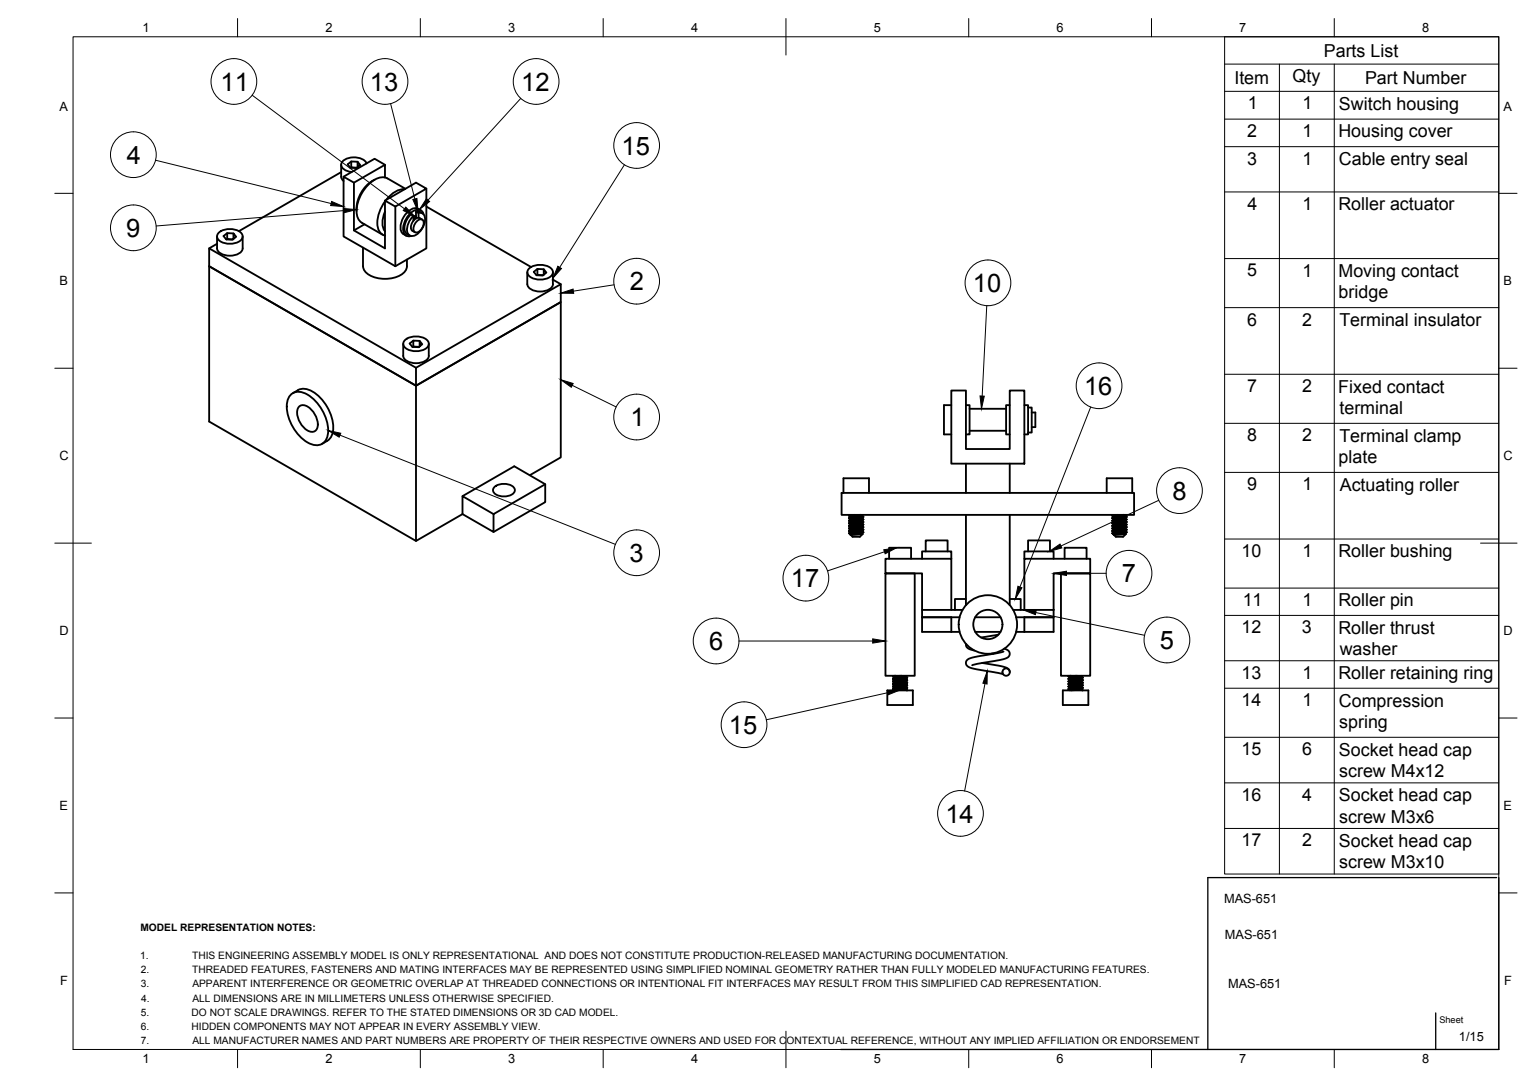
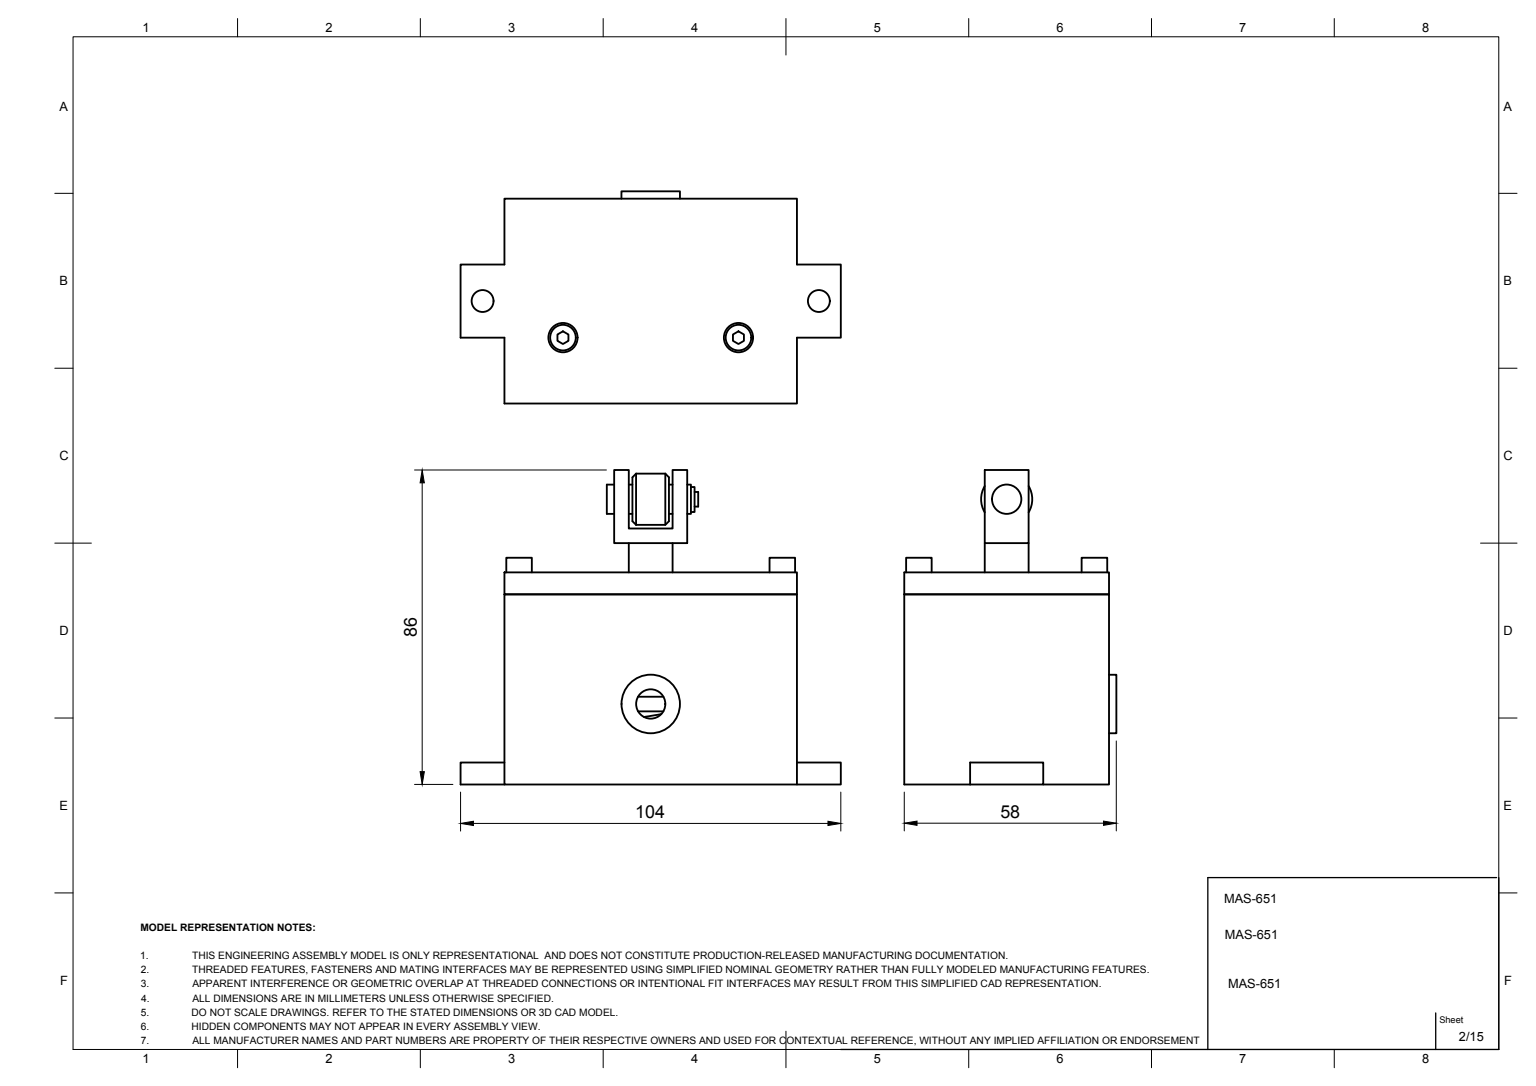
ISO-10303-21;
HEADER;
/* Generated by software containing ST-Developer
 * from STEP Tools, Inc. (www.steptools.com) 
 */

FILE_DESCRIPTION(
/* description */ ('Independent direct-acting normally-closed roller-plunger limit-switch
 CAD. Removable cover, insulated terminal supports, captured bus/conta
ct bridge, native Coil return spring, integral lower travel stop, reus
able instanced hardware and free roller. Manual geometric contact open
ing4mm; no snap-action/contact-force, electrical/current/voltage, envi
ronmental seal, safety-switch, wear, load or life certification. Exter
nal wiring and anchors omitted; fits and application engineering requi
red.'),
/* implementation_level */ '2;1');

FILE_NAME(
/* name */ 'MAS-651.step',
/* time_stamp */ '2026-11-08T07:32:43-08:00',
/* author */ (''),
/* organization */ (''),
/* preprocessor_version */ 'ST-DEVELOPER v20.2',
/* originating_system */ 'Autodesk Translation Framework v15.17.0.0',
/* authorisation */ '');

FILE_SCHEMA (('AUTOMOTIVE_DESIGN { 1 0 10303 214 3 1 1 }'));
ENDSEC;

DATA;
#10=MECHANICAL_DESIGN_GEOMETRIC_PRESENTATION_REPRESENTATION('',(#176,#177,
#178,#179,#180,#181,#182,#183,#184,#185,#186,#187,#188,#189,#190,#191,#192),
#36482);
#11=ITEM_DEFINED_TRANSFORMATION($,$,#9973,#10659);
#12=ITEM_DEFINED_TRANSFORMATION($,$,#10172,#10660);
#13=ITEM_DEFINED_TRANSFORMATION($,$,#10194,#10661);
#14=ITEM_DEFINED_TRANSFORMATION($,$,#10207,#10662);
#15=ITEM_DEFINED_TRANSFORMATION($,$,#10284,#10663);
#16=ITEM_DEFINED_TRANSFORMATION($,$,#10314,#10664);
#17=ITEM_DEFINED_TRANSFORMATION($,$,#10401,#10665);
#18=ITEM_DEFINED_TRANSFORMATION($,$,#10443,#10666);
#19=ITEM_DEFINED_TRANSFORMATION($,$,#10297,#10667);
#20=ITEM_DEFINED_TRANSFORMATION($,$,#10314,#10668);
#21=ITEM_DEFINED_TRANSFORMATION($,$,#10401,#10669);
#22=ITEM_DEFINED_TRANSFORMATION($,$,#10443,#10670);
#23=ITEM_DEFINED_TRANSFORMATION($,$,#10453,#10671);
#24=ITEM_DEFINED_TRANSFORMATION($,$,#10462,#10672);
#25=ITEM_DEFINED_TRANSFORMATION($,$,#10496,#10673);
#26=ITEM_DEFINED_TRANSFORMATION($,$,#10480,#10674);
#27=ITEM_DEFINED_TRANSFORMATION($,$,#10491,#10675);
#28=ITEM_DEFINED_TRANSFORMATION($,$,#10496,#10676);
#29=ITEM_DEFINED_TRANSFORMATION($,$,#10496,#10677);
#30=ITEM_DEFINED_TRANSFORMATION($,$,#10505,#10678);
#31=ITEM_DEFINED_TRANSFORMATION($,$,#10559,#10679);
#32=ITEM_DEFINED_TRANSFORMATION($,$,#10601,#10680);
#33=ITEM_DEFINED_TRANSFORMATION($,$,#10505,#10681);
#34=ITEM_DEFINED_TRANSFORMATION($,$,#10505,#10682);
#35=ITEM_DEFINED_TRANSFORMATION($,$,#10505,#10683);
#36=ITEM_DEFINED_TRANSFORMATION($,$,#10505,#10684);
#37=ITEM_DEFINED_TRANSFORMATION($,$,#10505,#10685);
#38=ITEM_DEFINED_TRANSFORMATION($,$,#10559,#10686);
#39=ITEM_DEFINED_TRANSFORMATION($,$,#10559,#10687);
#40=ITEM_DEFINED_TRANSFORMATION($,$,#10559,#10688);
#41=ITEM_DEFINED_TRANSFORMATION($,$,#10601,#10689);
#42=(
REPRESENTATION_RELATIONSHIP($,$,#36555,#36554)
REPRESENTATION_RELATIONSHIP_WITH_TRANSFORMATION(#11)
SHAPE_REPRESENTATION_RELATIONSHIP()
);
#43=(
REPRESENTATION_RELATIONSHIP($,$,#36556,#36554)
REPRESENTATION_RELATIONSHIP_WITH_TRANSFORMATION(#12)
SHAPE_REPRESENTATION_RELATIONSHIP()
);
#44=(
REPRESENTATION_RELATIONSHIP($,$,#36557,#36554)
REPRESENTATION_RELATIONSHIP_WITH_TRANSFORMATION(#13)
SHAPE_REPRESENTATION_RELATIONSHIP()
);
#45=(
REPRESENTATION_RELATIONSHIP($,$,#36558,#36554)
REPRESENTATION_RELATIONSHIP_WITH_TRANSFORMATION(#14)
SHAPE_REPRESENTATION_RELATIONSHIP()
);
#46=(
REPRESENTATION_RELATIONSHIP($,$,#36559,#36554)
REPRESENTATION_RELATIONSHIP_WITH_TRANSFORMATION(#15)
SHAPE_REPRESENTATION_RELATIONSHIP()
);
#47=(
REPRESENTATION_RELATIONSHIP($,$,#36561,#36554)
REPRESENTATION_RELATIONSHIP_WITH_TRANSFORMATION(#16)
SHAPE_REPRESENTATION_RELATIONSHIP()
);
#48=(
REPRESENTATION_RELATIONSHIP($,$,#36562,#36554)
REPRESENTATION_RELATIONSHIP_WITH_TRANSFORMATION(#17)
SHAPE_REPRESENTATION_RELATIONSHIP()
);
#49=(
REPRESENTATION_RELATIONSHIP($,$,#36563,#36554)
REPRESENTATION_RELATIONSHIP_WITH_TRANSFORMATION(#18)
SHAPE_REPRESENTATION_RELATIONSHIP()
);
#50=(
REPRESENTATION_RELATIONSHIP($,$,#36560,#36554)
REPRESENTATION_RELATIONSHIP_WITH_TRANSFORMATION(#19)
SHAPE_REPRESENTATION_RELATIONSHIP()
);
#51=(
REPRESENTATION_RELATIONSHIP($,$,#36561,#36554)
REPRESENTATION_RELATIONSHIP_WITH_TRANSFORMATION(#20)
SHAPE_REPRESENTATION_RELATIONSHIP()
);
#52=(
REPRESENTATION_RELATIONSHIP($,$,#36562,#36554)
REPRESENTATION_RELATIONSHIP_WITH_TRANSFORMATION(#21)
SHAPE_REPRESENTATION_RELATIONSHIP()
);
#53=(
REPRESENTATION_RELATIONSHIP($,$,#36563,#36554)
REPRESENTATION_RELATIONSHIP_WITH_TRANSFORMATION(#22)
SHAPE_REPRESENTATION_RELATIONSHIP()
);
#54=(
REPRESENTATION_RELATIONSHIP($,$,#36564,#36554)
REPRESENTATION_RELATIONSHIP_WITH_TRANSFORMATION(#23)
SHAPE_REPRESENTATION_RELATIONSHIP()
);
#55=(
REPRESENTATION_RELATIONSHIP($,$,#36565,#36554)
REPRESENTATION_RELATIONSHIP_WITH_TRANSFORMATION(#24)
SHAPE_REPRESENTATION_RELATIONSHIP()
);
#56=(
REPRESENTATION_RELATIONSHIP($,$,#36568,#36554)
REPRESENTATION_RELATIONSHIP_WITH_TRANSFORMATION(#25)
SHAPE_REPRESENTATION_RELATIONSHIP()
);
#57=(
REPRESENTATION_RELATIONSHIP($,$,#36566,#36554)
REPRESENTATION_RELATIONSHIP_WITH_TRANSFORMATION(#26)
SHAPE_REPRESENTATION_RELATIONSHIP()
);
#58=(
REPRESENTATION_RELATIONSHIP($,$,#36567,#36554)
REPRESENTATION_RELATIONSHIP_WITH_TRANSFORMATION(#27)
SHAPE_REPRESENTATION_RELATIONSHIP()
);
#59=(
REPRESENTATION_RELATIONSHIP($,$,#36568,#36554)
REPRESENTATION_RELATIONSHIP_WITH_TRANSFORMATION(#28)
SHAPE_REPRESENTATION_RELATIONSHIP()
);
#60=(
REPRESENTATION_RELATIONSHIP($,$,#36568,#36554)
REPRESENTATION_RELATIONSHIP_WITH_TRANSFORMATION(#29)
SHAPE_REPRESENTATION_RELATIONSHIP()
);
#61=(
REPRESENTATION_RELATIONSHIP($,$,#36569,#36554)
REPRESENTATION_RELATIONSHIP_WITH_TRANSFORMATION(#30)
SHAPE_REPRESENTATION_RELATIONSHIP()
);
#62=(
REPRESENTATION_RELATIONSHIP($,$,#36570,#36554)
REPRESENTATION_RELATIONSHIP_WITH_TRANSFORMATION(#31)
SHAPE_REPRESENTATION_RELATIONSHIP()
);
#63=(
REPRESENTATION_RELATIONSHIP($,$,#36571,#36554)
REPRESENTATION_RELATIONSHIP_WITH_TRANSFORMATION(#32)
SHAPE_REPRESENTATION_RELATIONSHIP()
);
#64=(
REPRESENTATION_RELATIONSHIP($,$,#36569,#36554)
REPRESENTATION_RELATIONSHIP_WITH_TRANSFORMATION(#33)
SHAPE_REPRESENTATION_RELATIONSHIP()
);
#65=(
REPRESENTATION_RELATIONSHIP($,$,#36569,#36554)
REPRESENTATION_RELATIONSHIP_WITH_TRANSFORMATION(#34)
SHAPE_REPRESENTATION_RELATIONSHIP()
);
#66=(
REPRESENTATION_RELATIONSHIP($,$,#36569,#36554)
REPRESENTATION_RELATIONSHIP_WITH_TRANSFORMATION(#35)
SHAPE_REPRESENTATION_RELATIONSHIP()
);
#67=(
REPRESENTATION_RELATIONSHIP($,$,#36569,#36554)
REPRESENTATION_RELATIONSHIP_WITH_TRANSFORMATION(#36)
SHAPE_REPRESENTATION_RELATIONSHIP()
);
#68=(
REPRESENTATION_RELATIONSHIP($,$,#36569,#36554)
REPRESENTATION_RELATIONSHIP_WITH_TRANSFORMATION(#37)
SHAPE_REPRESENTATION_RELATIONSHIP()
);
#69=(
REPRESENTATION_RELATIONSHIP($,$,#36570,#36554)
REPRESENTATION_RELATIONSHIP_WITH_TRANSFORMATION(#38)
SHAPE_REPRESENTATION_RELATIONSHIP()
);
#70=(
REPRESENTATION_RELATIONSHIP($,$,#36570,#36554)
REPRESENTATION_RELATIONSHIP_WITH_TRANSFORMATION(#39)
SHAPE_REPRESENTATION_RELATIONSHIP()
);
#71=(
REPRESENTATION_RELATIONSHIP($,$,#36570,#36554)
REPRESENTATION_RELATIONSHIP_WITH_TRANSFORMATION(#40)
SHAPE_REPRESENTATION_RELATIONSHIP()
);
#72=(
REPRESENTATION_RELATIONSHIP($,$,#36571,#36554)
REPRESENTATION_RELATIONSHIP_WITH_TRANSFORMATION(#41)
SHAPE_REPRESENTATION_RELATIONSHIP()
);
#73=CONTEXT_DEPENDENT_SHAPE_REPRESENTATION(#42,#36523);
#74=CONTEXT_DEPENDENT_SHAPE_REPRESENTATION(#43,#36524);
#75=CONTEXT_DEPENDENT_SHAPE_REPRESENTATION(#44,#36525);
#76=CONTEXT_DEPENDENT_SHAPE_REPRESENTATION(#45,#36526);
#77=CONTEXT_DEPENDENT_SHAPE_REPRESENTATION(#46,#36527);
#78=CONTEXT_DEPENDENT_SHAPE_REPRESENTATION(#47,#36528);
#79=CONTEXT_DEPENDENT_SHAPE_REPRESENTATION(#48,#36529);
#80=CONTEXT_DEPENDENT_SHAPE_REPRESENTATION(#49,#36530);
#81=CONTEXT_DEPENDENT_SHAPE_REPRESENTATION(#50,#36531);
#82=CONTEXT_DEPENDENT_SHAPE_REPRESENTATION(#51,#36532);
#83=CONTEXT_DEPENDENT_SHAPE_REPRESENTATION(#52,#36533);
#84=CONTEXT_DEPENDENT_SHAPE_REPRESENTATION(#53,#36534);
#85=CONTEXT_DEPENDENT_SHAPE_REPRESENTATION(#54,#36535);
#86=CONTEXT_DEPENDENT_SHAPE_REPRESENTATION(#55,#36536);
#87=CONTEXT_DEPENDENT_SHAPE_REPRESENTATION(#56,#36537);
#88=CONTEXT_DEPENDENT_SHAPE_REPRESENTATION(#57,#36538);
#89=CONTEXT_DEPENDENT_SHAPE_REPRESENTATION(#58,#36539);
#90=CONTEXT_DEPENDENT_SHAPE_REPRESENTATION(#59,#36540);
#91=CONTEXT_DEPENDENT_SHAPE_REPRESENTATION(#60,#36541);
#92=CONTEXT_DEPENDENT_SHAPE_REPRESENTATION(#61,#36542);
#93=CONTEXT_DEPENDENT_SHAPE_REPRESENTATION(#62,#36543);
#94=CONTEXT_DEPENDENT_SHAPE_REPRESENTATION(#63,#36544);
#95=CONTEXT_DEPENDENT_SHAPE_REPRESENTATION(#64,#36545);
#96=CONTEXT_DEPENDENT_SHAPE_REPRESENTATION(#65,#36546);
#97=CONTEXT_DEPENDENT_SHAPE_REPRESENTATION(#66,#36547);
#98=CONTEXT_DEPENDENT_SHAPE_REPRESENTATION(#67,#36548);
#99=CONTEXT_DEPENDENT_SHAPE_REPRESENTATION(#68,#36549);
#100=CONTEXT_DEPENDENT_SHAPE_REPRESENTATION(#69,#36550);
#101=CONTEXT_DEPENDENT_SHAPE_REPRESENTATION(#70,#36551);
#102=CONTEXT_DEPENDENT_SHAPE_REPRESENTATION(#71,#36552);
#103=CONTEXT_DEPENDENT_SHAPE_REPRESENTATION(#72,#36553);
#104=NEXT_ASSEMBLY_USAGE_OCCURRENCE('Switch housing:1',
'Switch housing:1','Switch housing:1',#36573,#36574,'Switch housing:1');
#105=NEXT_ASSEMBLY_USAGE_OCCURRENCE('Housing cover:1','Housing cover:1',
'Housing cover:1',#36573,#36575,'Housing cover:1');
#106=NEXT_ASSEMBLY_USAGE_OCCURRENCE('Cable entry seal:1',
'Cable entry seal:1','Cable entry seal:1',#36573,#36576,
'Cable entry seal:1');
#107=NEXT_ASSEMBLY_USAGE_OCCURRENCE('Roller actuator:1',
'Roller actuator:1','Roller actuator:1',#36573,#36577,
'Roller actuator:1');
#108=NEXT_ASSEMBLY_USAGE_OCCURRENCE('Moving contact bridge:1',
'Moving contact bridge:1','Moving contact bridge:1',#36573,#36578,
'Moving contact bridge:1');
#109=NEXT_ASSEMBLY_USAGE_OCCURRENCE('Terminal insulator:1',
'Terminal insulator:1','Terminal insulator:1',#36573,#36580,
'Terminal insulator:1');
#110=NEXT_ASSEMBLY_USAGE_OCCURRENCE('Fixed contact terminal:1',
'Fixed contact terminal:1','Fixed contact terminal:1',#36573,#36581,
'Fixed contact terminal:1');
#111=NEXT_ASSEMBLY_USAGE_OCCURRENCE('Terminal clamp plate:1',
'Terminal clamp plate:1','Terminal clamp plate:1',#36573,#36582,
'Terminal clamp plate:1');
#112=NEXT_ASSEMBLY_USAGE_OCCURRENCE('Actuating roller:1',
'Actuating roller:1','Actuating roller:1',#36573,#36579,
'Actuating roller:1');
#113=NEXT_ASSEMBLY_USAGE_OCCURRENCE('Terminal insulator:2',
'Terminal insulator:2','Terminal insulator:2',#36573,#36580,
'Terminal insulator:2');
#114=NEXT_ASSEMBLY_USAGE_OCCURRENCE('Fixed contact terminal:2',
'Fixed contact terminal:2','Fixed contact terminal:2',#36573,#36581,
'Fixed contact terminal:2');
#115=NEXT_ASSEMBLY_USAGE_OCCURRENCE('Terminal clamp plate:2',
'Terminal clamp plate:2','Terminal clamp plate:2',#36573,#36582,
'Terminal clamp plate:2');
#116=NEXT_ASSEMBLY_USAGE_OCCURRENCE('Roller bushing:1',
'Roller bushing:1','Roller bushing:1',#36573,#36583,'Roller bushing:1');
#117=NEXT_ASSEMBLY_USAGE_OCCURRENCE('Roller pin:1','Roller pin:1',
'Roller pin:1',#36573,#36584,'Roller pin:1');
#118=NEXT_ASSEMBLY_USAGE_OCCURRENCE('Roller thrust washer:1',
'Roller thrust washer:1','Roller thrust washer:1',#36573,#36587,
'Roller thrust washer:1');
#119=NEXT_ASSEMBLY_USAGE_OCCURRENCE('Roller retaining ring:1',
'Roller retaining ring:1','Roller retaining ring:1',#36573,#36585,
'Roller retaining ring:1');
#120=NEXT_ASSEMBLY_USAGE_OCCURRENCE('Compression spring:1',
'Compression spring:1','Compression spring:1',#36573,#36586,
'Compression spring:1');
#121=NEXT_ASSEMBLY_USAGE_OCCURRENCE('Roller thrust washer:2',
'Roller thrust washer:2','Roller thrust washer:2',#36573,#36587,
'Roller thrust washer:2');
#122=NEXT_ASSEMBLY_USAGE_OCCURRENCE('Roller thrust washer:3',
'Roller thrust washer:3','Roller thrust washer:3',#36573,#36587,
'Roller thrust washer:3');
#123=NEXT_ASSEMBLY_USAGE_OCCURRENCE('Socket head cap screw M4x12:1',
'Socket head cap screw M4x12:1','Socket head cap screw M4x12:1',#36573,
#36588,'Socket head cap screw M4x12:1');
#124=NEXT_ASSEMBLY_USAGE_OCCURRENCE('Socket head cap screw M3x6:1',
'Socket head cap screw M3x6:1','Socket head cap screw M3x6:1',#36573,#36589,
'Socket head cap screw M3x6:1');
#125=NEXT_ASSEMBLY_USAGE_OCCURRENCE('Socket head cap screw M3x10:1',
'Socket head cap screw M3x10:1','Socket head cap screw M3x10:1',#36573,
#36590,'Socket head cap screw M3x10:1');
#126=NEXT_ASSEMBLY_USAGE_OCCURRENCE('Socket head cap screw M4x12:2',
'Socket head cap screw M4x12:2','Socket head cap screw M4x12:2',#36573,
#36588,'Socket head cap screw M4x12:2');
#127=NEXT_ASSEMBLY_USAGE_OCCURRENCE('Socket head cap screw M4x12:3',
'Socket head cap screw M4x12:3','Socket head cap screw M4x12:3',#36573,
#36588,'Socket head cap screw M4x12:3');
#128=NEXT_ASSEMBLY_USAGE_OCCURRENCE('Socket head cap screw M4x12:4',
'Socket head cap screw M4x12:4','Socket head cap screw M4x12:4',#36573,
#36588,'Socket head cap screw M4x12:4');
#129=NEXT_ASSEMBLY_USAGE_OCCURRENCE('Socket head cap screw M4x12:5',
'Socket head cap screw M4x12:5','Socket head cap screw M4x12:5',#36573,
#36588,'Socket head cap screw M4x12:5');
#130=NEXT_ASSEMBLY_USAGE_OCCURRENCE('Socket head cap screw M4x12:6',
'Socket head cap screw M4x12:6','Socket head cap screw M4x12:6',#36573,
#36588,'Socket head cap screw M4x12:6');
#131=NEXT_ASSEMBLY_USAGE_OCCURRENCE('Socket head cap screw M3x6:2',
'Socket head cap screw M3x6:2','Socket head cap screw M3x6:2',#36573,#36589,
'Socket head cap screw M3x6:2');
#132=NEXT_ASSEMBLY_USAGE_OCCURRENCE('Socket head cap screw M3x6:3',
'Socket head cap screw M3x6:3','Socket head cap screw M3x6:3',#36573,#36589,
'Socket head cap screw M3x6:3');
#133=NEXT_ASSEMBLY_USAGE_OCCURRENCE('Socket head cap screw M3x6:4',
'Socket head cap screw M3x6:4','Socket head cap screw M3x6:4',#36573,#36589,
'Socket head cap screw M3x6:4');
#134=NEXT_ASSEMBLY_USAGE_OCCURRENCE('Socket head cap screw M3x10:2',
'Socket head cap screw M3x10:2','Socket head cap screw M3x10:2',#36573,
#36590,'Socket head cap screw M3x10:2');
#135=CONICAL_SURFACE('',#10298,0.65,0.785398163397448);
#136=CONICAL_SURFACE('',#10305,0.65,0.785398163397448);
#137=CONICAL_SURFACE('',#10309,0.35,0.785398163397448);
#138=CONICAL_SURFACE('',#10313,0.35,0.785398163397448);
#139=CONICAL_SURFACE('',#10540,0.15,0.785398163397449);
#140=CONICAL_SURFACE('',#10582,0.1,0.785398163397448);
#141=CONICAL_SURFACE('',#10640,0.1,0.785398163397448);
#142=SHAPE_REPRESENTATION_RELATIONSHIP('SRR','None',#36555,#159);
#143=SHAPE_REPRESENTATION_RELATIONSHIP('SRR','None',#36556,#160);
#144=SHAPE_REPRESENTATION_RELATIONSHIP('SRR','None',#36557,#161);
#145=SHAPE_REPRESENTATION_RELATIONSHIP('SRR','None',#36558,#162);
#146=SHAPE_REPRESENTATION_RELATIONSHIP('SRR','None',#36559,#163);
#147=SHAPE_REPRESENTATION_RELATIONSHIP('SRR','None',#36560,#164);
#148=SHAPE_REPRESENTATION_RELATIONSHIP('SRR','None',#36561,#165);
#149=SHAPE_REPRESENTATION_RELATIONSHIP('SRR','None',#36562,#166);
#150=SHAPE_REPRESENTATION_RELATIONSHIP('SRR','None',#36563,#167);
#151=SHAPE_REPRESENTATION_RELATIONSHIP('SRR','None',#36564,#168);
#152=SHAPE_REPRESENTATION_RELATIONSHIP('SRR','None',#36565,#169);
#153=SHAPE_REPRESENTATION_RELATIONSHIP('SRR','None',#36566,#170);
#154=SHAPE_REPRESENTATION_RELATIONSHIP('SRR','None',#36567,#171);
#155=SHAPE_REPRESENTATION_RELATIONSHIP('SRR','None',#36568,#172);
#156=SHAPE_REPRESENTATION_RELATIONSHIP('SRR','None',#36569,#173);
#157=SHAPE_REPRESENTATION_RELATIONSHIP('SRR','None',#36570,#174);
#158=SHAPE_REPRESENTATION_RELATIONSHIP('SRR','None',#36571,#175);
#159=ADVANCED_BREP_SHAPE_REPRESENTATION('',(#193),#36465);
#160=ADVANCED_BREP_SHAPE_REPRESENTATION('',(#194),#36466);
#161=ADVANCED_BREP_SHAPE_REPRESENTATION('',(#195),#36467);
#162=ADVANCED_BREP_SHAPE_REPRESENTATION('',(#196),#36468);
#163=ADVANCED_BREP_SHAPE_REPRESENTATION('',(#197),#36469);
#164=ADVANCED_BREP_SHAPE_REPRESENTATION('',(#198),#36470);
#165=ADVANCED_BREP_SHAPE_REPRESENTATION('',(#199),#36471);
#166=ADVANCED_BREP_SHAPE_REPRESENTATION('',(#200),#36472);
#167=ADVANCED_BREP_SHAPE_REPRESENTATION('',(#201),#36473);
#168=ADVANCED_BREP_SHAPE_REPRESENTATION('',(#202),#36474);
#169=ADVANCED_BREP_SHAPE_REPRESENTATION('',(#203),#36475);
#170=ADVANCED_BREP_SHAPE_REPRESENTATION('',(#204),#36476);
#171=ADVANCED_BREP_SHAPE_REPRESENTATION('',(#205),#36477);
#172=ADVANCED_BREP_SHAPE_REPRESENTATION('',(#206),#36478);
#173=ADVANCED_BREP_SHAPE_REPRESENTATION('',(#207),#36479);
#174=ADVANCED_BREP_SHAPE_REPRESENTATION('',(#208),#36480);
#175=ADVANCED_BREP_SHAPE_REPRESENTATION('',(#209),#36481);
#176=STYLED_ITEM('',(#36649),#193);
#177=STYLED_ITEM('',(#36650),#194);
#178=STYLED_ITEM('',(#36651),#195);
#179=STYLED_ITEM('',(#36652),#196);
#180=STYLED_ITEM('',(#36653),#197);
#181=STYLED_ITEM('',(#36654),#198);
#182=STYLED_ITEM('',(#36655),#199);
#183=STYLED_ITEM('',(#36653),#200);
#184=STYLED_ITEM('',(#36656),#201);
#185=STYLED_ITEM('',(#36657),#202);
#186=STYLED_ITEM('',(#36658),#203);
#187=STYLED_ITEM('',(#36659),#204);
#188=STYLED_ITEM('',(#36660),#205);
#189=STYLED_ITEM('',(#36661),#206);
#190=STYLED_ITEM('',(#36659),#207);
#191=STYLED_ITEM('',(#36659),#208);
#192=STYLED_ITEM('',(#36659),#209);
#193=MANIFOLD_SOLID_BREP('Body1',#9767);
#194=MANIFOLD_SOLID_BREP('Body1',#9768);
#195=MANIFOLD_SOLID_BREP('Body1',#9769);
#196=MANIFOLD_SOLID_BREP('Body1',#9770);
#197=MANIFOLD_SOLID_BREP('Body1',#9771);
#198=MANIFOLD_SOLID_BREP('Roller',#9772);
#199=MANIFOLD_SOLID_BREP('Body1',#9773);
#200=MANIFOLD_SOLID_BREP('Body1',#9774);
#201=MANIFOLD_SOLID_BREP('Body1',#9775);
#202=MANIFOLD_SOLID_BREP('Body1',#9776);
#203=MANIFOLD_SOLID_BREP('Body1',#9777);
#204=MANIFOLD_SOLID_BREP('Body1',#9778);
#205=MANIFOLD_SOLID_BREP('Body1',#9779);
#206=MANIFOLD_SOLID_BREP('Body1',#9780);
#207=MANIFOLD_SOLID_BREP('Body1',#9781);
#208=MANIFOLD_SOLID_BREP('Body1',#9782);
#209=MANIFOLD_SOLID_BREP('Body1',#9783);
#210=B_SPLINE_SURFACE_WITH_KNOTS('',3,3,((#16536,#16537,#16538,#16539,#16540,
#16541,#16542,#16543,#16544,#16545,#16546,#16547,#16548,#16549,#16550,#16551,
#16552,#16553,#16554,#16555,#16556,#16557,#16558,#16559,#16560,#16561,#16562,
#16563,#16564,#16565,#16566,#16567,#16568,#16569,#16570,#16571,#16572,#16573,
#16574,#16575,#16576,#16577,#16578,#16579,#16580,#16581,#16582,#16583,#16584,
#16585,#16586,#16587,#16588,#16589,#16590,#16591,#16592,#16593,#16594,#16595,
#16596,#16597,#16598,#16599,#16600,#16601,#16602,#16603,#16604,#16605,#16606,
#16607,#16608,#16609,#16610,#16611,#16612,#16613,#16614,#16615,#16616,#16617,
#16618,#16619,#16620,#16621),(#16622,#16623,#16624,#16625,#16626,#16627,
#16628,#16629,#16630,#16631,#16632,#16633,#16634,#16635,#16636,#16637,#16638,
#16639,#16640,#16641,#16642,#16643,#16644,#16645,#16646,#16647,#16648,#16649,
#16650,#16651,#16652,#16653,#16654,#16655,#16656,#16657,#16658,#16659,#16660,
#16661,#16662,#16663,#16664,#16665,#16666,#16667,#16668,#16669,#16670,#16671,
#16672,#16673,#16674,#16675,#16676,#16677,#16678,#16679,#16680,#16681,#16682,
#16683,#16684,#16685,#16686,#16687,#16688,#16689,#16690,#16691,#16692,#16693,
#16694,#16695,#16696,#16697,#16698,#16699,#16700,#16701,#16702,#16703,#16704,
#16705,#16706,#16707),(#16708,#16709,#16710,#16711,#16712,#16713,#16714,
#16715,#16716,#16717,#16718,#16719,#16720,#16721,#16722,#16723,#16724,#16725,
#16726,#16727,#16728,#16729,#16730,#16731,#16732,#16733,#16734,#16735,#16736,
#16737,#16738,#16739,#16740,#16741,#16742,#16743,#16744,#16745,#16746,#16747,
#16748,#16749,#16750,#16751,#16752,#16753,#16754,#16755,#16756,#16757,#16758,
#16759,#16760,#16761,#16762,#16763,#16764,#16765,#16766,#16767,#16768,#16769,
#16770,#16771,#16772,#16773,#16774,#16775,#16776,#16777,#16778,#16779,#16780,
#16781,#16782,#16783,#16784,#16785,#16786,#16787,#16788,#16789,#16790,#16791,
#16792,#16793),(#16794,#16795,#16796,#16797,#16798,#16799,#16800,#16801,
#16802,#16803,#16804,#16805,#16806,#16807,#16808,#16809,#16810,#16811,#16812,
#16813,#16814,#16815,#16816,#16817,#16818,#16819,#16820,#16821,#16822,#16823,
#16824,#16825,#16826,#16827,#16828,#16829,#16830,#16831,#16832,#16833,#16834,
#16835,#16836,#16837,#16838,#16839,#16840,#16841,#16842,#16843,#16844,#16845,
#16846,#16847,#16848,#16849,#16850,#16851,#16852,#16853,#16854,#16855,#16856,
#16857,#16858,#16859,#16860,#16861,#16862,#16863,#16864,#16865,#16866,#16867,
#16868,#16869,#16870,#16871,#16872,#16873,#16874,#16875,#16876,#16877,#16878,
#16879)),.UNSPECIFIED.,.F.,.F.,.F.,(4,4),(4,1,1,1,1,1,1,1,1,1,1,1,1,1,1,
1,1,1,1,1,1,1,1,1,1,1,1,1,1,1,1,1,1,1,1,1,1,1,1,1,1,1,1,1,1,1,1,1,1,1,1,
1,1,1,1,1,1,1,1,1,1,1,1,1,1,1,1,1,1,1,1,1,1,1,1,1,1,1,1,1,1,1,1,4),(0.,
0.0448889834294937),(11.8615800042567,12.8591513772396,13.8567227502226,
14.8542941232055,15.8518654961884,16.8494368691714,17.8470082421543,18.8445796151372,
19.8421509881202,20.8397223611031,21.837293734086,22.834865107069,23.8324364800519,
24.8300078530348,25.8275792260178,26.8251505990007,27.8227219719836,28.8202933449666,
29.8178647179495,30.8154360909324,31.8130074639154,32.8105788368983,33.8081502098812,
34.8057215828642,35.8032929558471,36.80086432883,37.798435701813,38.7960070747959,
39.7935784477789,40.7911498207618,41.7887211937447,42.7862925667277,43.7838639397106,
44.7814353126935,45.7790066856765,46.7765780586594,47.7741494316423,48.7717208046253,
49.7692921776082,50.7668635505911,51.7644349235741,52.762006296557,53.7595776695399,
54.7571490425229,55.7547204155058,56.7522917884887,57.7498631614717,58.7474345344546,
59.7450059074375,60.7425772804205,61.7401486534034,62.7377200263864,63.7352913993693,
64.7328627723522,65.7304341453352,66.7280055183181,67.725576891301,68.723148264284,
69.7207196372669,70.7182910102498,71.7158623832328,72.7134337562157,73.7110051291986,
74.7085765021816,75.7061478751645,76.7037192481474,77.7012906211304,78.6988619941133,
79.6964333670962,80.6940047400792,81.6915761130621,82.689147486045,83.686718859028,
84.6842902320109,85.6818616049939,86.6794329779768,87.6770043509597,88.6745757239427,
89.6721470969256,90.6697184699085,91.6672898428915,92.6648612158744,93.6624325888573,
94.6600039618403),.UNSPECIFIED.);
#211=B_SPLINE_SURFACE_WITH_KNOTS('',3,3,((#16957,#16958,#16959,#16960,#16961,
#16962,#16963,#16964,#16965,#16966,#16967,#16968,#16969,#16970,#16971,#16972,
#16973,#16974,#16975,#16976,#16977,#16978,#16979,#16980,#16981,#16982,#16983,
#16984,#16985,#16986,#16987,#16988,#16989,#16990,#16991,#16992,#16993,#16994,
#16995,#16996,#16997,#16998,#16999,#17000,#17001,#17002,#17003,#17004,#17005,
#17006,#17007,#17008,#17009,#17010,#17011,#17012,#17013,#17014,#17015,#17016,
#17017,#17018,#17019,#17020,#17021,#17022,#17023,#17024,#17025,#17026,#17027,
#17028,#17029,#17030,#17031,#17032,#17033,#17034,#17035,#17036,#17037,#17038,
#17039,#17040,#17041,#17042),(#17043,#17044,#17045,#17046,#17047,#17048,
#17049,#17050,#17051,#17052,#17053,#17054,#17055,#17056,#17057,#17058,#17059,
#17060,#17061,#17062,#17063,#17064,#17065,#17066,#17067,#17068,#17069,#17070,
#17071,#17072,#17073,#17074,#17075,#17076,#17077,#17078,#17079,#17080,#17081,
#17082,#17083,#17084,#17085,#17086,#17087,#17088,#17089,#17090,#17091,#17092,
#17093,#17094,#17095,#17096,#17097,#17098,#17099,#17100,#17101,#17102,#17103,
#17104,#17105,#17106,#17107,#17108,#17109,#17110,#17111,#17112,#17113,#17114,
#17115,#17116,#17117,#17118,#17119,#17120,#17121,#17122,#17123,#17124,#17125,
#17126,#17127,#17128),(#17129,#17130,#17131,#17132,#17133,#17134,#17135,
#17136,#17137,#17138,#17139,#17140,#17141,#17142,#17143,#17144,#17145,#17146,
#17147,#17148,#17149,#17150,#17151,#17152,#17153,#17154,#17155,#17156,#17157,
#17158,#17159,#17160,#17161,#17162,#17163,#17164,#17165,#17166,#17167,#17168,
#17169,#17170,#17171,#17172,#17173,#17174,#17175,#17176,#17177,#17178,#17179,
#17180,#17181,#17182,#17183,#17184,#17185,#17186,#17187,#17188,#17189,#17190,
#17191,#17192,#17193,#17194,#17195,#17196,#17197,#17198,#17199,#17200,#17201,
#17202,#17203,#17204,#17205,#17206,#17207,#17208,#17209,#17210,#17211,#17212,
#17213,#17214),(#17215,#17216,#17217,#17218,#17219,#17220,#17221,#17222,
#17223,#17224,#17225,#17226,#17227,#17228,#17229,#17230,#17231,#17232,#17233,
#17234,#17235,#17236,#17237,#17238,#17239,#17240,#17241,#17242,#17243,#17244,
#17245,#17246,#17247,#17248,#17249,#17250,#17251,#17252,#17253,#17254,#17255,
#17256,#17257,#17258,#17259,#17260,#17261,#17262,#17263,#17264,#17265,#17266,
#17267,#17268,#17269,#17270,#17271,#17272,#17273,#17274,#17275,#17276,#17277,
#17278,#17279,#17280,#17281,#17282,#17283,#17284,#17285,#17286,#17287,#17288,
#17289,#17290,#17291,#17292,#17293,#17294,#17295,#17296,#17297,#17298,#17299,
#17300)),.UNSPECIFIED.,.F.,.F.,.F.,(4,4),(4,1,1,1,1,1,1,1,1,1,1,1,1,1,1,
1,1,1,1,1,1,1,1,1,1,1,1,1,1,1,1,1,1,1,1,1,1,1,1,1,1,1,1,1,1,1,1,1,1,1,1,
1,1,1,1,1,1,1,1,1,1,1,1,1,1,1,1,1,1,1,1,1,1,1,1,1,1,1,1,1,1,1,1,4),(0.,
0.0448889834294937),(14.3981410127769,15.3957123857599,16.3932837587428,
17.3908551317257,18.3884265047087,19.3859978776916,20.3835692506745,21.3811406236575,
22.3787119966404,23.3762833696233,24.3738547426063,25.3714261155892,26.3689974885721,
27.3665688615551,28.364140234538,29.3617116075209,30.3592829805039,31.3568543534868,
32.3544257264697,33.3519970994527,34.3495684724356,35.3471398454185,36.3447112184015,
37.3422825913844,38.3398539643674,39.3374253373503,40.3349967103332,41.3325680833162,
42.3301394562991,43.327710829282,44.325282202265,45.3228535752479,46.3204249482308,
47.3179963212138,48.3155676941967,49.3131390671796,50.3107104401626,51.3082818131455,
52.3058531861284,53.3034245591114,54.3009959320943,55.2985673050772,56.2961386780602,
57.2937100510431,58.291281424026,59.288852797009,60.2864241699919,61.2839955429748,
62.2815669159578,63.2791382889407,64.2767096619236,65.2742810349066,66.2718524078895,
67.2694237808725,68.2669951538554,69.2645665268383,70.2621378998213,71.2597092728042,
72.2572806457871,73.2548520187701,74.252423391753,75.2499947647359,76.2475661377189,
77.2451375107018,78.2427088836847,79.2402802566677,80.2378516296506,81.2354230026336,
82.2329943756165,83.2305657485994,84.2281371215823,85.2257084945653,86.2232798675482,
87.2208512405312,88.2184226135141,89.215993986497,90.21356535948,91.2111367324629,
92.2087081054458,93.2062794784288,94.2038508514117,95.2014222243946,96.1989935973776,
97.1965649703605),.UNSPECIFIED.);
#212=B_SPLINE_SURFACE_WITH_KNOTS('',3,3,((#17509,#17510,#17511,#17512,#17513,
#17514,#17515,#17516,#17517,#17518,#17519,#17520,#17521,#17522,#17523,#17524,
#17525,#17526,#17527,#17528,#17529,#17530,#17531,#17532,#17533,#17534,#17535,
#17536,#17537,#17538,#17539,#17540,#17541,#17542,#17543,#17544,#17545,#17546,
#17547,#17548,#17549,#17550,#17551,#17552,#17553,#17554,#17555,#17556,#17557,
#17558,#17559,#17560,#17561,#17562,#17563,#17564,#17565,#17566,#17567,#17568,
#17569,#17570,#17571,#17572,#17573,#17574,#17575,#17576,#17577,#17578,#17579,
#17580,#17581,#17582,#17583,#17584,#17585,#17586,#17587,#17588,#17589,#17590,
#17591,#17592,#17593,#17594),(#17595,#17596,#17597,#17598,#17599,#17600,
#17601,#17602,#17603,#17604,#17605,#17606,#17607,#17608,#17609,#17610,#17611,
#17612,#17613,#17614,#17615,#17616,#17617,#17618,#17619,#17620,#17621,#17622,
#17623,#17624,#17625,#17626,#17627,#17628,#17629,#17630,#17631,#17632,#17633,
#17634,#17635,#17636,#17637,#17638,#17639,#17640,#17641,#17642,#17643,#17644,
#17645,#17646,#17647,#17648,#17649,#17650,#17651,#17652,#17653,#17654,#17655,
#17656,#17657,#17658,#17659,#17660,#17661,#17662,#17663,#17664,#17665,#17666,
#17667,#17668,#17669,#17670,#17671,#17672,#17673,#17674,#17675,#17676,#17677,
#17678,#17679,#17680),(#17681,#17682,#17683,#17684,#17685,#17686,#17687,
#17688,#17689,#17690,#17691,#17692,#17693,#17694,#17695,#17696,#17697,#17698,
#17699,#17700,#17701,#17702,#17703,#17704,#17705,#17706,#17707,#17708,#17709,
#17710,#17711,#17712,#17713,#17714,#17715,#17716,#17717,#17718,#17719,#17720,
#17721,#17722,#17723,#17724,#17725,#17726,#17727,#17728,#17729,#17730,#17731,
#17732,#17733,#17734,#17735,#17736,#17737,#17738,#17739,#17740,#17741,#17742,
#17743,#17744,#17745,#17746,#17747,#17748,#17749,#17750,#17751,#17752,#17753,
#17754,#17755,#17756,#17757,#17758,#17759,#17760,#17761,#17762,#17763,#17764,
#17765,#17766),(#17767,#17768,#17769,#17770,#17771,#17772,#17773,#17774,
#17775,#17776,#17777,#17778,#17779,#17780,#17781,#17782,#17783,#17784,#17785,
#17786,#17787,#17788,#17789,#17790,#17791,#17792,#17793,#17794,#17795,#17796,
#17797,#17798,#17799,#17800,#17801,#17802,#17803,#17804,#17805,#17806,#17807,
#17808,#17809,#17810,#17811,#17812,#17813,#17814,#17815,#17816,#17817,#17818,
#17819,#17820,#17821,#17822,#17823,#17824,#17825,#17826,#17827,#17828,#17829,
#17830,#17831,#17832,#17833,#17834,#17835,#17836,#17837,#17838,#17839,#17840,
#17841,#17842,#17843,#17844,#17845,#17846,#17847,#17848,#17849,#17850,#17851,
#17852)),.UNSPECIFIED.,.F.,.F.,.F.,(4,4),(4,1,1,1,1,1,1,1,1,1,1,1,1,1,1,
1,1,1,1,1,1,1,1,1,1,1,1,1,1,1,1,1,1,1,1,1,1,1,1,1,1,1,1,1,1,1,1,1,1,1,1,
1,1,1,1,1,1,1,1,1,1,1,1,1,1,1,1,1,1,1,1,1,1,1,1,1,1,1,1,1,1,1,1,4),(0.,
0.0448889834294937),(11.8615800042567,12.8591513772396,13.8567227502226,
14.8542941232055,15.8518654961884,16.8494368691714,17.8470082421543,18.8445796151372,
19.8421509881202,20.8397223611031,21.837293734086,22.834865107069,23.8324364800519,
24.8300078530348,25.8275792260178,26.8251505990007,27.8227219719836,28.8202933449666,
29.8178647179495,30.8154360909324,31.8130074639154,32.8105788368983,33.8081502098812,
34.8057215828642,35.8032929558471,36.80086432883,37.798435701813,38.7960070747959,
39.7935784477789,40.7911498207618,41.7887211937447,42.7862925667277,43.7838639397106,
44.7814353126935,45.7790066856765,46.7765780586594,47.7741494316423,48.7717208046253,
49.7692921776082,50.7668635505911,51.7644349235741,52.762006296557,53.7595776695399,
54.7571490425229,55.7547204155058,56.7522917884887,57.7498631614717,58.7474345344546,
59.7450059074375,60.7425772804205,61.7401486534034,62.7377200263864,63.7352913993693,
64.7328627723522,65.7304341453352,66.7280055183181,67.725576891301,68.723148264284,
69.7207196372669,70.7182910102498,71.7158623832328,72.7134337562157,73.7110051291986,
74.7085765021816,75.7061478751645,76.7037192481474,77.7012906211304,78.6988619941133,
79.6964333670962,80.6940047400792,81.6915761130621,82.689147486045,83.686718859028,
84.6842902320109,85.6818616049939,86.6794329779768,87.6770043509597,88.6745757239427,
89.6721470969256,90.6697184699085,91.6672898428915,92.6648612158744,93.6624325888573,
94.6600039618403),.UNSPECIFIED.);
#213=B_SPLINE_SURFACE_WITH_KNOTS('',3,3,((#17930,#17931,#17932,#17933,#17934,
#17935,#17936,#17937,#17938,#17939,#17940,#17941,#17942,#17943,#17944,#17945,
#17946,#17947,#17948,#17949,#17950,#17951,#17952,#17953,#17954,#17955,#17956,
#17957,#17958,#17959,#17960,#17961,#17962,#17963,#17964,#17965,#17966,#17967,
#17968,#17969,#17970,#17971,#17972,#17973,#17974,#17975,#17976,#17977,#17978,
#17979,#17980,#17981,#17982,#17983,#17984,#17985,#17986,#17987,#17988,#17989,
#17990,#17991,#17992,#17993,#17994,#17995,#17996,#17997,#17998,#17999,#18000,
#18001,#18002,#18003,#18004,#18005,#18006,#18007,#18008,#18009,#18010,#18011,
#18012,#18013,#18014,#18015),(#18016,#18017,#18018,#18019,#18020,#18021,
#18022,#18023,#18024,#18025,#18026,#18027,#18028,#18029,#18030,#18031,#18032,
#18033,#18034,#18035,#18036,#18037,#18038,#18039,#18040,#18041,#18042,#18043,
#18044,#18045,#18046,#18047,#18048,#18049,#18050,#18051,#18052,#18053,#18054,
#18055,#18056,#18057,#18058,#18059,#18060,#18061,#18062,#18063,#18064,#18065,
#18066,#18067,#18068,#18069,#18070,#18071,#18072,#18073,#18074,#18075,#18076,
#18077,#18078,#18079,#18080,#18081,#18082,#18083,#18084,#18085,#18086,#18087,
#18088,#18089,#18090,#18091,#18092,#18093,#18094,#18095,#18096,#18097,#18098,
#18099,#18100,#18101),(#18102,#18103,#18104,#18105,#18106,#18107,#18108,
#18109,#18110,#18111,#18112,#18113,#18114,#18115,#18116,#18117,#18118,#18119,
#18120,#18121,#18122,#18123,#18124,#18125,#18126,#18127,#18128,#18129,#18130,
#18131,#18132,#18133,#18134,#18135,#18136,#18137,#18138,#18139,#18140,#18141,
#18142,#18143,#18144,#18145,#18146,#18147,#18148,#18149,#18150,#18151,#18152,
#18153,#18154,#18155,#18156,#18157,#18158,#18159,#18160,#18161,#18162,#18163,
#18164,#18165,#18166,#18167,#18168,#18169,#18170,#18171,#18172,#18173,#18174,
#18175,#18176,#18177,#18178,#18179,#18180,#18181,#18182,#18183,#18184,#18185,
#18186,#18187),(#18188,#18189,#18190,#18191,#18192,#18193,#18194,#18195,
#18196,#18197,#18198,#18199,#18200,#18201,#18202,#18203,#18204,#18205,#18206,
#18207,#18208,#18209,#18210,#18211,#18212,#18213,#18214,#18215,#18216,#18217,
#18218,#18219,#18220,#18221,#18222,#18223,#18224,#18225,#18226,#18227,#18228,
#18229,#18230,#18231,#18232,#18233,#18234,#18235,#18236,#18237,#18238,#18239,
#18240,#18241,#18242,#18243,#18244,#18245,#18246,#18247,#18248,#18249,#18250,
#18251,#18252,#18253,#18254,#18255,#18256,#18257,#18258,#18259,#18260,#18261,
#18262,#18263,#18264,#18265,#18266,#18267,#18268,#18269,#18270,#18271,#18272,
#18273)),.UNSPECIFIED.,.F.,.F.,.F.,(4,4),(4,1,1,1,1,1,1,1,1,1,1,1,1,1,1,
1,1,1,1,1,1,1,1,1,1,1,1,1,1,1,1,1,1,1,1,1,1,1,1,1,1,1,1,1,1,1,1,1,1,1,1,
1,1,1,1,1,1,1,1,1,1,1,1,1,1,1,1,1,1,1,1,1,1,1,1,1,1,1,1,1,1,1,1,4),(0.,
0.0448889834294937),(14.3981410127769,15.3957123857599,16.3932837587428,
17.3908551317257,18.3884265047087,19.3859978776916,20.3835692506745,21.3811406236575,
22.3787119966404,23.3762833696233,24.3738547426063,25.3714261155892,26.3689974885721,
27.3665688615551,28.364140234538,29.3617116075209,30.3592829805039,31.3568543534868,
32.3544257264697,33.3519970994527,34.3495684724356,35.3471398454185,36.3447112184015,
37.3422825913844,38.3398539643674,39.3374253373503,40.3349967103332,41.3325680833162,
42.3301394562991,43.327710829282,44.325282202265,45.3228535752479,46.3204249482308,
47.3179963212138,48.3155676941967,49.3131390671796,50.3107104401626,51.3082818131455,
52.3058531861284,53.3034245591114,54.3009959320943,55.2985673050772,56.2961386780602,
57.2937100510431,58.291281424026,59.288852797009,60.2864241699919,61.2839955429748,
62.2815669159578,63.2791382889407,64.2767096619237,65.2742810349066,66.2718524078895,
67.2694237808725,68.2669951538554,69.2645665268383,70.2621378998213,71.2597092728042,
72.2572806457871,73.2548520187701,74.252423391753,75.2499947647359,76.2475661377189,
77.2451375107018,78.2427088836847,79.2402802566677,80.2378516296506,81.2354230026336,
82.2329943756165,83.2305657485994,84.2281371215823,85.2257084945653,86.2232798675482,
87.2208512405312,88.2184226135141,89.215993986497,90.21356535948,91.2111367324629,
92.2087081054458,93.2062794784288,94.2038508514117,95.2014222243946,96.1989935973776,
97.1965649703605),.UNSPECIFIED.);
#214=B_SPLINE_SURFACE_WITH_KNOTS('',3,3,((#18482,#18483,#18484,#18485,#18486,
#18487,#18488,#18489,#18490,#18491,#18492,#18493,#18494,#18495,#18496,#18497,
#18498,#18499,#18500,#18501,#18502,#18503,#18504,#18505,#18506,#18507,#18508,
#18509,#18510,#18511,#18512,#18513,#18514,#18515,#18516,#18517,#18518,#18519,
#18520,#18521,#18522,#18523,#18524,#18525,#18526,#18527,#18528,#18529,#18530,
#18531,#18532,#18533,#18534,#18535,#18536,#18537,#18538,#18539,#18540,#18541,
#18542,#18543,#18544,#18545,#18546,#18547,#18548,#18549,#18550,#18551,#18552,
#18553,#18554,#18555,#18556,#18557,#18558,#18559,#18560,#18561,#18562,#18563,
#18564,#18565,#18566,#18567),(#18568,#18569,#18570,#18571,#18572,#18573,
#18574,#18575,#18576,#18577,#18578,#18579,#18580,#18581,#18582,#18583,#18584,
#18585,#18586,#18587,#18588,#18589,#18590,#18591,#18592,#18593,#18594,#18595,
#18596,#18597,#18598,#18599,#18600,#18601,#18602,#18603,#18604,#18605,#18606,
#18607,#18608,#18609,#18610,#18611,#18612,#18613,#18614,#18615,#18616,#18617,
#18618,#18619,#18620,#18621,#18622,#18623,#18624,#18625,#18626,#18627,#18628,
#18629,#18630,#18631,#18632,#18633,#18634,#18635,#18636,#18637,#18638,#18639,
#18640,#18641,#18642,#18643,#18644,#18645,#18646,#18647,#18648,#18649,#18650,
#18651,#18652,#18653),(#18654,#18655,#18656,#18657,#18658,#18659,#18660,
#18661,#18662,#18663,#18664,#18665,#18666,#18667,#18668,#18669,#18670,#18671,
#18672,#18673,#18674,#18675,#18676,#18677,#18678,#18679,#18680,#18681,#18682,
#18683,#18684,#18685,#18686,#18687,#18688,#18689,#18690,#18691,#18692,#18693,
#18694,#18695,#18696,#18697,#18698,#18699,#18700,#18701,#18702,#18703,#18704,
#18705,#18706,#18707,#18708,#18709,#18710,#18711,#18712,#18713,#18714,#18715,
#18716,#18717,#18718,#18719,#18720,#18721,#18722,#18723,#18724,#18725,#18726,
#18727,#18728,#18729,#18730,#18731,#18732,#18733,#18734,#18735,#18736,#18737,
#18738,#18739),(#18740,#18741,#18742,#18743,#18744,#18745,#18746,#18747,
#18748,#18749,#18750,#18751,#18752,#18753,#18754,#18755,#18756,#18757,#18758,
#18759,#18760,#18761,#18762,#18763,#18764,#18765,#18766,#18767,#18768,#18769,
#18770,#18771,#18772,#18773,#18774,#18775,#18776,#18777,#18778,#18779,#18780,
#18781,#18782,#18783,#18784,#18785,#18786,#18787,#18788,#18789,#18790,#18791,
#18792,#18793,#18794,#18795,#18796,#18797,#18798,#18799,#18800,#18801,#18802,
#18803,#18804,#18805,#18806,#18807,#18808,#18809,#18810,#18811,#18812,#18813,
#18814,#18815,#18816,#18817,#18818,#18819,#18820,#18821,#18822,#18823,#18824,
#18825)),.UNSPECIFIED.,.F.,.F.,.F.,(4,4),(4,1,1,1,1,1,1,1,1,1,1,1,1,1,1,
1,1,1,1,1,1,1,1,1,1,1,1,1,1,1,1,1,1,1,1,1,1,1,1,1,1,1,1,1,1,1,1,1,1,1,1,
1,1,1,1,1,1,1,1,1,1,1,1,1,1,1,1,1,1,1,1,1,1,1,1,1,1,1,1,1,1,1,1,4),(0.,
0.0448889834294937),(11.8615800042567,12.8591513772396,13.8567227502225,
14.8542941232055,15.8518654961884,16.8494368691713,17.8470082421543,18.8445796151372,
19.8421509881201,20.8397223611031,21.837293734086,22.8348651070689,23.8324364800519,
24.8300078530348,25.8275792260178,26.8251505990007,27.8227219719836,28.8202933449666,
29.8178647179495,30.8154360909324,31.8130074639154,32.8105788368983,33.8081502098812,
34.8057215828642,35.8032929558471,36.80086432883,37.798435701813,38.7960070747959,
39.7935784477788,40.7911498207618,41.7887211937447,42.7862925667276,43.7838639397106,
44.7814353126935,45.7790066856764,46.7765780586594,47.7741494316423,48.7717208046252,
49.7692921776082,50.7668635505911,51.764434923574,52.762006296557,53.7595776695399,
54.7571490425228,55.7547204155058,56.7522917884887,57.7498631614716,58.7474345344546,
59.7450059074375,60.7425772804204,61.7401486534034,62.7377200263863,63.7352913993692,
64.7328627723522,65.7304341453351,66.728005518318,67.725576891301,68.7231482642839,
69.7207196372668,70.7182910102498,71.7158623832327,72.7134337562156,73.7110051291986,
74.7085765021815,75.7061478751644,76.7037192481474,77.7012906211303,78.6988619941132,
79.6964333670962,80.6940047400791,81.6915761130621,82.689147486045,83.6867188590279,
84.6842902320109,85.6818616049938,86.6794329779767,87.6770043509596,88.6745757239426,
89.6721470969255,90.6697184699085,91.6672898428914,92.6648612158743,93.6624325888573,
94.6600039618402),.UNSPECIFIED.);
#215=B_SPLINE_SURFACE_WITH_KNOTS('',3,3,((#18903,#18904,#18905,#18906,#18907,
#18908,#18909,#18910,#18911,#18912,#18913,#18914,#18915,#18916,#18917,#18918,
#18919,#18920,#18921,#18922,#18923,#18924,#18925,#18926,#18927,#18928,#18929,
#18930,#18931,#18932,#18933,#18934,#18935,#18936,#18937,#18938,#18939,#18940,
#18941,#18942,#18943,#18944,#18945,#18946,#18947,#18948,#18949,#18950,#18951,
#18952,#18953,#18954,#18955,#18956,#18957,#18958,#18959,#18960,#18961,#18962,
#18963,#18964,#18965,#18966,#18967,#18968,#18969,#18970,#18971,#18972,#18973,
#18974,#18975,#18976,#18977,#18978,#18979,#18980,#18981,#18982,#18983,#18984,
#18985,#18986,#18987,#18988),(#18989,#18990,#18991,#18992,#18993,#18994,
#18995,#18996,#18997,#18998,#18999,#19000,#19001,#19002,#19003,#19004,#19005,
#19006,#19007,#19008,#19009,#19010,#19011,#19012,#19013,#19014,#19015,#19016,
#19017,#19018,#19019,#19020,#19021,#19022,#19023,#19024,#19025,#19026,#19027,
#19028,#19029,#19030,#19031,#19032,#19033,#19034,#19035,#19036,#19037,#19038,
#19039,#19040,#19041,#19042,#19043,#19044,#19045,#19046,#19047,#19048,#19049,
#19050,#19051,#19052,#19053,#19054,#19055,#19056,#19057,#19058,#19059,#19060,
#19061,#19062,#19063,#19064,#19065,#19066,#19067,#19068,#19069,#19070,#19071,
#19072,#19073,#19074),(#19075,#19076,#19077,#19078,#19079,#19080,#19081,
#19082,#19083,#19084,#19085,#19086,#19087,#19088,#19089,#19090,#19091,#19092,
#19093,#19094,#19095,#19096,#19097,#19098,#19099,#19100,#19101,#19102,#19103,
#19104,#19105,#19106,#19107,#19108,#19109,#19110,#19111,#19112,#19113,#19114,
#19115,#19116,#19117,#19118,#19119,#19120,#19121,#19122,#19123,#19124,#19125,
#19126,#19127,#19128,#19129,#19130,#19131,#19132,#19133,#19134,#19135,#19136,
#19137,#19138,#19139,#19140,#19141,#19142,#19143,#19144,#19145,#19146,#19147,
#19148,#19149,#19150,#19151,#19152,#19153,#19154,#19155,#19156,#19157,#19158,
#19159,#19160),(#19161,#19162,#19163,#19164,#19165,#19166,#19167,#19168,
#19169,#19170,#19171,#19172,#19173,#19174,#19175,#19176,#19177,#19178,#19179,
#19180,#19181,#19182,#19183,#19184,#19185,#19186,#19187,#19188,#19189,#19190,
#19191,#19192,#19193,#19194,#19195,#19196,#19197,#19198,#19199,#19200,#19201,
#19202,#19203,#19204,#19205,#19206,#19207,#19208,#19209,#19210,#19211,#19212,
#19213,#19214,#19215,#19216,#19217,#19218,#19219,#19220,#19221,#19222,#19223,
#19224,#19225,#19226,#19227,#19228,#19229,#19230,#19231,#19232,#19233,#19234,
#19235,#19236,#19237,#19238,#19239,#19240,#19241,#19242,#19243,#19244,#19245,
#19246)),.UNSPECIFIED.,.F.,.F.,.F.,(4,4),(4,1,1,1,1,1,1,1,1,1,1,1,1,1,1,
1,1,1,1,1,1,1,1,1,1,1,1,1,1,1,1,1,1,1,1,1,1,1,1,1,1,1,1,1,1,1,1,1,1,1,1,
1,1,1,1,1,1,1,1,1,1,1,1,1,1,1,1,1,1,1,1,1,1,1,1,1,1,1,1,1,1,1,1,4),(0.,
0.0448889834294937),(14.3981410127769,15.3957123857599,16.3932837587428,
17.3908551317257,18.3884265047087,19.3859978776916,20.3835692506745,21.3811406236575,
22.3787119966404,23.3762833696233,24.3738547426063,25.3714261155892,26.3689974885721,
27.3665688615551,28.364140234538,29.3617116075209,30.3592829805039,31.3568543534868,
32.3544257264697,33.3519970994527,34.3495684724356,35.3471398454185,36.3447112184015,
37.3422825913844,38.3398539643673,39.3374253373503,40.3349967103332,41.3325680833161,
42.3301394562991,43.327710829282,44.3252822022649,45.3228535752479,46.3204249482308,
47.3179963212137,48.3155676941967,49.3131390671796,50.3107104401625,51.3082818131455,
52.3058531861284,53.3034245591113,54.3009959320943,55.2985673050772,56.2961386780601,
57.2937100510431,58.291281424026,59.2888527970089,60.2864241699919,61.2839955429748,
62.2815669159577,63.2791382889407,64.2767096619236,65.2742810349065,66.2718524078895,
67.2694237808724,68.2669951538553,69.2645665268383,70.2621378998212,71.2597092728041,
72.2572806457871,73.25485201877,74.2524233917529,75.2499947647359,76.2475661377188,
77.2451375107017,78.2427088836847,79.2402802566676,80.2378516296505,81.2354230026335,
82.2329943756164,83.2305657485993,84.2281371215823,85.2257084945652,86.2232798675481,
87.2208512405311,88.218422613514,89.2159939864969,90.2135653594799,91.2111367324628,
92.2087081054457,93.2062794784287,94.2038508514116,95.2014222243945,96.1989935973775,
97.1965649703604),.UNSPECIFIED.);
#216=B_SPLINE_SURFACE_WITH_KNOTS('',3,3,((#19455,#19456,#19457,#19458,#19459,
#19460,#19461,#19462,#19463,#19464,#19465,#19466,#19467,#19468,#19469,#19470,
#19471,#19472,#19473,#19474,#19475,#19476,#19477,#19478,#19479,#19480,#19481,
#19482,#19483,#19484,#19485,#19486,#19487,#19488,#19489,#19490,#19491,#19492,
#19493,#19494,#19495,#19496,#19497,#19498,#19499,#19500,#19501,#19502,#19503,
#19504,#19505,#19506,#19507,#19508,#19509,#19510,#19511,#19512,#19513,#19514,
#19515,#19516,#19517,#19518,#19519,#19520,#19521,#19522,#19523,#19524,#19525,
#19526,#19527,#19528,#19529,#19530,#19531,#19532,#19533,#19534,#19535,#19536,
#19537,#19538,#19539,#19540),(#19541,#19542,#19543,#19544,#19545,#19546,
#19547,#19548,#19549,#19550,#19551,#19552,#19553,#19554,#19555,#19556,#19557,
#19558,#19559,#19560,#19561,#19562,#19563,#19564,#19565,#19566,#19567,#19568,
#19569,#19570,#19571,#19572,#19573,#19574,#19575,#19576,#19577,#19578,#19579,
#19580,#19581,#19582,#19583,#19584,#19585,#19586,#19587,#19588,#19589,#19590,
#19591,#19592,#19593,#19594,#19595,#19596,#19597,#19598,#19599,#19600,#19601,
#19602,#19603,#19604,#19605,#19606,#19607,#19608,#19609,#19610,#19611,#19612,
#19613,#19614,#19615,#19616,#19617,#19618,#19619,#19620,#19621,#19622,#19623,
#19624,#19625,#19626),(#19627,#19628,#19629,#19630,#19631,#19632,#19633,
#19634,#19635,#19636,#19637,#19638,#19639,#19640,#19641,#19642,#19643,#19644,
#19645,#19646,#19647,#19648,#19649,#19650,#19651,#19652,#19653,#19654,#19655,
#19656,#19657,#19658,#19659,#19660,#19661,#19662,#19663,#19664,#19665,#19666,
#19667,#19668,#19669,#19670,#19671,#19672,#19673,#19674,#19675,#19676,#19677,
#19678,#19679,#19680,#19681,#19682,#19683,#19684,#19685,#19686,#19687,#19688,
#19689,#19690,#19691,#19692,#19693,#19694,#19695,#19696,#19697,#19698,#19699,
#19700,#19701,#19702,#19703,#19704,#19705,#19706,#19707,#19708,#19709,#19710,
#19711,#19712),(#19713,#19714,#19715,#19716,#19717,#19718,#19719,#19720,
#19721,#19722,#19723,#19724,#19725,#19726,#19727,#19728,#19729,#19730,#19731,
#19732,#19733,#19734,#19735,#19736,#19737,#19738,#19739,#19740,#19741,#19742,
#19743,#19744,#19745,#19746,#19747,#19748,#19749,#19750,#19751,#19752,#19753,
#19754,#19755,#19756,#19757,#19758,#19759,#19760,#19761,#19762,#19763,#19764,
#19765,#19766,#19767,#19768,#19769,#19770,#19771,#19772,#19773,#19774,#19775,
#19776,#19777,#19778,#19779,#19780,#19781,#19782,#19783,#19784,#19785,#19786,
#19787,#19788,#19789,#19790,#19791,#19792,#19793,#19794,#19795,#19796,#19797,
#19798)),.UNSPECIFIED.,.F.,.F.,.F.,(4,4),(4,1,1,1,1,1,1,1,1,1,1,1,1,1,1,
1,1,1,1,1,1,1,1,1,1,1,1,1,1,1,1,1,1,1,1,1,1,1,1,1,1,1,1,1,1,1,1,1,1,1,1,
1,1,1,1,1,1,1,1,1,1,1,1,1,1,1,1,1,1,1,1,1,1,1,1,1,1,1,1,1,1,1,1,4),(0.,
0.0448889834294937),(11.8615800042567,12.8591513772396,13.8567227502225,
14.8542941232055,15.8518654961884,16.8494368691713,17.8470082421543,18.8445796151372,
19.8421509881202,20.8397223611031,21.837293734086,22.834865107069,23.8324364800519,
24.8300078530348,25.8275792260178,26.8251505990007,27.8227219719836,28.8202933449666,
29.8178647179495,30.8154360909324,31.8130074639154,32.8105788368983,33.8081502098812,
34.8057215828642,35.8032929558471,36.80086432883,37.798435701813,38.7960070747959,
39.7935784477788,40.7911498207618,41.7887211937447,42.7862925667276,43.7838639397106,
44.7814353126935,45.7790066856764,46.7765780586594,47.7741494316423,48.7717208046252,
49.7692921776082,50.7668635505911,51.764434923574,52.762006296557,53.7595776695399,
54.7571490425228,55.7547204155058,56.7522917884887,57.7498631614716,58.7474345344546,
59.7450059074375,60.7425772804204,61.7401486534034,62.7377200263863,63.7352913993692,
64.7328627723522,65.7304341453351,66.728005518318,67.725576891301,68.7231482642839,
69.7207196372669,70.7182910102498,71.7158623832327,72.7134337562156,73.7110051291986,
74.7085765021815,75.7061478751644,76.7037192481474,77.7012906211303,78.6988619941132,
79.6964333670962,80.6940047400791,81.6915761130621,82.689147486045,83.6867188590279,
84.6842902320109,85.6818616049938,86.6794329779767,87.6770043509596,88.6745757239426,
89.6721470969255,90.6697184699085,91.6672898428914,92.6648612158743,93.6624325888573,
94.6600039618402),.UNSPECIFIED.);
#217=B_SPLINE_SURFACE_WITH_KNOTS('',3,3,((#19876,#19877,#19878,#19879,#19880,
#19881,#19882,#19883,#19884,#19885,#19886,#19887,#19888,#19889,#19890,#19891,
#19892,#19893,#19894,#19895,#19896,#19897,#19898,#19899,#19900,#19901,#19902,
#19903,#19904,#19905,#19906,#19907,#19908,#19909,#19910,#19911,#19912,#19913,
#19914,#19915,#19916,#19917,#19918,#19919,#19920,#19921,#19922,#19923,#19924,
#19925,#19926,#19927,#19928,#19929,#19930,#19931,#19932,#19933,#19934,#19935,
#19936,#19937,#19938,#19939,#19940,#19941,#19942,#19943,#19944,#19945,#19946,
#19947,#19948,#19949,#19950,#19951,#19952,#19953,#19954,#19955,#19956,#19957,
#19958,#19959,#19960,#19961),(#19962,#19963,#19964,#19965,#19966,#19967,
#19968,#19969,#19970,#19971,#19972,#19973,#19974,#19975,#19976,#19977,#19978,
#19979,#19980,#19981,#19982,#19983,#19984,#19985,#19986,#19987,#19988,#19989,
#19990,#19991,#19992,#19993,#19994,#19995,#19996,#19997,#19998,#19999,#20000,
#20001,#20002,#20003,#20004,#20005,#20006,#20007,#20008,#20009,#20010,#20011,
#20012,#20013,#20014,#20015,#20016,#20017,#20018,#20019,#20020,#20021,#20022,
#20023,#20024,#20025,#20026,#20027,#20028,#20029,#20030,#20031,#20032,#20033,
#20034,#20035,#20036,#20037,#20038,#20039,#20040,#20041,#20042,#20043,#20044,
#20045,#20046,#20047),(#20048,#20049,#20050,#20051,#20052,#20053,#20054,
#20055,#20056,#20057,#20058,#20059,#20060,#20061,#20062,#20063,#20064,#20065,
#20066,#20067,#20068,#20069,#20070,#20071,#20072,#20073,#20074,#20075,#20076,
#20077,#20078,#20079,#20080,#20081,#20082,#20083,#20084,#20085,#20086,#20087,
#20088,#20089,#20090,#20091,#20092,#20093,#20094,#20095,#20096,#20097,#20098,
#20099,#20100,#20101,#20102,#20103,#20104,#20105,#20106,#20107,#20108,#20109,
#20110,#20111,#20112,#20113,#20114,#20115,#20116,#20117,#20118,#20119,#20120,
#20121,#20122,#20123,#20124,#20125,#20126,#20127,#20128,#20129,#20130,#20131,
#20132,#20133),(#20134,#20135,#20136,#20137,#20138,#20139,#20140,#20141,
#20142,#20143,#20144,#20145,#20146,#20147,#20148,#20149,#20150,#20151,#20152,
#20153,#20154,#20155,#20156,#20157,#20158,#20159,#20160,#20161,#20162,#20163,
#20164,#20165,#20166,#20167,#20168,#20169,#20170,#20171,#20172,#20173,#20174,
#20175,#20176,#20177,#20178,#20179,#20180,#20181,#20182,#20183,#20184,#20185,
#20186,#20187,#20188,#20189,#20190,#20191,#20192,#20193,#20194,#20195,#20196,
#20197,#20198,#20199,#20200,#20201,#20202,#20203,#20204,#20205,#20206,#20207,
#20208,#20209,#20210,#20211,#20212,#20213,#20214,#20215,#20216,#20217,#20218,
#20219)),.UNSPECIFIED.,.F.,.F.,.F.,(4,4),(4,1,1,1,1,1,1,1,1,1,1,1,1,1,1,
1,1,1,1,1,1,1,1,1,1,1,1,1,1,1,1,1,1,1,1,1,1,1,1,1,1,1,1,1,1,1,1,1,1,1,1,
1,1,1,1,1,1,1,1,1,1,1,1,1,1,1,1,1,1,1,1,1,1,1,1,1,1,1,1,1,1,1,1,4),(0.,
0.0448889834294937),(14.3981410127769,15.3957123857599,16.3932837587428,
17.3908551317257,18.3884265047087,19.3859978776916,20.3835692506745,21.3811406236575,
22.3787119966404,23.3762833696233,24.3738547426063,25.3714261155892,26.3689974885721,
27.3665688615551,28.364140234538,29.3617116075209,30.3592829805039,31.3568543534868,
32.3544257264697,33.3519970994527,34.3495684724356,35.3471398454185,36.3447112184015,
37.3422825913844,38.3398539643673,39.3374253373503,40.3349967103332,41.3325680833161,
42.3301394562991,43.327710829282,44.3252822022649,45.3228535752479,46.3204249482308,
47.3179963212137,48.3155676941967,49.3131390671796,50.3107104401625,51.3082818131455,
52.3058531861284,53.3034245591113,54.3009959320943,55.2985673050772,56.2961386780601,
57.2937100510431,58.291281424026,59.2888527970089,60.2864241699919,61.2839955429748,
62.2815669159577,63.2791382889407,64.2767096619236,65.2742810349065,66.2718524078895,
67.2694237808724,68.2669951538553,69.2645665268383,70.2621378998212,71.2597092728041,
72.2572806457871,73.25485201877,74.2524233917529,75.2499947647359,76.2475661377188,
77.2451375107017,78.2427088836847,79.2402802566676,80.2378516296505,81.2354230026335,
82.2329943756164,83.2305657485993,84.2281371215823,85.2257084945652,86.2232798675481,
87.2208512405311,88.218422613514,89.2159939864969,90.2135653594799,91.2111367324628,
92.2087081054457,93.2062794784287,94.2038508514116,95.2014222243945,96.1989935973775,
97.1965649703604),.UNSPECIFIED.);
#218=B_SPLINE_SURFACE_WITH_KNOTS('',3,3,((#21599,#21600,#21601,#21602,#21603,
#21604,#21605,#21606,#21607,#21608,#21609,#21610,#21611,#21612,#21613,#21614,
#21615,#21616,#21617,#21618,#21619,#21620,#21621,#21622,#21623,#21624,#21625,
#21626,#21627,#21628,#21629,#21630,#21631,#21632,#21633,#21634,#21635,#21636,
#21637,#21638,#21639,#21640,#21641,#21642,#21643,#21644,#21645,#21646,#21647,
#21648,#21649,#21650,#21651,#21652,#21653,#21654),(#21655,#21656,#21657,
#21658,#21659,#21660,#21661,#21662,#21663,#21664,#21665,#21666,#21667,#21668,
#21669,#21670,#21671,#21672,#21673,#21674,#21675,#21676,#21677,#21678,#21679,
#21680,#21681,#21682,#21683,#21684,#21685,#21686,#21687,#21688,#21689,#21690,
#21691,#21692,#21693,#21694,#21695,#21696,#21697,#21698,#21699,#21700,#21701,
#21702,#21703,#21704,#21705,#21706,#21707,#21708,#21709,#21710),(#21711,
#21712,#21713,#21714,#21715,#21716,#21717,#21718,#21719,#21720,#21721,#21722,
#21723,#21724,#21725,#21726,#21727,#21728,#21729,#21730,#21731,#21732,#21733,
#21734,#21735,#21736,#21737,#21738,#21739,#21740,#21741,#21742,#21743,#21744,
#21745,#21746,#21747,#21748,#21749,#21750,#21751,#21752,#21753,#21754,#21755,
#21756,#21757,#21758,#21759,#21760,#21761,#21762,#21763,#21764,#21765,#21766),
(#21767,#21768,#21769,#21770,#21771,#21772,#21773,#21774,#21775,#21776,
#21777,#21778,#21779,#21780,#21781,#21782,#21783,#21784,#21785,#21786,#21787,
#21788,#21789,#21790,#21791,#21792,#21793,#21794,#21795,#21796,#21797,#21798,
#21799,#21800,#21801,#21802,#21803,#21804,#21805,#21806,#21807,#21808,#21809,
#21810,#21811,#21812,#21813,#21814,#21815,#21816,#21817,#21818,#21819,#21820,
#21821,#21822)),.UNSPECIFIED.,.F.,.F.,.F.,(4,4),(4,1,1,1,1,1,1,1,1,1,1,
1,1,1,1,1,1,1,1,1,1,1,1,1,1,1,1,1,1,1,1,1,1,1,1,1,1,1,1,1,1,1,1,1,1,1,1,
1,1,1,1,1,1,4),(0.,0.0321584099938621),(11.8553612635793,12.8418906022433,
13.8284199409074,14.8149492795714,15.8014786182354,16.7880079568995,17.7745372955635,
18.7610666342275,19.7475959728915,20.7341253115556,21.7206546502196,22.7071839888836,
23.6937133275477,24.6802426662117,25.6667720048757,26.6533013435398,27.6398306822038,
28.6263600208678,29.6128893595319,30.5994186981959,31.5859480368599,32.5724773755239,
33.559006714188,34.545536052852,35.532065391516,36.5185947301801,37.5051240688441,
38.4916534075081,39.4781827461722,40.4647120848362,41.4512414235002,42.4377707621643,
43.4243001008283,44.4108294394923,45.3973587781563,46.3838881168204,47.3704174554844,
48.3569467941484,49.3434761328125,50.3300054714765,51.3165348101405,52.3030641488046,
53.2895934874686,54.2761228261326,55.2626521647967,56.2491815034607,57.2357108421247,
58.2222401807888,59.2087695194528,60.1952988581168,61.1818281967808,62.1683575354449,
63.1548868741089,64.1414162127729),.UNSPECIFIED.);
#219=B_SPLINE_SURFACE_WITH_KNOTS('',3,3,((#21949,#21950,#21951,#21952,#21953,
#21954,#21955,#21956,#21957,#21958,#21959,#21960,#21961,#21962,#21963,#21964,
#21965,#21966,#21967,#21968,#21969,#21970,#21971,#21972,#21973,#21974,#21975,
#21976,#21977,#21978,#21979,#21980,#21981,#21982,#21983,#21984,#21985,#21986,
#21987,#21988,#21989,#21990,#21991,#21992,#21993,#21994,#21995,#21996,#21997,
#21998,#21999,#22000,#22001,#22002,#22003,#22004),(#22005,#22006,#22007,
#22008,#22009,#22010,#22011,#22012,#22013,#22014,#22015,#22016,#22017,#22018,
#22019,#22020,#22021,#22022,#22023,#22024,#22025,#22026,#22027,#22028,#22029,
#22030,#22031,#22032,#22033,#22034,#22035,#22036,#22037,#22038,#22039,#22040,
#22041,#22042,#22043,#22044,#22045,#22046,#22047,#22048,#22049,#22050,#22051,
#22052,#22053,#22054,#22055,#22056,#22057,#22058,#22059,#22060),(#22061,
#22062,#22063,#22064,#22065,#22066,#22067,#22068,#22069,#22070,#22071,#22072,
#22073,#22074,#22075,#22076,#22077,#22078,#22079,#22080,#22081,#22082,#22083,
#22084,#22085,#22086,#22087,#22088,#22089,#22090,#22091,#22092,#22093,#22094,
#22095,#22096,#22097,#22098,#22099,#22100,#22101,#22102,#22103,#22104,#22105,
#22106,#22107,#22108,#22109,#22110,#22111,#22112,#22113,#22114,#22115,#22116),
(#22117,#22118,#22119,#22120,#22121,#22122,#22123,#22124,#22125,#22126,
#22127,#22128,#22129,#22130,#22131,#22132,#22133,#22134,#22135,#22136,#22137,
#22138,#22139,#22140,#22141,#22142,#22143,#22144,#22145,#22146,#22147,#22148,
#22149,#22150,#22151,#22152,#22153,#22154,#22155,#22156,#22157,#22158,#22159,
#22160,#22161,#22162,#22163,#22164,#22165,#22166,#22167,#22168,#22169,#22170,
#22171,#22172)),.UNSPECIFIED.,.F.,.F.,.F.,(4,4),(4,1,1,1,1,1,1,1,1,1,1,
1,1,1,1,1,1,1,1,1,1,1,1,1,1,1,1,1,1,1,1,1,1,1,1,1,1,1,1,1,1,1,1,1,1,1,1,
1,1,1,1,1,1,4),(0.,0.0321584099938621),(14.3984001269718,15.3849294656359,
16.3714588042999,17.3579881429639,18.344517481628,19.331046820292,20.317576158956,
21.30410549762,22.2906348362841,23.2771641749481,24.2636935136121,25.2502228522762,
26.2367521909402,27.2232815296042,28.2098108682683,29.1963402069323,30.1828695455963,
31.1693988842604,32.1559282229244,33.1424575615884,34.1289869002524,35.1155162389165,
36.1020455775805,37.0885749162445,38.0751042549086,39.0616335935726,40.0481629322366,
41.0346922709007,42.0212216095647,43.0077509482287,43.9942802868928,44.9808096255568,
45.9673389642208,46.9538683028848,47.9403976415489,48.9269269802129,49.9134563188769,
50.899985657541,51.886514996205,52.873044334869,53.8595736735331,54.8461030121971,
55.8326323508611,56.8191616895251,57.8056910281892,58.7922203668532,59.7787497055172,
60.7652790441813,61.7518083828453,62.7383377215093,63.7248670601734,64.7113963988374,
65.6979257375014,66.6844550761655),.UNSPECIFIED.);
#220=B_SPLINE_SURFACE_WITH_KNOTS('',3,3,((#22435,#22436,#22437,#22438,#22439,
#22440,#22441,#22442,#22443,#22444,#22445,#22446,#22447,#22448,#22449,#22450,
#22451,#22452,#22453,#22454,#22455,#22456,#22457,#22458,#22459,#22460,#22461,
#22462,#22463,#22464,#22465,#22466,#22467,#22468,#22469,#22470,#22471,#22472,
#22473,#22474,#22475,#22476,#22477,#22478,#22479,#22480,#22481,#22482,#22483,
#22484,#22485,#22486,#22487,#22488,#22489,#22490),(#22491,#22492,#22493,
#22494,#22495,#22496,#22497,#22498,#22499,#22500,#22501,#22502,#22503,#22504,
#22505,#22506,#22507,#22508,#22509,#22510,#22511,#22512,#22513,#22514,#22515,
#22516,#22517,#22518,#22519,#22520,#22521,#22522,#22523,#22524,#22525,#22526,
#22527,#22528,#22529,#22530,#22531,#22532,#22533,#22534,#22535,#22536,#22537,
#22538,#22539,#22540,#22541,#22542,#22543,#22544,#22545,#22546),(#22547,
#22548,#22549,#22550,#22551,#22552,#22553,#22554,#22555,#22556,#22557,#22558,
#22559,#22560,#22561,#22562,#22563,#22564,#22565,#22566,#22567,#22568,#22569,
#22570,#22571,#22572,#22573,#22574,#22575,#22576,#22577,#22578,#22579,#22580,
#22581,#22582,#22583,#22584,#22585,#22586,#22587,#22588,#22589,#22590,#22591,
#22592,#22593,#22594,#22595,#22596,#22597,#22598,#22599,#22600,#22601,#22602),
(#22603,#22604,#22605,#22606,#22607,#22608,#22609,#22610,#22611,#22612,
#22613,#22614,#22615,#22616,#22617,#22618,#22619,#22620,#22621,#22622,#22623,
#22624,#22625,#22626,#22627,#22628,#22629,#22630,#22631,#22632,#22633,#22634,
#22635,#22636,#22637,#22638,#22639,#22640,#22641,#22642,#22643,#22644,#22645,
#22646,#22647,#22648,#22649,#22650,#22651,#22652,#22653,#22654,#22655,#22656,
#22657,#22658)),.UNSPECIFIED.,.F.,.F.,.F.,(4,4),(4,1,1,1,1,1,1,1,1,1,1,
1,1,1,1,1,1,1,1,1,1,1,1,1,1,1,1,1,1,1,1,1,1,1,1,1,1,1,1,1,1,1,1,1,1,1,1,
1,1,1,1,1,1,4),(0.,0.0321584099938621),(11.8553612635793,12.8418906022433,
13.8284199409074,14.8149492795714,15.8014786182354,16.7880079568995,17.7745372955635,
18.7610666342275,19.7475959728915,20.7341253115556,21.7206546502196,22.7071839888836,
23.6937133275477,24.6802426662117,25.6667720048757,26.6533013435398,27.6398306822038,
28.6263600208678,29.6128893595319,30.5994186981959,31.5859480368599,32.5724773755239,
33.559006714188,34.545536052852,35.532065391516,36.5185947301801,37.5051240688441,
38.4916534075081,39.4781827461722,40.4647120848362,41.4512414235002,42.4377707621643,
43.4243001008283,44.4108294394923,45.3973587781563,46.3838881168204,47.3704174554844,
48.3569467941484,49.3434761328125,50.3300054714765,51.3165348101405,52.3030641488046,
53.2895934874686,54.2761228261326,55.2626521647967,56.2491815034607,57.2357108421247,
58.2222401807888,59.2087695194528,60.1952988581168,61.1818281967808,62.1683575354449,
63.1548868741089,64.1414162127729),.UNSPECIFIED.);
#221=B_SPLINE_SURFACE_WITH_KNOTS('',3,3,((#22733,#22734,#22735,#22736,#22737,
#22738,#22739,#22740,#22741,#22742,#22743,#22744,#22745,#22746,#22747,#22748,
#22749,#22750,#22751,#22752,#22753,#22754,#22755,#22756,#22757,#22758,#22759,
#22760,#22761,#22762,#22763,#22764,#22765,#22766,#22767,#22768,#22769,#22770,
#22771,#22772,#22773,#22774,#22775,#22776,#22777,#22778,#22779,#22780,#22781,
#22782,#22783,#22784,#22785,#22786,#22787,#22788),(#22789,#22790,#22791,
#22792,#22793,#22794,#22795,#22796,#22797,#22798,#22799,#22800,#22801,#22802,
#22803,#22804,#22805,#22806,#22807,#22808,#22809,#22810,#22811,#22812,#22813,
#22814,#22815,#22816,#22817,#22818,#22819,#22820,#22821,#22822,#22823,#22824,
#22825,#22826,#22827,#22828,#22829,#22830,#22831,#22832,#22833,#22834,#22835,
#22836,#22837,#22838,#22839,#22840,#22841,#22842,#22843,#22844),(#22845,
#22846,#22847,#22848,#22849,#22850,#22851,#22852,#22853,#22854,#22855,#22856,
#22857,#22858,#22859,#22860,#22861,#22862,#22863,#22864,#22865,#22866,#22867,
#22868,#22869,#22870,#22871,#22872,#22873,#22874,#22875,#22876,#22877,#22878,
#22879,#22880,#22881,#22882,#22883,#22884,#22885,#22886,#22887,#22888,#22889,
#22890,#22891,#22892,#22893,#22894,#22895,#22896,#22897,#22898,#22899,#22900),
(#22901,#22902,#22903,#22904,#22905,#22906,#22907,#22908,#22909,#22910,
#22911,#22912,#22913,#22914,#22915,#22916,#22917,#22918,#22919,#22920,#22921,
#22922,#22923,#22924,#22925,#22926,#22927,#22928,#22929,#22930,#22931,#22932,
#22933,#22934,#22935,#22936,#22937,#22938,#22939,#22940,#22941,#22942,#22943,
#22944,#22945,#22946,#22947,#22948,#22949,#22950,#22951,#22952,#22953,#22954,
#22955,#22956)),.UNSPECIFIED.,.F.,.F.,.F.,(4,4),(4,1,1,1,1,1,1,1,1,1,1,
1,1,1,1,1,1,1,1,1,1,1,1,1,1,1,1,1,1,1,1,1,1,1,1,1,1,1,1,1,1,1,1,1,1,1,1,
1,1,1,1,1,1,4),(0.,0.0321584099938621),(14.3984001269718,15.3849294656359,
16.3714588042999,17.3579881429639,18.344517481628,19.331046820292,20.317576158956,
21.30410549762,22.2906348362841,23.2771641749481,24.2636935136121,25.2502228522762,
26.2367521909402,27.2232815296042,28.2098108682683,29.1963402069323,30.1828695455963,
31.1693988842604,32.1559282229244,33.1424575615884,34.1289869002524,35.1155162389165,
36.1020455775805,37.0885749162445,38.0751042549086,39.0616335935726,40.0481629322366,
41.0346922709007,42.0212216095647,43.0077509482287,43.9942802868928,44.9808096255568,
45.9673389642208,46.9538683028848,47.9403976415489,48.9269269802129,49.9134563188769,
50.899985657541,51.886514996205,52.873044334869,53.8595736735331,54.8461030121971,
55.8326323508611,56.8191616895251,57.8056910281892,58.7922203668532,59.7787497055172,
60.7652790441813,61.7518083828453,62.7383377215093,63.7248670601734,64.7113963988374,
65.6979257375014,66.6844550761655),.UNSPECIFIED.);
#222=B_SPLINE_SURFACE_WITH_KNOTS('',3,3,((#25543,#25544,#25545,#25546,#25547,
#25548,#25549,#25550,#25551,#25552,#25553,#25554,#25555,#25556,#25557,#25558,
#25559,#25560,#25561,#25562,#25563,#25564,#25565,#25566,#25567,#25568,#25569,
#25570,#25571,#25572,#25573,#25574,#25575,#25576,#25577,#25578,#25579,#25580,
#25581,#25582,#25583,#25584,#25585,#25586,#25587,#25588,#25589,#25590,#25591,
#25592,#25593,#25594,#25595,#25596,#25597,#25598,#25599,#25600,#25601,#25602,
#25603,#25604,#25605,#25606,#25607,#25608,#25609,#25610,#25611,#25612,#25613,
#25614,#25615,#25616,#25617,#25618,#25619,#25620,#25621,#25622,#25623,#25624,
#25625,#25626,#25627,#25628,#25629,#25630,#25631,#25632,#25633,#25634,#25635,
#25636,#25637,#25638,#25639,#25640,#25641,#25642,#25643,#25644,#25645,#25646,
#25647,#25648,#25649,#25650,#25651,#25652,#25653,#25654,#25655,#25656,#25657,
#25658,#25659,#25660,#25661),(#25662,#25663,#25664,#25665,#25666,#25667,
#25668,#25669,#25670,#25671,#25672,#25673,#25674,#25675,#25676,#25677,#25678,
#25679,#25680,#25681,#25682,#25683,#25684,#25685,#25686,#25687,#25688,#25689,
#25690,#25691,#25692,#25693,#25694,#25695,#25696,#25697,#25698,#25699,#25700,
#25701,#25702,#25703,#25704,#25705,#25706,#25707,#25708,#25709,#25710,#25711,
#25712,#25713,#25714,#25715,#25716,#25717,#25718,#25719,#25720,#25721,#25722,
#25723,#25724,#25725,#25726,#25727,#25728,#25729,#25730,#25731,#25732,#25733,
#25734,#25735,#25736,#25737,#25738,#25739,#25740,#25741,#25742,#25743,#25744,
#25745,#25746,#25747,#25748,#25749,#25750,#25751,#25752,#25753,#25754,#25755,
#25756,#25757,#25758,#25759,#25760,#25761,#25762,#25763,#25764,#25765,#25766,
#25767,#25768,#25769,#25770,#25771,#25772,#25773,#25774,#25775,#25776,#25777,
#25778,#25779,#25780),(#25781,#25782,#25783,#25784,#25785,#25786,#25787,
#25788,#25789,#25790,#25791,#25792,#25793,#25794,#25795,#25796,#25797,#25798,
#25799,#25800,#25801,#25802,#25803,#25804,#25805,#25806,#25807,#25808,#25809,
#25810,#25811,#25812,#25813,#25814,#25815,#25816,#25817,#25818,#25819,#25820,
#25821,#25822,#25823,#25824,#25825,#25826,#25827,#25828,#25829,#25830,#25831,
#25832,#25833,#25834,#25835,#25836,#25837,#25838,#25839,#25840,#25841,#25842,
#25843,#25844,#25845,#25846,#25847,#25848,#25849,#25850,#25851,#25852,#25853,
#25854,#25855,#25856,#25857,#25858,#25859,#25860,#25861,#25862,#25863,#25864,
#25865,#25866,#25867,#25868,#25869,#25870,#25871,#25872,#25873,#25874,#25875,
#25876,#25877,#25878,#25879,#25880,#25881,#25882,#25883,#25884,#25885,#25886,
#25887,#25888,#25889,#25890,#25891,#25892,#25893,#25894,#25895,#25896,#25897,
#25898,#25899),(#25900,#25901,#25902,#25903,#25904,#25905,#25906,#25907,
#25908,#25909,#25910,#25911,#25912,#25913,#25914,#25915,#25916,#25917,#25918,
#25919,#25920,#25921,#25922,#25923,#25924,#25925,#25926,#25927,#25928,#25929,
#25930,#25931,#25932,#25933,#25934,#25935,#25936,#25937,#25938,#25939,#25940,
#25941,#25942,#25943,#25944,#25945,#25946,#25947,#25948,#25949,#25950,#25951,
#25952,#25953,#25954,#25955,#25956,#25957,#25958,#25959,#25960,#25961,#25962,
#25963,#25964,#25965,#25966,#25967,#25968,#25969,#25970,#25971,#25972,#25973,
#25974,#25975,#25976,#25977,#25978,#25979,#25980,#25981,#25982,#25983,#25984,
#25985,#25986,#25987,#25988,#25989,#25990,#25991,#25992,#25993,#25994,#25995,
#25996,#25997,#25998,#25999,#26000,#26001,#26002,#26003,#26004,#26005,#26006,
#26007,#26008,#26009,#26010,#26011,#26012,#26013,#26014,#26015,#26016,#26017,
#26018)),.UNSPECIFIED.,.F.,.F.,.F.,(4,4),(4,1,1,1,1,1,1,1,1,1,1,1,1,1,1,
1,1,1,1,1,1,1,1,1,1,1,1,1,1,1,1,1,1,1,1,1,1,1,1,1,1,1,1,1,1,1,1,1,1,1,1,
1,1,1,1,1,1,1,1,1,1,1,1,1,1,1,1,1,1,1,1,1,1,1,1,1,1,1,1,1,1,1,1,1,1,1,1,
1,1,1,1,1,1,1,1,1,1,1,1,1,1,1,1,1,1,1,1,1,1,1,1,1,1,1,1,1,4),(0.,0.0321584099938621),
(11.8553612635792,12.8477570223809,13.8401527811825,14.8325485399841,15.8249442987858,
16.8173400575874,17.809735816389,18.8021315751907,19.7945273339923,20.7869230927939,
21.7793188515956,22.7717146103972,23.7641103691988,24.7565061280005,25.7489018868021,
26.7412976456037,27.7336934044054,28.726089163207,29.7184849220086,30.7108806808103,
31.7032764396119,32.6956721984135,33.6880679572152,34.6804637160168,35.6728594748184,
36.6652552336201,37.6576509924217,38.6500467512233,39.642442510025,40.6348382688266,
41.6272340276282,42.6196297864299,43.6120255452315,44.6044213040331,45.5968170628348,
46.5892128216364,47.581608580438,48.5740043392397,49.5664000980413,50.5587958568429,
51.5511916156446,52.5435873744462,53.5359831332478,54.5283788920495,55.5207746508511,
56.5131704096527,57.5055661684544,58.497961927256,59.4903576860576,60.4827534448593,
61.4751492036609,62.4675449624625,63.4599407212642,64.4523364800658,65.4447322388674,
66.4371279976691,67.4295237564707,68.4219195152723,69.4143152740739,70.4067110328756,
71.3991067916772,72.3915025504788,73.3838983092805,74.3762940680821,75.3686898268838,
76.3610855856854,77.353481344487,78.3458771032886,79.3382728620903,80.3306686208919,
81.3230643796935,82.3154601384952,83.3078558972968,84.3002516560985,85.2926474149001,
86.2850431737017,87.2774389325033,88.269834691305,89.2622304501066,90.2546262089082,
91.2470219677099,92.2394177265115,93.2318134853131,94.2242092441148,95.2166050029164,
96.209000761718,97.2013965205197,98.1937922793213,99.1861880381229,100.178583796925,
101.170979555726,102.163375314528,103.155771073329,104.148166832131,105.140562590933,
106.132958349734,107.125354108536,108.117749867338,109.110145626139,110.102541384941,
111.094937143743,112.087332902544,113.079728661346,114.072124420147,115.064520178949,
116.056915937751,117.049311696552,118.041707455354,119.034103214156,120.026498972957,
121.018894731759,122.01129049056,123.003686249362,123.996082008164,124.988477766965,
125.980873525767,126.973269284569),.UNSPECIFIED.);
#223=B_SPLINE_SURFACE_WITH_KNOTS('',3,3,((#26093,#26094,#26095,#26096,#26097,
#26098,#26099,#26100,#26101,#26102,#26103,#26104,#26105,#26106,#26107,#26108,
#26109,#26110,#26111,#26112,#26113,#26114,#26115,#26116,#26117,#26118,#26119,
#26120,#26121,#26122,#26123,#26124,#26125,#26126,#26127,#26128,#26129,#26130,
#26131,#26132,#26133,#26134,#26135,#26136,#26137,#26138,#26139,#26140,#26141,
#26142,#26143,#26144,#26145,#26146,#26147,#26148,#26149,#26150,#26151,#26152,
#26153,#26154,#26155,#26156,#26157,#26158,#26159,#26160,#26161,#26162,#26163,
#26164,#26165,#26166,#26167,#26168,#26169,#26170,#26171,#26172,#26173,#26174,
#26175,#26176,#26177,#26178,#26179,#26180,#26181,#26182,#26183,#26184,#26185,
#26186,#26187,#26188,#26189,#26190,#26191,#26192,#26193,#26194,#26195,#26196,
#26197,#26198,#26199,#26200,#26201,#26202,#26203,#26204,#26205,#26206,#26207,
#26208,#26209,#26210,#26211),(#26212,#26213,#26214,#26215,#26216,#26217,
#26218,#26219,#26220,#26221,#26222,#26223,#26224,#26225,#26226,#26227,#26228,
#26229,#26230,#26231,#26232,#26233,#26234,#26235,#26236,#26237,#26238,#26239,
#26240,#26241,#26242,#26243,#26244,#26245,#26246,#26247,#26248,#26249,#26250,
#26251,#26252,#26253,#26254,#26255,#26256,#26257,#26258,#26259,#26260,#26261,
#26262,#26263,#26264,#26265,#26266,#26267,#26268,#26269,#26270,#26271,#26272,
#26273,#26274,#26275,#26276,#26277,#26278,#26279,#26280,#26281,#26282,#26283,
#26284,#26285,#26286,#26287,#26288,#26289,#26290,#26291,#26292,#26293,#26294,
#26295,#26296,#26297,#26298,#26299,#26300,#26301,#26302,#26303,#26304,#26305,
#26306,#26307,#26308,#26309,#26310,#26311,#26312,#26313,#26314,#26315,#26316,
#26317,#26318,#26319,#26320,#26321,#26322,#26323,#26324,#26325,#26326,#26327,
#26328,#26329,#26330),(#26331,#26332,#26333,#26334,#26335,#26336,#26337,
#26338,#26339,#26340,#26341,#26342,#26343,#26344,#26345,#26346,#26347,#26348,
#26349,#26350,#26351,#26352,#26353,#26354,#26355,#26356,#26357,#26358,#26359,
#26360,#26361,#26362,#26363,#26364,#26365,#26366,#26367,#26368,#26369,#26370,
#26371,#26372,#26373,#26374,#26375,#26376,#26377,#26378,#26379,#26380,#26381,
#26382,#26383,#26384,#26385,#26386,#26387,#26388,#26389,#26390,#26391,#26392,
#26393,#26394,#26395,#26396,#26397,#26398,#26399,#26400,#26401,#26402,#26403,
#26404,#26405,#26406,#26407,#26408,#26409,#26410,#26411,#26412,#26413,#26414,
#26415,#26416,#26417,#26418,#26419,#26420,#26421,#26422,#26423,#26424,#26425,
#26426,#26427,#26428,#26429,#26430,#26431,#26432,#26433,#26434,#26435,#26436,
#26437,#26438,#26439,#26440,#26441,#26442,#26443,#26444,#26445,#26446,#26447,
#26448,#26449),(#26450,#26451,#26452,#26453,#26454,#26455,#26456,#26457,
#26458,#26459,#26460,#26461,#26462,#26463,#26464,#26465,#26466,#26467,#26468,
#26469,#26470,#26471,#26472,#26473,#26474,#26475,#26476,#26477,#26478,#26479,
#26480,#26481,#26482,#26483,#26484,#26485,#26486,#26487,#26488,#26489,#26490,
#26491,#26492,#26493,#26494,#26495,#26496,#26497,#26498,#26499,#26500,#26501,
#26502,#26503,#26504,#26505,#26506,#26507,#26508,#26509,#26510,#26511,#26512,
#26513,#26514,#26515,#26516,#26517,#26518,#26519,#26520,#26521,#26522,#26523,
#26524,#26525,#26526,#26527,#26528,#26529,#26530,#26531,#26532,#26533,#26534,
#26535,#26536,#26537,#26538,#26539,#26540,#26541,#26542,#26543,#26544,#26545,
#26546,#26547,#26548,#26549,#26550,#26551,#26552,#26553,#26554,#26555,#26556,
#26557,#26558,#26559,#26560,#26561,#26562,#26563,#26564,#26565,#26566,#26567,
#26568)),.UNSPECIFIED.,.F.,.F.,.F.,(4,4),(4,1,1,1,1,1,1,1,1,1,1,1,1,1,1,
1,1,1,1,1,1,1,1,1,1,1,1,1,1,1,1,1,1,1,1,1,1,1,1,1,1,1,1,1,1,1,1,1,1,1,1,
1,1,1,1,1,1,1,1,1,1,1,1,1,1,1,1,1,1,1,1,1,1,1,1,1,1,1,1,1,1,1,1,1,1,1,1,
1,1,1,1,1,1,1,1,1,1,1,1,1,1,1,1,1,1,1,1,1,1,1,1,1,1,1,1,1,4),(0.,0.0321584099938621),
(14.3984001269718,15.3907958857734,16.383191644575,17.3755874033767,18.3679831621783,
19.3603789209799,20.3527746797816,21.3451704385832,22.3375661973848,23.3299619561865,
24.3223577149881,25.3147534737897,26.3071492325914,27.299544991393,28.2919407501946,
29.2843365089963,30.2767322677979,31.2691280265995,32.2615237854012,33.2539195442028,
34.2463153030044,35.2387110618061,36.2311068206077,37.2235025794093,38.215898338211,
39.2082940970126,40.2006898558142,41.1930856146159,42.1854813734175,43.1778771322191,
44.1702728910208,45.1626686498224,46.155064408624,47.1474601674257,48.1398559262273,
49.1322516850289,50.1246474438306,51.1170432026322,52.1094389614338,53.1018347202355,
54.0942304790371,55.0866262378387,56.0790219966403,57.071417755442,58.0638135142436,
59.0562092730452,60.0486050318469,61.0410007906485,62.0333965494501,63.0257923082518,
64.0181880670534,65.010583825855,66.0029795846567,66.9953753434583,67.9877711022599,
68.9801668610616,69.9725626198632,70.9649583786648,71.9573541374665,72.9497498962681,
73.9421456550697,74.9345414138714,75.926937172673,76.9193329314746,77.9117286902763,
78.9041244490779,79.8965202078795,80.8889159666812,81.8813117254828,82.8737074842844,
83.8661032430861,84.8584990018877,85.8508947606893,86.8432905194909,87.8356862782926,
88.8280820370942,89.8204777958959,90.8128735546975,91.8052693134991,92.7976650723007,
93.7900608311024,94.782456589904,95.7748523487057,96.7672481075073,97.7596438663089,
98.7520396251105,99.7444353839122,100.736831142714,101.729226901515,102.721622660317,
103.714018419119,104.70641417792,105.698809936722,106.691205695524,107.683601454325,
108.675997213127,109.668392971929,110.66078873073,111.653184489532,112.645580248333,
113.637976007135,114.630371765937,115.622767524738,116.61516328354,117.607559042342,
118.599954801143,119.592350559945,120.584746318746,121.577142077548,122.56953783635,
123.561933595151,124.554329353953,125.546725112755,126.539120871556,127.531516630358,
128.52391238916,129.516308147961),.UNSPECIFIED.);
#224=B_SPLINE_SURFACE_WITH_KNOTS('',3,3,((#26775,#26776,#26777,#26778,#26779,
#26780,#26781,#26782,#26783,#26784,#26785,#26786,#26787,#26788,#26789,#26790,
#26791,#26792,#26793,#26794,#26795,#26796,#26797,#26798,#26799,#26800,#26801,
#26802,#26803,#26804,#26805,#26806,#26807,#26808,#26809,#26810,#26811,#26812,
#26813,#26814,#26815,#26816,#26817,#26818,#26819,#26820,#26821,#26822,#26823,
#26824,#26825,#26826,#26827,#26828,#26829,#26830,#26831,#26832,#26833,#26834,
#26835,#26836,#26837,#26838,#26839,#26840,#26841,#26842,#26843,#26844,#26845,
#26846,#26847,#26848,#26849,#26850,#26851,#26852,#26853,#26854,#26855,#26856,
#26857,#26858,#26859,#26860),(#26861,#26862,#26863,#26864,#26865,#26866,
#26867,#26868,#26869,#26870,#26871,#26872,#26873,#26874,#26875,#26876,#26877,
#26878,#26879,#26880,#26881,#26882,#26883,#26884,#26885,#26886,#26887,#26888,
#26889,#26890,#26891,#26892,#26893,#26894,#26895,#26896,#26897,#26898,#26899,
#26900,#26901,#26902,#26903,#26904,#26905,#26906,#26907,#26908,#26909,#26910,
#26911,#26912,#26913,#26914,#26915,#26916,#26917,#26918,#26919,#26920,#26921,
#26922,#26923,#26924,#26925,#26926,#26927,#26928,#26929,#26930,#26931,#26932,
#26933,#26934,#26935,#26936,#26937,#26938,#26939,#26940,#26941,#26942,#26943,
#26944,#26945,#26946),(#26947,#26948,#26949,#26950,#26951,#26952,#26953,
#26954,#26955,#26956,#26957,#26958,#26959,#26960,#26961,#26962,#26963,#26964,
#26965,#26966,#26967,#26968,#26969,#26970,#26971,#26972,#26973,#26974,#26975,
#26976,#26977,#26978,#26979,#26980,#26981,#26982,#26983,#26984,#26985,#26986,
#26987,#26988,#26989,#26990,#26991,#26992,#26993,#26994,#26995,#26996,#26997,
#26998,#26999,#27000,#27001,#27002,#27003,#27004,#27005,#27006,#27007,#27008,
#27009,#27010,#27011,#27012,#27013,#27014,#27015,#27016,#27017,#27018,#27019,
#27020,#27021,#27022,#27023,#27024,#27025,#27026,#27027,#27028,#27029,#27030,
#27031,#27032),(#27033,#27034,#27035,#27036,#27037,#27038,#27039,#27040,
#27041,#27042,#27043,#27044,#27045,#27046,#27047,#27048,#27049,#27050,#27051,
#27052,#27053,#27054,#27055,#27056,#27057,#27058,#27059,#27060,#27061,#27062,
#27063,#27064,#27065,#27066,#27067,#27068,#27069,#27070,#27071,#27072,#27073,
#27074,#27075,#27076,#27077,#27078,#27079,#27080,#27081,#27082,#27083,#27084,
#27085,#27086,#27087,#27088,#27089,#27090,#27091,#27092,#27093,#27094,#27095,
#27096,#27097,#27098,#27099,#27100,#27101,#27102,#27103,#27104,#27105,#27106,
#27107,#27108,#27109,#27110,#27111,#27112,#27113,#27114,#27115,#27116,#27117,
#27118)),.UNSPECIFIED.,.F.,.F.,.F.,(4,4),(4,1,1,1,1,1,1,1,1,1,1,1,1,1,1,
1,1,1,1,1,1,1,1,1,1,1,1,1,1,1,1,1,1,1,1,1,1,1,1,1,1,1,1,1,1,1,1,1,1,1,1,
1,1,1,1,1,1,1,1,1,1,1,1,1,1,1,1,1,1,1,1,1,1,1,1,1,1,1,1,1,1,1,1,4),(0.,
0.0448889834294934),(11.8615800042567,12.8591513772396,13.8567227502225,
14.8542941232054,15.8518654961884,16.8494368691713,17.8470082421542,18.8445796151372,
19.8421509881201,20.839722361103,21.837293734086,22.8348651070689,23.8324364800518,
24.8300078530348,25.8275792260177,26.8251505990006,27.8227219719836,28.8202933449665,
29.8178647179494,30.8154360909324,31.8130074639153,32.8105788368982,33.8081502098812,
34.8057215828641,35.803292955847,36.80086432883,37.7984357018129,38.7960070747958,
39.7935784477788,40.7911498207617,41.7887211937446,42.7862925667276,43.7838639397105,
44.7814353126934,45.7790066856764,46.7765780586593,47.7741494316422,48.7717208046252,
49.7692921776081,50.766863550591,51.764434923574,52.7620062965569,53.7595776695398,
54.7571490425228,55.7547204155057,56.7522917884886,57.7498631614716,58.7474345344545,
59.7450059074374,60.7425772804204,61.7401486534033,62.7377200263862,63.7352913993692,
64.7328627723521,65.730434145335,66.728005518318,67.7255768913009,68.7231482642838,
69.7207196372668,70.7182910102497,71.7158623832326,72.7134337562156,73.7110051291985,
74.7085765021814,75.7061478751643,76.7037192481473,77.7012906211302,78.6988619941132,
79.6964333670961,80.694004740079,81.691576113062,82.6891474860449,83.6867188590278,
84.6842902320108,85.6818616049937,86.6794329779766,87.6770043509595,88.6745757239425,
89.6721470969254,90.6697184699083,91.6672898428913,92.6648612158742,93.6624325888571,
94.6600039618401),.UNSPECIFIED.);
#225=B_SPLINE_SURFACE_WITH_KNOTS('',3,3,((#27196,#27197,#27198,#27199,#27200,
#27201,#27202,#27203,#27204,#27205,#27206,#27207,#27208,#27209,#27210,#27211,
#27212,#27213,#27214,#27215,#27216,#27217,#27218,#27219,#27220,#27221,#27222,
#27223,#27224,#27225,#27226,#27227,#27228,#27229,#27230,#27231,#27232,#27233,
#27234,#27235,#27236,#27237,#27238,#27239,#27240,#27241,#27242,#27243,#27244,
#27245,#27246,#27247,#27248,#27249,#27250,#27251,#27252,#27253,#27254,#27255,
#27256,#27257,#27258,#27259,#27260,#27261,#27262,#27263,#27264,#27265,#27266,
#27267,#27268,#27269,#27270,#27271,#27272,#27273,#27274,#27275,#27276,#27277,
#27278,#27279,#27280,#27281),(#27282,#27283,#27284,#27285,#27286,#27287,
#27288,#27289,#27290,#27291,#27292,#27293,#27294,#27295,#27296,#27297,#27298,
#27299,#27300,#27301,#27302,#27303,#27304,#27305,#27306,#27307,#27308,#27309,
#27310,#27311,#27312,#27313,#27314,#27315,#27316,#27317,#27318,#27319,#27320,
#27321,#27322,#27323,#27324,#27325,#27326,#27327,#27328,#27329,#27330,#27331,
#27332,#27333,#27334,#27335,#27336,#27337,#27338,#27339,#27340,#27341,#27342,
#27343,#27344,#27345,#27346,#27347,#27348,#27349,#27350,#27351,#27352,#27353,
#27354,#27355,#27356,#27357,#27358,#27359,#27360,#27361,#27362,#27363,#27364,
#27365,#27366,#27367),(#27368,#27369,#27370,#27371,#27372,#27373,#27374,
#27375,#27376,#27377,#27378,#27379,#27380,#27381,#27382,#27383,#27384,#27385,
#27386,#27387,#27388,#27389,#27390,#27391,#27392,#27393,#27394,#27395,#27396,
#27397,#27398,#27399,#27400,#27401,#27402,#27403,#27404,#27405,#27406,#27407,
#27408,#27409,#27410,#27411,#27412,#27413,#27414,#27415,#27416,#27417,#27418,
#27419,#27420,#27421,#27422,#27423,#27424,#27425,#27426,#27427,#27428,#27429,
#27430,#27431,#27432,#27433,#27434,#27435,#27436,#27437,#27438,#27439,#27440,
#27441,#27442,#27443,#27444,#27445,#27446,#27447,#27448,#27449,#27450,#27451,
#27452,#27453),(#27454,#27455,#27456,#27457,#27458,#27459,#27460,#27461,
#27462,#27463,#27464,#27465,#27466,#27467,#27468,#27469,#27470,#27471,#27472,
#27473,#27474,#27475,#27476,#27477,#27478,#27479,#27480,#27481,#27482,#27483,
#27484,#27485,#27486,#27487,#27488,#27489,#27490,#27491,#27492,#27493,#27494,
#27495,#27496,#27497,#27498,#27499,#27500,#27501,#27502,#27503,#27504,#27505,
#27506,#27507,#27508,#27509,#27510,#27511,#27512,#27513,#27514,#27515,#27516,
#27517,#27518,#27519,#27520,#27521,#27522,#27523,#27524,#27525,#27526,#27527,
#27528,#27529,#27530,#27531,#27532,#27533,#27534,#27535,#27536,#27537,#27538,
#27539)),.UNSPECIFIED.,.F.,.F.,.F.,(4,4),(4,1,1,1,1,1,1,1,1,1,1,1,1,1,1,
1,1,1,1,1,1,1,1,1,1,1,1,1,1,1,1,1,1,1,1,1,1,1,1,1,1,1,1,1,1,1,1,1,1,1,1,
1,1,1,1,1,1,1,1,1,1,1,1,1,1,1,1,1,1,1,1,1,1,1,1,1,1,1,1,1,1,1,1,4),(0.,
0.0448889834294934),(14.3981410127769,15.3957123857598,16.3932837587428,
17.3908551317257,18.3884265047086,19.3859978776916,20.3835692506745,21.3811406236574,
22.3787119966404,23.3762833696233,24.3738547426062,25.3714261155892,26.3689974885721,
27.366568861555,28.364140234538,29.3617116075209,30.3592829805038,31.3568543534868,
32.3544257264697,33.3519970994526,34.3495684724355,35.3471398454185,36.3447112184014,
37.3422825913843,38.3398539643673,39.3374253373502,40.3349967103331,41.3325680833161,
42.330139456299,43.3277108292819,44.3252822022649,45.3228535752478,46.3204249482307,
47.3179963212137,48.3155676941966,49.3131390671795,50.3107104401625,51.3082818131454,
52.3058531861283,53.3034245591113,54.3009959320942,55.2985673050771,56.2961386780601,
57.293710051043,58.2912814240259,59.2888527970089,60.2864241699918,61.2839955429747,
62.2815669159577,63.2791382889406,64.2767096619235,65.2742810349065,66.2718524078894,
67.2694237808723,68.2669951538553,69.2645665268382,70.2621378998211,71.2597092728041,
72.257280645787,73.2548520187699,74.2524233917529,75.2499947647358,76.2475661377187,
77.2451375107017,78.2427088836846,79.2402802566675,80.2378516296505,81.2354230026334,
82.2329943756163,83.2305657485993,84.2281371215822,85.2257084945651,86.2232798675481,
87.220851240531,88.2184226135139,89.2159939864969,90.2135653594798,91.2111367324627,
92.2087081054457,93.2062794784286,94.2038508514115,95.2014222243944,96.1989935973774,
97.1965649703603),.UNSPECIFIED.);
#226=B_SPLINE_SURFACE_WITH_KNOTS('',3,3,((#28474,#28475,#28476,#28477,#28478,
#28479,#28480,#28481,#28482,#28483,#28484,#28485,#28486,#28487,#28488,#28489,
#28490,#28491,#28492,#28493,#28494,#28495,#28496,#28497,#28498,#28499,#28500,
#28501,#28502,#28503,#28504,#28505,#28506,#28507,#28508,#28509,#28510,#28511,
#28512,#28513,#28514,#28515,#28516,#28517,#28518,#28519,#28520,#28521,#28522,
#28523,#28524,#28525,#28526,#28527,#28528,#28529,#28530,#28531,#28532,#28533,
#28534,#28535,#28536,#28537,#28538,#28539,#28540,#28541),(#28542,#28543,
#28544,#28545,#28546,#28547,#28548,#28549,#28550,#28551,#28552,#28553,#28554,
#28555,#28556,#28557,#28558,#28559,#28560,#28561,#28562,#28563,#28564,#28565,
#28566,#28567,#28568,#28569,#28570,#28571,#28572,#28573,#28574,#28575,#28576,
#28577,#28578,#28579,#28580,#28581,#28582,#28583,#28584,#28585,#28586,#28587,
#28588,#28589,#28590,#28591,#28592,#28593,#28594,#28595,#28596,#28597,#28598,
#28599,#28600,#28601,#28602,#28603,#28604,#28605,#28606,#28607,#28608,#28609),
(#28610,#28611,#28612,#28613,#28614,#28615,#28616,#28617,#28618,#28619,
#28620,#28621,#28622,#28623,#28624,#28625,#28626,#28627,#28628,#28629,#28630,
#28631,#28632,#28633,#28634,#28635,#28636,#28637,#28638,#28639,#28640,#28641,
#28642,#28643,#28644,#28645,#28646,#28647,#28648,#28649,#28650,#28651,#28652,
#28653,#28654,#28655,#28656,#28657,#28658,#28659,#28660,#28661,#28662,#28663,
#28664,#28665,#28666,#28667,#28668,#28669,#28670,#28671,#28672,#28673,#28674,
#28675,#28676,#28677),(#28678,#28679,#28680,#28681,#28682,#28683,#28684,
#28685,#28686,#28687,#28688,#28689,#28690,#28691,#28692,#28693,#28694,#28695,
#28696,#28697,#28698,#28699,#28700,#28701,#28702,#28703,#28704,#28705,#28706,
#28707,#28708,#28709,#28710,#28711,#28712,#28713,#28714,#28715,#28716,#28717,
#28718,#28719,#28720,#28721,#28722,#28723,#28724,#28725,#28726,#28727,#28728,
#28729,#28730,#28731,#28732,#28733,#28734,#28735,#28736,#28737,#28738,#28739,
#28740,#28741,#28742,#28743,#28744,#28745)),.UNSPECIFIED.,.F.,.F.,.F.,(4,
4),(4,1,1,1,1,1,1,1,1,1,1,1,1,1,1,1,1,1,1,1,1,1,1,1,1,1,1,1,1,1,1,1,1,1,
1,1,1,1,1,1,1,1,1,1,1,1,1,1,1,1,1,1,1,1,1,1,1,1,1,1,1,1,1,1,1,4),(0.,0.0321584099938621),
(11.8553612635792,12.8530908876339,13.8508205116886,14.8485501357432,15.8462797597979,
16.8440093838525,17.8417390079072,18.8394686319618,19.8371982560165,20.8349278800712,
21.8326575041258,22.8303871281805,23.8281167522351,24.8258463762898,25.8235760003445,
26.8213056243991,27.8190352484538,28.8167648725084,29.8144944965631,30.8122241206177,
31.8099537446724,32.8076833687271,33.8054129927817,34.8031426168364,35.800872240891,
36.7986018649457,37.7963314890004,38.794061113055,39.7917907371097,40.7895203611643,
41.787249985219,42.7849796092736,43.7827092333283,44.780438857383,45.7781684814376,
46.7758981054923,47.7736277295469,48.7713573536016,49.7690869776563,50.7668166017109,
51.7645462257656,52.7622758498202,53.7600054738749,54.7577350979295,55.7554647219842,
56.7531943460389,57.7509239700935,58.7486535941482,59.7463832182028,60.7441128422575,
61.7418424663121,62.7395720903668,63.7373017144215,64.7350313384761,65.7327609625308,
66.7304905865854,67.7282202106401,68.7259498346948,69.7236794587494,70.7214090828041,
71.7191387068587,72.7168683309134,73.7145979549681,74.7123275790227,75.7100572030774,
76.707786827132),.UNSPECIFIED.);
#227=B_SPLINE_SURFACE_WITH_KNOTS('',3,3,((#28820,#28821,#28822,#28823,#28824,
#28825,#28826,#28827,#28828,#28829,#28830,#28831,#28832,#28833,#28834,#28835,
#28836,#28837,#28838,#28839,#28840,#28841,#28842,#28843,#28844,#28845,#28846,
#28847,#28848,#28849,#28850,#28851,#28852,#28853,#28854,#28855,#28856,#28857,
#28858,#28859,#28860,#28861,#28862,#28863,#28864,#28865,#28866,#28867,#28868,
#28869,#28870,#28871,#28872,#28873,#28874,#28875,#28876,#28877,#28878,#28879,
#28880,#28881,#28882,#28883,#28884,#28885,#28886,#28887),(#28888,#28889,
#28890,#28891,#28892,#28893,#28894,#28895,#28896,#28897,#28898,#28899,#28900,
#28901,#28902,#28903,#28904,#28905,#28906,#28907,#28908,#28909,#28910,#28911,
#28912,#28913,#28914,#28915,#28916,#28917,#28918,#28919,#28920,#28921,#28922,
#28923,#28924,#28925,#28926,#28927,#28928,#28929,#28930,#28931,#28932,#28933,
#28934,#28935,#28936,#28937,#28938,#28939,#28940,#28941,#28942,#28943,#28944,
#28945,#28946,#28947,#28948,#28949,#28950,#28951,#28952,#28953,#28954,#28955),
(#28956,#28957,#28958,#28959,#28960,#28961,#28962,#28963,#28964,#28965,
#28966,#28967,#28968,#28969,#28970,#28971,#28972,#28973,#28974,#28975,#28976,
#28977,#28978,#28979,#28980,#28981,#28982,#28983,#28984,#28985,#28986,#28987,
#28988,#28989,#28990,#28991,#28992,#28993,#28994,#28995,#28996,#28997,#28998,
#28999,#29000,#29001,#29002,#29003,#29004,#29005,#29006,#29007,#29008,#29009,
#29010,#29011,#29012,#29013,#29014,#29015,#29016,#29017,#29018,#29019,#29020,
#29021,#29022,#29023),(#29024,#29025,#29026,#29027,#29028,#29029,#29030,
#29031,#29032,#29033,#29034,#29035,#29036,#29037,#29038,#29039,#29040,#29041,
#29042,#29043,#29044,#29045,#29046,#29047,#29048,#29049,#29050,#29051,#29052,
#29053,#29054,#29055,#29056,#29057,#29058,#29059,#29060,#29061,#29062,#29063,
#29064,#29065,#29066,#29067,#29068,#29069,#29070,#29071,#29072,#29073,#29074,
#29075,#29076,#29077,#29078,#29079,#29080,#29081,#29082,#29083,#29084,#29085,
#29086,#29087,#29088,#29089,#29090,#29091)),.UNSPECIFIED.,.F.,.F.,.F.,(4,
4),(4,1,1,1,1,1,1,1,1,1,1,1,1,1,1,1,1,1,1,1,1,1,1,1,1,1,1,1,1,1,1,1,1,1,
1,1,1,1,1,1,1,1,1,1,1,1,1,1,1,1,1,1,1,1,1,1,1,1,1,1,1,1,1,1,1,4),(0.,0.0321584099938616),
(14.3984001269718,15.3961297510265,16.3938593750811,17.3915889991358,18.3893186231905,
19.3870482472451,20.3847778712998,21.3825074953544,22.3802371194091,23.3779667434637,
24.3756963675184,25.3734259915731,26.3711556156277,27.3688852396824,28.366614863737,
29.3643444877917,30.3620741118463,31.359803735901,32.3575333599556,33.3552629840103,
34.352992608065,35.3507222321196,36.3484518561743,37.3461814802289,38.3439111042836,
39.3416407283382,40.3393703523929,41.3370999764475,42.3348296005022,43.3325592245569,
44.3302888486115,45.3280184726662,46.3257480967208,47.3234777207755,48.3212073448301,
49.3189369688848,50.3166665929395,51.3143962169941,52.3121258410488,53.3098554651034,
54.3075850891581,55.3053147132127,56.3030443372674,57.3007739613221,58.2985035853767,
59.2962332094314,60.293962833486,61.2916924575407,62.2894220815953,63.28715170565,
64.2848813297046,65.2826109537593,66.280340577814,67.2780702018686,68.2757998259233,
69.2735294499779,70.2712590740326,71.2689886980872,72.2667183221419,73.2644479461966,
74.2621775702512,75.2599071943059,76.2576368183605,77.2553664424152,78.2530960664698,
79.2508256905245),.UNSPECIFIED.);
#228=B_SPLINE_SURFACE_WITH_KNOTS('',3,3,((#29315,#29316,#29317,#29318,#29319,
#29320,#29321,#29322,#29323,#29324,#29325,#29326,#29327,#29328,#29329,#29330,
#29331,#29332,#29333,#29334,#29335,#29336,#29337,#29338,#29339,#29340,#29341,
#29342,#29343),(#29344,#29345,#29346,#29347,#29348,#29349,#29350,#29351,
#29352,#29353,#29354,#29355,#29356,#29357,#29358,#29359,#29360,#29361,#29362,
#29363,#29364,#29365,#29366,#29367,#29368,#29369,#29370,#29371,#29372),
(#29373,#29374,#29375,#29376,#29377,#29378,#29379,#29380,#29381,#29382,
#29383,#29384,#29385,#29386,#29387,#29388,#29389,#29390,#29391,#29392,#29393,
#29394,#29395,#29396,#29397,#29398,#29399,#29400,#29401),(#29402,#29403,
#29404,#29405,#29406,#29407,#29408,#29409,#29410,#29411,#29412,#29413,#29414,
#29415,#29416,#29417,#29418,#29419,#29420,#29421,#29422,#29423,#29424,#29425,
#29426,#29427,#29428,#29429,#29430),(#29431,#29432,#29433,#29434,#29435,
#29436,#29437,#29438,#29439,#29440,#29441,#29442,#29443,#29444,#29445,#29446,
#29447,#29448,#29449,#29450,#29451,#29452,#29453,#29454,#29455,#29456,#29457,
#29458,#29459),(#29460,#29461,#29462,#29463,#29464,#29465,#29466,#29467,
#29468,#29469,#29470,#29471,#29472,#29473,#29474,#29475,#29476,#29477,#29478,
#29479,#29480,#29481,#29482,#29483,#29484,#29485,#29486,#29487,#29488),
(#29489,#29490,#29491,#29492,#29493,#29494,#29495,#29496,#29497,#29498,
#29499,#29500,#29501,#29502,#29503,#29504,#29505,#29506,#29507,#29508,#29509,
#29510,#29511,#29512,#29513,#29514,#29515,#29516,#29517),(#29518,#29519,
#29520,#29521,#29522,#29523,#29524,#29525,#29526,#29527,#29528,#29529,#29530,
#29531,#29532,#29533,#29534,#29535,#29536,#29537,#29538,#29539,#29540,#29541,
#29542,#29543,#29544,#29545,#29546),(#29547,#29548,#29549,#29550,#29551,
#29552,#29553,#29554,#29555,#29556,#29557,#29558,#29559,#29560,#29561,#29562,
#29563,#29564,#29565,#29566,#29567,#29568,#29569,#29570,#29571,#29572,#29573,
#29574,#29575),(#29576,#29577,#29578,#29579,#29580,#29581,#29582,#29583,
#29584,#29585,#29586,#29587,#29588,#29589,#29590,#29591,#29592,#29593,#29594,
#29595,#29596,#29597,#29598,#29599,#29600,#29601,#29602,#29603,#29604)),
 .UNSPECIFIED.,.T.,.F.,.F.,(4,1,1,1,1,1,1,4),(4,1,1,1,1,1,1,1,1,1,1,1,1,
1,1,1,1,1,1,1,1,1,1,1,1,1,4),(-3.14159265358979,-2.24399475256414,-1.34639685153848,
-0.448798950512828,0.448798950512828,1.34639685153848,2.24399475256414,
3.14159265358979),(0.,0.483321946706122,0.966643893412244,1.44996584011837,
1.93328778682449,2.41660973353061,2.89993168023673,3.38325362694285,3.86657557364898,
4.3498975203551,4.83321946706122,5.31654141376734,5.79986336047346,6.28318530717959,
6.76650725388571,7.24982920059183,7.73315114729795,8.21647309400407,8.6997950407102,
9.18311698741632,9.66643893412244,10.1497608808286,10.6330828275347,11.1164047742408,
11.5997267209469,12.083048667653,12.5663706143592),.UNSPECIFIED.);
#229=B_SPLINE_SURFACE_WITH_KNOTS('',3,3,((#30990,#30991,#30992,#30993,#30994,
#30995,#30996,#30997,#30998,#30999,#31000,#31001,#31002,#31003,#31004,#31005,
#31006,#31007,#31008,#31009,#31010,#31011,#31012,#31013,#31014,#31015,#31016,
#31017,#31018,#31019,#31020,#31021,#31022,#31023,#31024,#31025,#31026,#31027,
#31028,#31029,#31030,#31031,#31032,#31033,#31034,#31035,#31036,#31037,#31038,
#31039,#31040,#31041,#31042,#31043,#31044,#31045,#31046,#31047,#31048,#31049,
#31050,#31051,#31052,#31053,#31054,#31055,#31056,#31057,#31058,#31059,#31060,
#31061,#31062,#31063,#31064,#31065,#31066,#31067,#31068,#31069,#31070,#31071,
#31072,#31073,#31074,#31075,#31076,#31077,#31078,#31079,#31080,#31081,#31082,
#31083,#31084,#31085,#31086,#31087,#31088,#31089,#31090,#31091,#31092,#31093,
#31094,#31095),(#31096,#31097,#31098,#31099,#31100,#31101,#31102,#31103,
#31104,#31105,#31106,#31107,#31108,#31109,#31110,#31111,#31112,#31113,#31114,
#31115,#31116,#31117,#31118,#31119,#31120,#31121,#31122,#31123,#31124,#31125,
#31126,#31127,#31128,#31129,#31130,#31131,#31132,#31133,#31134,#31135,#31136,
#31137,#31138,#31139,#31140,#31141,#31142,#31143,#31144,#31145,#31146,#31147,
#31148,#31149,#31150,#31151,#31152,#31153,#31154,#31155,#31156,#31157,#31158,
#31159,#31160,#31161,#31162,#31163,#31164,#31165,#31166,#31167,#31168,#31169,
#31170,#31171,#31172,#31173,#31174,#31175,#31176,#31177,#31178,#31179,#31180,
#31181,#31182,#31183,#31184,#31185,#31186,#31187,#31188,#31189,#31190,#31191,
#31192,#31193,#31194,#31195,#31196,#31197,#31198,#31199,#31200,#31201),
(#31202,#31203,#31204,#31205,#31206,#31207,#31208,#31209,#31210,#31211,
#31212,#31213,#31214,#31215,#31216,#31217,#31218,#31219,#31220,#31221,#31222,
#31223,#31224,#31225,#31226,#31227,#31228,#31229,#31230,#31231,#31232,#31233,
#31234,#31235,#31236,#31237,#31238,#31239,#31240,#31241,#31242,#31243,#31244,
#31245,#31246,#31247,#31248,#31249,#31250,#31251,#31252,#31253,#31254,#31255,
#31256,#31257,#31258,#31259,#31260,#31261,#31262,#31263,#31264,#31265,#31266,
#31267,#31268,#31269,#31270,#31271,#31272,#31273,#31274,#31275,#31276,#31277,
#31278,#31279,#31280,#31281,#31282,#31283,#31284,#31285,#31286,#31287,#31288,
#31289,#31290,#31291,#31292,#31293,#31294,#31295,#31296,#31297,#31298,#31299,
#31300,#31301,#31302,#31303,#31304,#31305,#31306,#31307),(#31308,#31309,
#31310,#31311,#31312,#31313,#31314,#31315,#31316,#31317,#31318,#31319,#31320,
#31321,#31322,#31323,#31324,#31325,#31326,#31327,#31328,#31329,#31330,#31331,
#31332,#31333,#31334,#31335,#31336,#31337,#31338,#31339,#31340,#31341,#31342,
#31343,#31344,#31345,#31346,#31347,#31348,#31349,#31350,#31351,#31352,#31353,
#31354,#31355,#31356,#31357,#31358,#31359,#31360,#31361,#31362,#31363,#31364,
#31365,#31366,#31367,#31368,#31369,#31370,#31371,#31372,#31373,#31374,#31375,
#31376,#31377,#31378,#31379,#31380,#31381,#31382,#31383,#31384,#31385,#31386,
#31387,#31388,#31389,#31390,#31391,#31392,#31393,#31394,#31395,#31396,#31397,
#31398,#31399,#31400,#31401,#31402,#31403,#31404,#31405,#31406,#31407,#31408,
#31409,#31410,#31411,#31412,#31413)),.UNSPECIFIED.,.F.,.F.,.F.,(4,4),(4,
1,1,1,1,1,1,1,1,1,1,1,1,1,1,1,1,1,1,1,1,1,1,1,1,1,1,1,1,1,1,1,1,1,1,1,1,
1,1,1,1,1,1,1,1,1,1,1,1,1,1,1,1,1,1,1,1,1,1,1,1,1,1,1,1,1,1,1,1,1,1,1,1,
1,1,1,1,1,1,1,1,1,1,1,1,1,1,1,1,1,1,1,1,1,1,1,1,1,1,1,1,1,1,4),(0.,0.0460148164544132),
(11.6154215191105,12.6127573616628,13.610093204215,14.6074290467673,15.6047648893195,
16.6021007318718,17.599436574424,18.5967724169762,19.5941082595285,20.5914441020807,
21.588779944633,22.5861157871852,23.5834516297375,24.5807874722897,25.5781233148419,
26.5754591573942,27.5727949999464,28.5701308424987,29.5674666850509,30.5648025276032,
31.5621383701554,32.5594742127077,33.5568100552599,34.5541458978121,35.5514817403644,
36.5488175829166,37.5461534254689,38.5434892680211,39.5408251105734,40.5381609531256,
41.5354967956779,42.5328326382301,43.5301684807823,44.5275043233346,45.5248401658868,
46.5221760084391,47.5195118509913,48.5168476935436,49.5141835360958,50.5115193786481,
51.5088552212003,52.5061910637525,53.5035269063048,54.500862748857,55.4981985914093,
56.4955344339615,57.4928702765138,58.490206119066,59.4875419616182,60.4848778041705,
61.4822136467227,62.479549489275,63.4768853318272,64.4742211743795,65.4715570169317,
66.468892859484,67.4662287020362,68.4635645445884,69.4609003871407,70.4582362296929,
71.4555720722452,72.4529079147974,73.4502437573497,74.4475795999019,75.4449154424541,
76.4422512850064,77.4395871275586,78.4369229701109,79.4342588126631,80.4315946552154,
81.4289304977676,82.4262663403199,83.4236021828721,84.4209380254243,85.4182738679766,
86.4156097105288,87.4129455530811,88.4102813956333,89.4076172381856,90.4049530807378,
91.4022889232901,92.3996247658423,93.3969606083945,94.3942964509468,95.391632293499,
96.3889681360513,97.3863039786035,98.3836398211558,99.380975663708,100.37831150626,
101.375647348812,102.372983191365,103.370319033917,104.367654876469,105.364990719021,
106.362326561574,107.359662404126,108.356998246678,109.35433408923,110.351669931783,
111.349005774335,112.346341616887,113.343677459439,114.341013301992),
 .UNSPECIFIED.);
#230=B_SPLINE_SURFACE_WITH_KNOTS('',3,3,((#31506,#31507,#31508,#31509,#31510,
#31511,#31512,#31513,#31514,#31515,#31516,#31517,#31518,#31519,#31520,#31521,
#31522,#31523,#31524,#31525,#31526,#31527,#31528,#31529,#31530,#31531,#31532,
#31533,#31534,#31535,#31536,#31537,#31538,#31539,#31540,#31541,#31542,#31543,
#31544,#31545,#31546,#31547,#31548,#31549,#31550,#31551,#31552,#31553,#31554,
#31555,#31556,#31557,#31558,#31559,#31560,#31561,#31562,#31563,#31564,#31565,
#31566,#31567,#31568,#31569,#31570,#31571,#31572,#31573,#31574,#31575,#31576,
#31577,#31578,#31579,#31580,#31581,#31582,#31583,#31584,#31585,#31586,#31587,
#31588,#31589,#31590,#31591,#31592,#31593,#31594,#31595,#31596,#31597,#31598,
#31599,#31600,#31601,#31602,#31603,#31604,#31605,#31606,#31607,#31608,#31609,
#31610,#31611,#31612,#31613),(#31614,#31615,#31616,#31617,#31618,#31619,
#31620,#31621,#31622,#31623,#31624,#31625,#31626,#31627,#31628,#31629,#31630,
#31631,#31632,#31633,#31634,#31635,#31636,#31637,#31638,#31639,#31640,#31641,
#31642,#31643,#31644,#31645,#31646,#31647,#31648,#31649,#31650,#31651,#31652,
#31653,#31654,#31655,#31656,#31657,#31658,#31659,#31660,#31661,#31662,#31663,
#31664,#31665,#31666,#31667,#31668,#31669,#31670,#31671,#31672,#31673,#31674,
#31675,#31676,#31677,#31678,#31679,#31680,#31681,#31682,#31683,#31684,#31685,
#31686,#31687,#31688,#31689,#31690,#31691,#31692,#31693,#31694,#31695,#31696,
#31697,#31698,#31699,#31700,#31701,#31702,#31703,#31704,#31705,#31706,#31707,
#31708,#31709,#31710,#31711,#31712,#31713,#31714,#31715,#31716,#31717,#31718,
#31719,#31720,#31721),(#31722,#31723,#31724,#31725,#31726,#31727,#31728,
#31729,#31730,#31731,#31732,#31733,#31734,#31735,#31736,#31737,#31738,#31739,
#31740,#31741,#31742,#31743,#31744,#31745,#31746,#31747,#31748,#31749,#31750,
#31751,#31752,#31753,#31754,#31755,#31756,#31757,#31758,#31759,#31760,#31761,
#31762,#31763,#31764,#31765,#31766,#31767,#31768,#31769,#31770,#31771,#31772,
#31773,#31774,#31775,#31776,#31777,#31778,#31779,#31780,#31781,#31782,#31783,
#31784,#31785,#31786,#31787,#31788,#31789,#31790,#31791,#31792,#31793,#31794,
#31795,#31796,#31797,#31798,#31799,#31800,#31801,#31802,#31803,#31804,#31805,
#31806,#31807,#31808,#31809,#31810,#31811,#31812,#31813,#31814,#31815,#31816,
#31817,#31818,#31819,#31820,#31821,#31822,#31823,#31824,#31825,#31826,#31827,
#31828,#31829),(#31830,#31831,#31832,#31833,#31834,#31835,#31836,#31837,
#31838,#31839,#31840,#31841,#31842,#31843,#31844,#31845,#31846,#31847,#31848,
#31849,#31850,#31851,#31852,#31853,#31854,#31855,#31856,#31857,#31858,#31859,
#31860,#31861,#31862,#31863,#31864,#31865,#31866,#31867,#31868,#31869,#31870,
#31871,#31872,#31873,#31874,#31875,#31876,#31877,#31878,#31879,#31880,#31881,
#31882,#31883,#31884,#31885,#31886,#31887,#31888,#31889,#31890,#31891,#31892,
#31893,#31894,#31895,#31896,#31897,#31898,#31899,#31900,#31901,#31902,#31903,
#31904,#31905,#31906,#31907,#31908,#31909,#31910,#31911,#31912,#31913,#31914,
#31915,#31916,#31917,#31918,#31919,#31920,#31921,#31922,#31923,#31924,#31925,
#31926,#31927,#31928,#31929,#31930,#31931,#31932,#31933,#31934,#31935,#31936,
#31937)),.UNSPECIFIED.,.F.,.F.,.F.,(4,4),(4,1,1,1,1,1,1,1,1,1,1,1,1,1,1,
1,1,1,1,1,1,1,1,1,1,1,1,1,1,1,1,1,1,1,1,1,1,1,1,1,1,1,1,1,1,1,1,1,1,1,1,
1,1,1,1,1,1,1,1,1,1,1,1,1,1,1,1,1,1,1,1,1,1,1,1,1,1,1,1,1,1,1,1,1,1,1,1,
1,1,1,1,1,1,1,1,1,1,1,1,1,1,1,1,1,1,4),(0.,0.0460148164544132),(8.31058692273969,
9.30859389336977,10.3066008639999,11.30460783463,12.30261480526,13.3006217758901,
14.2986287465202,15.2966357171503,16.2946426877804,17.2926496584105,18.2906566290406,
19.2886635996707,20.2866705703008,21.2846775409308,22.2826845115609,23.280691482191,
24.2786984528211,25.2767054234512,26.2747123940813,27.2727193647114,28.2707263353415,
29.2687333059716,30.2667402766016,31.2647472472317,32.2627542178618,33.2607611884919,
34.258768159122,35.2567751297521,36.2547821003822,37.2527890710123,38.2507960416424,
39.2488030122724,40.2468099829025,41.2448169535326,42.2428239241627,43.2408308947928,
44.2388378654229,45.236844836053,46.2348518066831,47.2328587773132,48.2308657479432,
49.2288727185733,50.2268796892034,51.2248866598335,52.2228936304636,53.2209006010937,
54.2189075717238,55.2169145423539,56.214921512984,57.212928483614,58.2109354542441,
59.2089424248742,60.2069493955043,61.2049563661344,62.2029633367645,63.2009703073946,
64.1989772780247,65.1969842486548,66.1949912192848,67.1929981899149,68.191005160545,
69.1890121311751,70.1870191018052,71.1850260724353,72.1830330430654,73.1810400136955,
74.1790469843256,75.1770539549557,76.1750609255857,77.1730678962158,78.1710748668459,
79.169081837476,80.1670888081061,81.1650957787362,82.1631027493663,83.1611097199964,
84.1591166906264,85.1571236612565,86.1551306318866,87.1531376025167,88.1511445731468,
89.1491515437769,90.147158514407,91.1451654850371,92.1431724556672,93.1411794262973,
94.1391863969273,95.1371933675574,96.1352003381875,97.1332073088176,98.1312142794477,
99.1292212500778,100.127228220708,101.125235191338,102.123242161968,103.121249132598,
104.119256103228,105.117263073858,106.115270044488,107.113277015118,108.111283985749,
109.109290956379,110.107297927009,111.105304897639,112.103311868269,113.101318838899),
 .UNSPECIFIED.);
#231=B_SPLINE_SURFACE_WITH_KNOTS('',3,3,((#32953,#32954,#32955,#32956,#32957,
#32958,#32959,#32960,#32961,#32962,#32963,#32964,#32965,#32966,#32967,#32968,
#32969,#32970,#32971,#32972,#32973,#32974,#32975,#32976,#32977,#32978,#32979,
#32980,#32981,#32982,#32983,#32984,#32985,#32986,#32987,#32988,#32989,#32990,
#32991,#32992,#32993,#32994,#32995,#32996,#32997,#32998,#32999,#33000,#33001,
#33002,#33003,#33004,#33005,#33006,#33007,#33008,#33009,#33010,#33011,#33012,
#33013,#33014,#33015,#33016,#33017,#33018,#33019,#33020,#33021,#33022),
(#33023,#33024,#33025,#33026,#33027,#33028,#33029,#33030,#33031,#33032,
#33033,#33034,#33035,#33036,#33037,#33038,#33039,#33040,#33041,#33042,#33043,
#33044,#33045,#33046,#33047,#33048,#33049,#33050,#33051,#33052,#33053,#33054,
#33055,#33056,#33057,#33058,#33059,#33060,#33061,#33062,#33063,#33064,#33065,
#33066,#33067,#33068,#33069,#33070,#33071,#33072,#33073,#33074,#33075,#33076,
#33077,#33078,#33079,#33080,#33081,#33082,#33083,#33084,#33085,#33086,#33087,
#33088,#33089,#33090,#33091,#33092),(#33093,#33094,#33095,#33096,#33097,
#33098,#33099,#33100,#33101,#33102,#33103,#33104,#33105,#33106,#33107,#33108,
#33109,#33110,#33111,#33112,#33113,#33114,#33115,#33116,#33117,#33118,#33119,
#33120,#33121,#33122,#33123,#33124,#33125,#33126,#33127,#33128,#33129,#33130,
#33131,#33132,#33133,#33134,#33135,#33136,#33137,#33138,#33139,#33140,#33141,
#33142,#33143,#33144,#33145,#33146,#33147,#33148,#33149,#33150,#33151,#33152,
#33153,#33154,#33155,#33156,#33157,#33158,#33159,#33160,#33161,#33162),
(#33163,#33164,#33165,#33166,#33167,#33168,#33169,#33170,#33171,#33172,
#33173,#33174,#33175,#33176,#33177,#33178,#33179,#33180,#33181,#33182,#33183,
#33184,#33185,#33186,#33187,#33188,#33189,#33190,#33191,#33192,#33193,#33194,
#33195,#33196,#33197,#33198,#33199,#33200,#33201,#33202,#33203,#33204,#33205,
#33206,#33207,#33208,#33209,#33210,#33211,#33212,#33213,#33214,#33215,#33216,
#33217,#33218,#33219,#33220,#33221,#33222,#33223,#33224,#33225,#33226,#33227,
#33228,#33229,#33230,#33231,#33232)),.UNSPECIFIED.,.F.,.F.,.F.,(4,4),(4,
1,1,1,1,1,1,1,1,1,1,1,1,1,1,1,1,1,1,1,1,1,1,1,1,1,1,1,1,1,1,1,1,1,1,1,1,
1,1,1,1,1,1,1,1,1,1,1,1,1,1,1,1,1,1,1,1,1,1,1,1,1,1,1,1,1,1,4),(0.,0.0329955678841871),
(11.6159397475004,12.6141690908179,13.6123984341354,14.6106277774529,15.6088571207704,
16.6070864640879,17.6053158074054,18.6035451507229,19.6017744940404,20.600003837358,
21.5982331806755,22.596462523993,23.5946918673105,24.592921210628,25.5911505539455,
26.589379897263,27.5876092405805,28.585838583898,29.5840679272155,30.5822972705331,
31.5805266138506,32.5787559571681,33.5769853004856,34.5752146438031,35.5734439871206,
36.5716733304381,37.5699026737556,38.5681320170731,39.5663613603907,40.5645907037082,
41.5628200470257,42.5610493903432,43.5592787336607,44.5575080769782,45.5557374202957,
46.5539667636132,47.5521961069307,48.5504254502482,49.5486547935658,50.5468841368833,
51.5451134802008,52.5433428235183,53.5415721668358,54.5398015101533,55.5380308534708,
56.5362601967883,57.5344895401058,58.5327188834233,59.5309482267409,60.5291775700584,
61.5274069133759,62.5256362566934,63.5238656000109,64.5220949433284,65.5203242866459,
66.5185536299634,67.5167829732809,68.5150123165984,69.513241659916,70.5114710032335,
71.509700346551,72.5079296898685,73.506159033186,74.5043883765035,75.502617719821,
76.5008470631385,77.499076406456,78.4973057497735),.UNSPECIFIED.);
#232=B_SPLINE_SURFACE_WITH_KNOTS('',3,3,((#33322,#33323,#33324,#33325,#33326,
#33327,#33328,#33329,#33330,#33331,#33332,#33333,#33334,#33335,#33336,#33337,
#33338,#33339,#33340,#33341,#33342,#33343,#33344,#33345,#33346,#33347,#33348,
#33349,#33350,#33351,#33352,#33353,#33354,#33355,#33356,#33357,#33358,#33359,
#33360,#33361,#33362,#33363,#33364,#33365,#33366,#33367,#33368,#33369,#33370,
#33371,#33372,#33373,#33374,#33375,#33376,#33377,#33378,#33379,#33380,#33381,
#33382,#33383,#33384,#33385,#33386,#33387,#33388,#33389,#33390,#33391,#33392,
#33393),(#33394,#33395,#33396,#33397,#33398,#33399,#33400,#33401,#33402,
#33403,#33404,#33405,#33406,#33407,#33408,#33409,#33410,#33411,#33412,#33413,
#33414,#33415,#33416,#33417,#33418,#33419,#33420,#33421,#33422,#33423,#33424,
#33425,#33426,#33427,#33428,#33429,#33430,#33431,#33432,#33433,#33434,#33435,
#33436,#33437,#33438,#33439,#33440,#33441,#33442,#33443,#33444,#33445,#33446,
#33447,#33448,#33449,#33450,#33451,#33452,#33453,#33454,#33455,#33456,#33457,
#33458,#33459,#33460,#33461,#33462,#33463,#33464,#33465),(#33466,#33467,
#33468,#33469,#33470,#33471,#33472,#33473,#33474,#33475,#33476,#33477,#33478,
#33479,#33480,#33481,#33482,#33483,#33484,#33485,#33486,#33487,#33488,#33489,
#33490,#33491,#33492,#33493,#33494,#33495,#33496,#33497,#33498,#33499,#33500,
#33501,#33502,#33503,#33504,#33505,#33506,#33507,#33508,#33509,#33510,#33511,
#33512,#33513,#33514,#33515,#33516,#33517,#33518,#33519,#33520,#33521,#33522,
#33523,#33524,#33525,#33526,#33527,#33528,#33529,#33530,#33531,#33532,#33533,
#33534,#33535,#33536,#33537),(#33538,#33539,#33540,#33541,#33542,#33543,
#33544,#33545,#33546,#33547,#33548,#33549,#33550,#33551,#33552,#33553,#33554,
#33555,#33556,#33557,#33558,#33559,#33560,#33561,#33562,#33563,#33564,#33565,
#33566,#33567,#33568,#33569,#33570,#33571,#33572,#33573,#33574,#33575,#33576,
#33577,#33578,#33579,#33580,#33581,#33582,#33583,#33584,#33585,#33586,#33587,
#33588,#33589,#33590,#33591,#33592,#33593,#33594,#33595,#33596,#33597,#33598,
#33599,#33600,#33601,#33602,#33603,#33604,#33605,#33606,#33607,#33608,#33609)),
 .UNSPECIFIED.,.F.,.F.,.F.,(4,4),(4,1,1,1,1,1,1,1,1,1,1,1,1,1,1,1,1,1,1,
1,1,1,1,1,1,1,1,1,1,1,1,1,1,1,1,1,1,1,1,1,1,1,1,1,1,1,1,1,1,1,1,1,1,1,1,
1,1,1,1,1,1,1,1,1,1,1,1,1,1,4),(0.,0.0329955678841871),(8.30203615430834,
9.30137729453432,10.3007184347603,11.3000595749863,12.2994007152123,13.2987418554383,
14.2980829956642,15.2974241358902,16.2967652761162,17.2961064163422,18.2954475565682,
19.2947886967942,20.2941298370201,21.2934709772461,22.2928121174721,23.2921532576981,
24.2914943979241,25.2908355381501,26.290176678376,27.289517818602,28.288858958828,
29.288200099054,30.28754123928,31.286882379506,32.2862235197319,33.2855646599579,
34.2849058001839,35.2842469404099,36.2835880806359,37.2829292208619,38.2822703610879,
39.2816115013138,40.2809526415398,41.2802937817658,42.2796349219918,43.2789760622178,
44.2783172024438,45.2776583426697,46.2769994828957,47.2763406231217,48.2756817633477,
49.2750229035737,50.2743640437997,51.2737051840256,52.2730463242516,53.2723874644776,
54.2717286047036,55.2710697449296,56.2704108851556,57.2697520253815,58.2690931656075,
59.2684343058335,60.2677754460595,61.2671165862855,62.2664577265115,63.2657988667374,
64.2651400069634,65.2644811471894,66.2638222874154,67.2631634276414,68.2625045678674,
69.2618457080933,70.2611868483193,71.2605279885453,72.2598691287713,73.2592102689973,
74.2585514092233,75.2578925494492,76.2572336896752,77.2565748299012),
 .UNSPECIFIED.);
#233=B_SPLINE_SURFACE_WITH_KNOTS('',3,3,((#35222,#35223,#35224,#35225,#35226,
#35227,#35228,#35229,#35230,#35231,#35232,#35233,#35234,#35235,#35236,#35237,
#35238,#35239,#35240,#35241,#35242,#35243,#35244,#35245,#35246,#35247,#35248,
#35249,#35250,#35251,#35252,#35253,#35254,#35255,#35256,#35257,#35258,#35259,
#35260,#35261,#35262,#35263,#35264,#35265,#35266,#35267,#35268,#35269,#35270,
#35271,#35272,#35273,#35274,#35275,#35276,#35277,#35278,#35279,#35280,#35281,
#35282,#35283,#35284,#35285,#35286,#35287,#35288,#35289,#35290,#35291,#35292,
#35293,#35294,#35295,#35296,#35297,#35298,#35299,#35300,#35301,#35302,#35303,
#35304,#35305,#35306,#35307,#35308,#35309,#35310,#35311,#35312,#35313,#35314,
#35315,#35316,#35317,#35318,#35319,#35320,#35321,#35322,#35323,#35324,#35325,
#35326,#35327,#35328,#35329,#35330,#35331,#35332,#35333,#35334,#35335,#35336,
#35337,#35338,#35339,#35340,#35341,#35342),(#35343,#35344,#35345,#35346,
#35347,#35348,#35349,#35350,#35351,#35352,#35353,#35354,#35355,#35356,#35357,
#35358,#35359,#35360,#35361,#35362,#35363,#35364,#35365,#35366,#35367,#35368,
#35369,#35370,#35371,#35372,#35373,#35374,#35375,#35376,#35377,#35378,#35379,
#35380,#35381,#35382,#35383,#35384,#35385,#35386,#35387,#35388,#35389,#35390,
#35391,#35392,#35393,#35394,#35395,#35396,#35397,#35398,#35399,#35400,#35401,
#35402,#35403,#35404,#35405,#35406,#35407,#35408,#35409,#35410,#35411,#35412,
#35413,#35414,#35415,#35416,#35417,#35418,#35419,#35420,#35421,#35422,#35423,
#35424,#35425,#35426,#35427,#35428,#35429,#35430,#35431,#35432,#35433,#35434,
#35435,#35436,#35437,#35438,#35439,#35440,#35441,#35442,#35443,#35444,#35445,
#35446,#35447,#35448,#35449,#35450,#35451,#35452,#35453,#35454,#35455,#35456,
#35457,#35458,#35459,#35460,#35461,#35462,#35463),(#35464,#35465,#35466,
#35467,#35468,#35469,#35470,#35471,#35472,#35473,#35474,#35475,#35476,#35477,
#35478,#35479,#35480,#35481,#35482,#35483,#35484,#35485,#35486,#35487,#35488,
#35489,#35490,#35491,#35492,#35493,#35494,#35495,#35496,#35497,#35498,#35499,
#35500,#35501,#35502,#35503,#35504,#35505,#35506,#35507,#35508,#35509,#35510,
#35511,#35512,#35513,#35514,#35515,#35516,#35517,#35518,#35519,#35520,#35521,
#35522,#35523,#35524,#35525,#35526,#35527,#35528,#35529,#35530,#35531,#35532,
#35533,#35534,#35535,#35536,#35537,#35538,#35539,#35540,#35541,#35542,#35543,
#35544,#35545,#35546,#35547,#35548,#35549,#35550,#35551,#35552,#35553,#35554,
#35555,#35556,#35557,#35558,#35559,#35560,#35561,#35562,#35563,#35564,#35565,
#35566,#35567,#35568,#35569,#35570,#35571,#35572,#35573,#35574,#35575,#35576,
#35577,#35578,#35579,#35580,#35581,#35582,#35583,#35584),(#35585,#35586,
#35587,#35588,#35589,#35590,#35591,#35592,#35593,#35594,#35595,#35596,#35597,
#35598,#35599,#35600,#35601,#35602,#35603,#35604,#35605,#35606,#35607,#35608,
#35609,#35610,#35611,#35612,#35613,#35614,#35615,#35616,#35617,#35618,#35619,
#35620,#35621,#35622,#35623,#35624,#35625,#35626,#35627,#35628,#35629,#35630,
#35631,#35632,#35633,#35634,#35635,#35636,#35637,#35638,#35639,#35640,#35641,
#35642,#35643,#35644,#35645,#35646,#35647,#35648,#35649,#35650,#35651,#35652,
#35653,#35654,#35655,#35656,#35657,#35658,#35659,#35660,#35661,#35662,#35663,
#35664,#35665,#35666,#35667,#35668,#35669,#35670,#35671,#35672,#35673,#35674,
#35675,#35676,#35677,#35678,#35679,#35680,#35681,#35682,#35683,#35684,#35685,
#35686,#35687,#35688,#35689,#35690,#35691,#35692,#35693,#35694,#35695,#35696,
#35697,#35698,#35699,#35700,#35701,#35702,#35703,#35704,#35705)),
 .UNSPECIFIED.,.F.,.F.,.F.,(4,4),(4,1,1,1,1,1,1,1,1,1,1,1,1,1,1,1,1,1,1,
1,1,1,1,1,1,1,1,1,1,1,1,1,1,1,1,1,1,1,1,1,1,1,1,1,1,1,1,1,1,1,1,1,1,1,1,
1,1,1,1,1,1,1,1,1,1,1,1,1,1,1,1,1,1,1,1,1,1,1,1,1,1,1,1,1,1,1,1,1,1,1,1,
1,1,1,1,1,1,1,1,1,1,1,1,1,1,1,1,1,1,1,1,1,1,1,1,1,1,1,4),(0.,0.0329955678841871),
(11.6159397475003,12.6087096497013,13.6014795519022,14.5942494541031,15.5870193563041,
16.579789258505,17.5725591607059,18.5653290629068,19.5580989651078,20.5508688673087,
21.5436387695096,22.5364086717106,23.5291785739115,24.5219484761124,25.5147183783134,
26.5074882805143,27.5002581827152,28.4930280849161,29.4857979871171,30.478567889318,
31.4713377915189,32.4641076937199,33.4568775959208,34.4496474981217,35.4424174003227,
36.4351873025236,37.4279572047245,38.4207271069255,39.4134970091264,40.4062669113273,
41.3990368135282,42.3918067157292,43.3845766179301,44.377346520131,45.370116422332,
46.3628863245329,47.3556562267338,48.3484261289348,49.3411960311357,50.3339659333366,
51.3267358355376,52.3195057377385,53.3122756399394,54.3050455421403,55.2978154443413,
56.2905853465422,57.2833552487431,58.2761251509441,59.268895053145,60.2616649553459,
61.2544348575469,62.2472047597478,63.2399746619487,64.2327445641497,65.2255144663506,
66.2182843685515,67.2110542707524,68.2038241729534,69.1965940751543,70.1893639773552,
71.1821338795562,72.1749037817571,73.167673683958,74.160443586159,75.1532134883599,
76.1459833905608,77.1387532927618,78.1315231949627,79.1242930971636,80.1170629993645,
81.1098329015655,82.1026028037664,83.0953727059673,84.0881426081683,85.0809125103692,
86.0736824125701,87.0664523147711,88.059222216972,89.0519921191729,90.0447620213739,
91.0375319235748,92.0303018257757,93.0230717279766,94.0158416301776,95.0086115323785,
96.0013814345794,96.9941513367804,97.9869212389813,98.9796911411822,99.9724610433832,
100.965230945584,101.958000847785,102.950770749986,103.943540652187,104.936310554388,
105.929080456589,106.92185035879,107.914620260991,108.907390163192,109.900160065392,
110.892929967593,111.885699869794,112.878469771995,113.871239674196,114.864009576397,
115.856779478598,116.849549380799,117.842319283,118.835089185201,119.827859087402,
120.820628989603,121.813398891804,122.806168794005,123.798938696205,124.791708598406,
125.784478500607,126.777248402808,127.770018305009,128.76278820721),
 .UNSPECIFIED.);
#234=B_SPLINE_SURFACE_WITH_KNOTS('',3,3,((#35801,#35802,#35803,#35804,#35805,
#35806,#35807,#35808,#35809,#35810,#35811,#35812,#35813,#35814,#35815,#35816,
#35817,#35818,#35819,#35820,#35821,#35822,#35823,#35824,#35825,#35826,#35827,
#35828,#35829,#35830,#35831,#35832,#35833,#35834,#35835,#35836,#35837,#35838,
#35839,#35840,#35841,#35842,#35843,#35844,#35845,#35846,#35847,#35848,#35849,
#35850,#35851,#35852,#35853,#35854,#35855,#35856,#35857,#35858,#35859,#35860,
#35861,#35862,#35863,#35864,#35865,#35866,#35867,#35868,#35869,#35870,#35871,
#35872,#35873,#35874,#35875,#35876,#35877,#35878,#35879,#35880,#35881,#35882,
#35883,#35884,#35885,#35886,#35887,#35888,#35889,#35890,#35891,#35892,#35893,
#35894,#35895,#35896,#35897,#35898,#35899,#35900,#35901,#35902,#35903,#35904,
#35905,#35906,#35907,#35908,#35909,#35910,#35911,#35912,#35913,#35914,#35915,
#35916,#35917,#35918,#35919,#35920,#35921,#35922,#35923),(#35924,#35925,
#35926,#35927,#35928,#35929,#35930,#35931,#35932,#35933,#35934,#35935,#35936,
#35937,#35938,#35939,#35940,#35941,#35942,#35943,#35944,#35945,#35946,#35947,
#35948,#35949,#35950,#35951,#35952,#35953,#35954,#35955,#35956,#35957,#35958,
#35959,#35960,#35961,#35962,#35963,#35964,#35965,#35966,#35967,#35968,#35969,
#35970,#35971,#35972,#35973,#35974,#35975,#35976,#35977,#35978,#35979,#35980,
#35981,#35982,#35983,#35984,#35985,#35986,#35987,#35988,#35989,#35990,#35991,
#35992,#35993,#35994,#35995,#35996,#35997,#35998,#35999,#36000,#36001,#36002,
#36003,#36004,#36005,#36006,#36007,#36008,#36009,#36010,#36011,#36012,#36013,
#36014,#36015,#36016,#36017,#36018,#36019,#36020,#36021,#36022,#36023,#36024,
#36025,#36026,#36027,#36028,#36029,#36030,#36031,#36032,#36033,#36034,#36035,
#36036,#36037,#36038,#36039,#36040,#36041,#36042,#36043,#36044,#36045,#36046),
(#36047,#36048,#36049,#36050,#36051,#36052,#36053,#36054,#36055,#36056,
#36057,#36058,#36059,#36060,#36061,#36062,#36063,#36064,#36065,#36066,#36067,
#36068,#36069,#36070,#36071,#36072,#36073,#36074,#36075,#36076,#36077,#36078,
#36079,#36080,#36081,#36082,#36083,#36084,#36085,#36086,#36087,#36088,#36089,
#36090,#36091,#36092,#36093,#36094,#36095,#36096,#36097,#36098,#36099,#36100,
#36101,#36102,#36103,#36104,#36105,#36106,#36107,#36108,#36109,#36110,#36111,
#36112,#36113,#36114,#36115,#36116,#36117,#36118,#36119,#36120,#36121,#36122,
#36123,#36124,#36125,#36126,#36127,#36128,#36129,#36130,#36131,#36132,#36133,
#36134,#36135,#36136,#36137,#36138,#36139,#36140,#36141,#36142,#36143,#36144,
#36145,#36146,#36147,#36148,#36149,#36150,#36151,#36152,#36153,#36154,#36155,
#36156,#36157,#36158,#36159,#36160,#36161,#36162,#36163,#36164,#36165,#36166,
#36167,#36168,#36169),(#36170,#36171,#36172,#36173,#36174,#36175,#36176,
#36177,#36178,#36179,#36180,#36181,#36182,#36183,#36184,#36185,#36186,#36187,
#36188,#36189,#36190,#36191,#36192,#36193,#36194,#36195,#36196,#36197,#36198,
#36199,#36200,#36201,#36202,#36203,#36204,#36205,#36206,#36207,#36208,#36209,
#36210,#36211,#36212,#36213,#36214,#36215,#36216,#36217,#36218,#36219,#36220,
#36221,#36222,#36223,#36224,#36225,#36226,#36227,#36228,#36229,#36230,#36231,
#36232,#36233,#36234,#36235,#36236,#36237,#36238,#36239,#36240,#36241,#36242,
#36243,#36244,#36245,#36246,#36247,#36248,#36249,#36250,#36251,#36252,#36253,
#36254,#36255,#36256,#36257,#36258,#36259,#36260,#36261,#36262,#36263,#36264,
#36265,#36266,#36267,#36268,#36269,#36270,#36271,#36272,#36273,#36274,#36275,
#36276,#36277,#36278,#36279,#36280,#36281,#36282,#36283,#36284,#36285,#36286,
#36287,#36288,#36289,#36290,#36291,#36292)),.UNSPECIFIED.,.F.,.F.,.F.,(4,
4),(4,1,1,1,1,1,1,1,1,1,1,1,1,1,1,1,1,1,1,1,1,1,1,1,1,1,1,1,1,1,1,1,1,1,
1,1,1,1,1,1,1,1,1,1,1,1,1,1,1,1,1,1,1,1,1,1,1,1,1,1,1,1,1,1,1,1,1,1,1,1,
1,1,1,1,1,1,1,1,1,1,1,1,1,1,1,1,1,1,1,1,1,1,1,1,1,1,1,1,1,1,1,1,1,1,1,1,
1,1,1,1,1,1,1,1,1,1,1,1,1,1,4),(0.,0.0329955678841871),(8.30203615430831,
9.29553633041689,10.2890365065255,11.282536682634,12.2760368587426,13.2695370348512,
14.2630372109598,15.2565373870684,16.2500375631769,17.2435377392855,18.2370379153941,
19.2305380915027,20.2240382676113,21.2175384437198,22.2110386198284,23.204538795937,
24.1980389720456,25.1915391481542,26.1850393242627,27.1785395003713,28.1720396764799,
29.1655398525885,30.1590400286971,31.1525402048056,32.1460403809142,33.1395405570228,
34.1330407331314,35.1265409092399,36.1200410853485,37.1135412614571,38.1070414375657,
39.1005416136743,40.0940417897828,41.0875419658914,42.081042142,43.0745423181086,
44.0680424942172,45.0615426703257,46.0550428464343,47.0485430225429,48.0420431986515,
49.0355433747601,50.0290435508686,51.0225437269772,52.0160439030858,53.0095440791944,
54.003044255303,54.9965444314115,55.9900446075201,56.9835447836287,57.9770449597373,
58.9705451358458,59.9640453119544,60.957545488063,61.9510456641716,62.9445458402802,
63.9380460163887,64.9315461924973,65.9250463686059,66.9185465447145,67.9120467208231,
68.9055468969316,69.8990470730402,70.8925472491488,71.8860474252574,72.879547601366,
73.8730477774745,74.8665479535831,75.8600481296917,76.8535483058003,77.8470484819088,
78.8405486580174,79.834048834126,80.8275490102346,81.8210491863432,82.8145493624517,
83.8080495385603,84.8015497146689,85.7950498907775,86.7885500668861,87.7820502429946,
88.7755504191032,89.7690505952118,90.7625507713204,91.756050947429,92.7495511235375,
93.7430512996461,94.7365514757547,95.7300516518633,96.7235518279718,97.7170520040804,
98.710552180189,99.7040523562976,100.697552532406,101.691052708515,102.684552884623,
103.678053060732,104.67155323684,105.665053412949,106.658553589058,107.652053765166,
108.645553941275,109.639054117383,110.632554293492,111.626054469601,112.619554645709,
113.613054821818,114.606554997926,115.600055174035,116.593555350143,117.587055526252,
118.580555702361,119.574055878469,120.567556054578,121.561056230686,122.554556406795,
123.548056582903,124.541556759012,125.535056935121,126.528557111229,127.522057287338),
 .UNSPECIFIED.);
#235=FACE_BOUND('',#1083,.T.);
#236=FACE_BOUND('',#1084,.T.);
#237=FACE_BOUND('',#1085,.T.);
#238=FACE_BOUND('',#1087,.T.);
#239=FACE_BOUND('',#1091,.T.);
#240=FACE_BOUND('',#1095,.T.);
#241=FACE_BOUND('',#1128,.T.);
#242=FACE_BOUND('',#1133,.T.);
#243=FACE_BOUND('',#1137,.T.);
#244=FACE_BOUND('',#1143,.T.);
#245=FACE_BOUND('',#1146,.T.);
#246=FACE_BOUND('',#1147,.T.);
#247=FACE_BOUND('',#1148,.T.);
#248=FACE_BOUND('',#1149,.T.);
#249=FACE_BOUND('',#1150,.T.);
#250=FACE_BOUND('',#1152,.T.);
#251=FACE_BOUND('',#1153,.T.);
#252=FACE_BOUND('',#1154,.T.);
#253=FACE_BOUND('',#1155,.T.);
#254=FACE_BOUND('',#1166,.T.);
#255=FACE_BOUND('',#1167,.T.);
#256=FACE_BOUND('',#1168,.T.);
#257=FACE_BOUND('',#1169,.T.);
#258=FACE_BOUND('',#1170,.T.);
#259=FACE_BOUND('',#1172,.T.);
#260=FACE_BOUND('',#1173,.T.);
#261=FACE_BOUND('',#1174,.T.);
#262=FACE_BOUND('',#1175,.T.);
#263=FACE_BOUND('',#1176,.T.);
#264=FACE_BOUND('',#1178,.T.);
#265=FACE_BOUND('',#1181,.T.);
#266=FACE_BOUND('',#1185,.T.);
#267=FACE_BOUND('',#1222,.T.);
#268=FACE_BOUND('',#1223,.T.);
#269=FACE_BOUND('',#1232,.T.);
#270=FACE_BOUND('',#1237,.T.);
#271=FACE_BOUND('',#1243,.T.);
#272=FACE_BOUND('',#1245,.T.);
#273=FACE_BOUND('',#1254,.T.);
#274=FACE_BOUND('',#1255,.T.);
#275=FACE_BOUND('',#1256,.T.);
#276=FACE_BOUND('',#1264,.T.);
#277=FACE_BOUND('',#1265,.T.);
#278=FACE_BOUND('',#1267,.T.);
#279=FACE_BOUND('',#1268,.T.);
#280=FACE_BOUND('',#1272,.T.);
#281=FACE_BOUND('',#1275,.T.);
#282=FACE_BOUND('',#1357,.T.);
#283=FACE_BOUND('',#1359,.T.);
#284=FACE_BOUND('',#1389,.T.);
#285=FACE_BOUND('',#1395,.T.);
#286=FACE_BOUND('',#1396,.T.);
#287=FACE_BOUND('',#1404,.T.);
#288=FACE_BOUND('',#1406,.T.);
#289=FACE_BOUND('',#1410,.T.);
#290=FACE_BOUND('',#1412,.T.);
#291=FACE_BOUND('',#1415,.T.);
#292=FACE_BOUND('',#1417,.T.);
#293=FACE_BOUND('',#1420,.T.);
#294=FACE_BOUND('',#1437,.T.);
#295=FACE_BOUND('',#1439,.T.);
#296=FACE_BOUND('',#1485,.T.);
#297=FACE_BOUND('',#1488,.T.);
#298=FACE_BOUND('',#1523,.T.);
#299=FACE_BOUND('',#1526,.T.);
#300=FACE_BOUND('',#1577,.T.);
#301=FACE_BOUND('',#1580,.T.);
#302=PLANE('',#10097);
#303=PLANE('',#10101);
#304=PLANE('',#10105);
#305=PLANE('',#10110);
#306=PLANE('',#10116);
#307=PLANE('',#10122);
#308=PLANE('',#10128);
#309=PLANE('',#10131);
#310=PLANE('',#10134);
#311=PLANE('',#10137);
#312=PLANE('',#10140);
#313=PLANE('',#10141);
#314=PLANE('',#10142);
#315=PLANE('',#10143);
#316=PLANE('',#10150);
#317=PLANE('',#10151);
#318=PLANE('',#10152);
#319=PLANE('',#10153);
#320=PLANE('',#10154);
#321=PLANE('',#10155);
#322=PLANE('',#10156);
#323=PLANE('',#10157);
#324=PLANE('',#10163);
#325=PLANE('',#10164);
#326=PLANE('',#10165);
#327=PLANE('',#10166);
#328=PLANE('',#10167);
#329=PLANE('',#10168);
#330=PLANE('',#10169);
#331=PLANE('',#10170);
#332=PLANE('',#10171);
#333=PLANE('',#10188);
#334=PLANE('',#10189);
#335=PLANE('',#10190);
#336=PLANE('',#10191);
#337=PLANE('',#10192);
#338=PLANE('',#10193);
#339=PLANE('',#10195);
#340=PLANE('',#10200);
#341=PLANE('',#10206);
#342=PLANE('',#10249);
#343=PLANE('',#10260);
#344=PLANE('',#10261);
#345=PLANE('',#10262);
#346=PLANE('',#10263);
#347=PLANE('',#10264);
#348=PLANE('',#10265);
#349=PLANE('',#10266);
#350=PLANE('',#10268);
#351=PLANE('',#10271);
#352=PLANE('',#10272);
#353=PLANE('',#10273);
#354=PLANE('',#10274);
#355=PLANE('',#10275);
#356=PLANE('',#10276);
#357=PLANE('',#10277);
#358=PLANE('',#10278);
#359=PLANE('',#10283);
#360=PLANE('',#10291);
#361=PLANE('',#10292);
#362=PLANE('',#10293);
#363=PLANE('',#10294);
#364=PLANE('',#10295);
#365=PLANE('',#10296);
#366=PLANE('',#10303);
#367=PLANE('',#10307);
#368=PLANE('',#10387);
#369=PLANE('',#10390);
#370=PLANE('',#10391);
#371=PLANE('',#10394);
#372=PLANE('',#10395);
#373=PLANE('',#10396);
#374=PLANE('',#10397);
#375=PLANE('',#10398);
#376=PLANE('',#10399);
#377=PLANE('',#10400);
#378=PLANE('',#10428);
#379=PLANE('',#10431);
#380=PLANE('',#10435);
#381=PLANE('',#10436);
#382=PLANE('',#10437);
#383=PLANE('',#10438);
#384=PLANE('',#10439);
#385=PLANE('',#10440);
#386=PLANE('',#10441);
#387=PLANE('',#10442);
#388=PLANE('',#10447);
#389=PLANE('',#10448);
#390=PLANE('',#10449);
#391=PLANE('',#10450);
#392=PLANE('',#10451);
#393=PLANE('',#10452);
#394=PLANE('',#10460);
#395=PLANE('',#10461);
#396=PLANE('',#10466);
#397=PLANE('',#10468);
#398=PLANE('',#10472);
#399=PLANE('',#10477);
#400=PLANE('',#10479);
#401=PLANE('',#10481);
#402=PLANE('',#10482);
#403=PLANE('',#10483);
#404=PLANE('',#10490);
#405=PLANE('',#10494);
#406=PLANE('',#10495);
#407=PLANE('',#10503);
#408=PLANE('',#10504);
#409=PLANE('',#10546);
#410=PLANE('',#10547);
#411=PLANE('',#10548);
#412=PLANE('',#10549);
#413=PLANE('',#10550);
#414=PLANE('',#10551);
#415=PLANE('',#10552);
#416=PLANE('',#10553);
#417=PLANE('',#10557);
#418=PLANE('',#10558);
#419=PLANE('',#10588);
#420=PLANE('',#10589);
#421=PLANE('',#10590);
#422=PLANE('',#10591);
#423=PLANE('',#10592);
#424=PLANE('',#10593);
#425=PLANE('',#10594);
#426=PLANE('',#10595);
#427=PLANE('',#10599);
#428=PLANE('',#10600);
#429=PLANE('',#10646);
#430=PLANE('',#10647);
#431=PLANE('',#10648);
#432=PLANE('',#10649);
#433=PLANE('',#10650);
#434=PLANE('',#10651);
#435=PLANE('',#10652);
#436=PLANE('',#10653);
#437=PLANE('',#10657);
#438=PLANE('',#10658);
#439=FACE_OUTER_BOUND('',#977,.T.);
#440=FACE_OUTER_BOUND('',#978,.T.);
#441=FACE_OUTER_BOUND('',#979,.T.);
#442=FACE_OUTER_BOUND('',#980,.T.);
#443=FACE_OUTER_BOUND('',#981,.T.);
#444=FACE_OUTER_BOUND('',#982,.T.);
#445=FACE_OUTER_BOUND('',#983,.T.);
#446=FACE_OUTER_BOUND('',#984,.T.);
#447=FACE_OUTER_BOUND('',#985,.T.);
#448=FACE_OUTER_BOUND('',#986,.T.);
#449=FACE_OUTER_BOUND('',#987,.T.);
#450=FACE_OUTER_BOUND('',#988,.T.);
#451=FACE_OUTER_BOUND('',#989,.T.);
#452=FACE_OUTER_BOUND('',#990,.T.);
#453=FACE_OUTER_BOUND('',#991,.T.);
#454=FACE_OUTER_BOUND('',#992,.T.);
#455=FACE_OUTER_BOUND('',#993,.T.);
#456=FACE_OUTER_BOUND('',#994,.T.);
#457=FACE_OUTER_BOUND('',#995,.T.);
#458=FACE_OUTER_BOUND('',#996,.T.);
#459=FACE_OUTER_BOUND('',#997,.T.);
#460=FACE_OUTER_BOUND('',#998,.T.);
#461=FACE_OUTER_BOUND('',#999,.T.);
#462=FACE_OUTER_BOUND('',#1000,.T.);
#463=FACE_OUTER_BOUND('',#1001,.T.);
#464=FACE_OUTER_BOUND('',#1002,.T.);
#465=FACE_OUTER_BOUND('',#1003,.T.);
#466=FACE_OUTER_BOUND('',#1004,.T.);
#467=FACE_OUTER_BOUND('',#1005,.T.);
#468=FACE_OUTER_BOUND('',#1006,.T.);
#469=FACE_OUTER_BOUND('',#1007,.T.);
#470=FACE_OUTER_BOUND('',#1008,.T.);
#471=FACE_OUTER_BOUND('',#1009,.T.);
#472=FACE_OUTER_BOUND('',#1010,.T.);
#473=FACE_OUTER_BOUND('',#1011,.T.);
#474=FACE_OUTER_BOUND('',#1012,.T.);
#475=FACE_OUTER_BOUND('',#1013,.T.);
#476=FACE_OUTER_BOUND('',#1014,.T.);
#477=FACE_OUTER_BOUND('',#1015,.T.);
#478=FACE_OUTER_BOUND('',#1016,.T.);
#479=FACE_OUTER_BOUND('',#1017,.T.);
#480=FACE_OUTER_BOUND('',#1018,.T.);
#481=FACE_OUTER_BOUND('',#1019,.T.);
#482=FACE_OUTER_BOUND('',#1020,.T.);
#483=FACE_OUTER_BOUND('',#1021,.T.);
#484=FACE_OUTER_BOUND('',#1022,.T.);
#485=FACE_OUTER_BOUND('',#1023,.T.);
#486=FACE_OUTER_BOUND('',#1024,.T.);
#487=FACE_OUTER_BOUND('',#1025,.T.);
#488=FACE_OUTER_BOUND('',#1026,.T.);
#489=FACE_OUTER_BOUND('',#1027,.T.);
#490=FACE_OUTER_BOUND('',#1028,.T.);
#491=FACE_OUTER_BOUND('',#1029,.T.);
#492=FACE_OUTER_BOUND('',#1030,.T.);
#493=FACE_OUTER_BOUND('',#1031,.T.);
#494=FACE_OUTER_BOUND('',#1032,.T.);
#495=FACE_OUTER_BOUND('',#1033,.T.);
#496=FACE_OUTER_BOUND('',#1034,.T.);
#497=FACE_OUTER_BOUND('',#1035,.T.);
#498=FACE_OUTER_BOUND('',#1036,.T.);
#499=FACE_OUTER_BOUND('',#1037,.T.);
#500=FACE_OUTER_BOUND('',#1038,.T.);
#501=FACE_OUTER_BOUND('',#1039,.T.);
#502=FACE_OUTER_BOUND('',#1040,.T.);
#503=FACE_OUTER_BOUND('',#1041,.T.);
#504=FACE_OUTER_BOUND('',#1042,.T.);
#505=FACE_OUTER_BOUND('',#1043,.T.);
#506=FACE_OUTER_BOUND('',#1044,.T.);
#507=FACE_OUTER_BOUND('',#1045,.T.);
#508=FACE_OUTER_BOUND('',#1046,.T.);
#509=FACE_OUTER_BOUND('',#1047,.T.);
#510=FACE_OUTER_BOUND('',#1048,.T.);
#511=FACE_OUTER_BOUND('',#1049,.T.);
#512=FACE_OUTER_BOUND('',#1050,.T.);
#513=FACE_OUTER_BOUND('',#1051,.T.);
#514=FACE_OUTER_BOUND('',#1052,.T.);
#515=FACE_OUTER_BOUND('',#1053,.T.);
#516=FACE_OUTER_BOUND('',#1054,.T.);
#517=FACE_OUTER_BOUND('',#1055,.T.);
#518=FACE_OUTER_BOUND('',#1056,.T.);
#519=FACE_OUTER_BOUND('',#1057,.T.);
#520=FACE_OUTER_BOUND('',#1058,.T.);
#521=FACE_OUTER_BOUND('',#1059,.T.);
#522=FACE_OUTER_BOUND('',#1060,.T.);
#523=FACE_OUTER_BOUND('',#1061,.T.);
#524=FACE_OUTER_BOUND('',#1062,.T.);
#525=FACE_OUTER_BOUND('',#1063,.T.);
#526=FACE_OUTER_BOUND('',#1064,.T.);
#527=FACE_OUTER_BOUND('',#1065,.T.);
#528=FACE_OUTER_BOUND('',#1066,.T.);
#529=FACE_OUTER_BOUND('',#1067,.T.);
#530=FACE_OUTER_BOUND('',#1068,.T.);
#531=FACE_OUTER_BOUND('',#1069,.T.);
#532=FACE_OUTER_BOUND('',#1070,.T.);
#533=FACE_OUTER_BOUND('',#1071,.T.);
#534=FACE_OUTER_BOUND('',#1072,.T.);
#535=FACE_OUTER_BOUND('',#1073,.T.);
#536=FACE_OUTER_BOUND('',#1074,.T.);
#537=FACE_OUTER_BOUND('',#1075,.T.);
#538=FACE_OUTER_BOUND('',#1076,.T.);
#539=FACE_OUTER_BOUND('',#1077,.T.);
#540=FACE_OUTER_BOUND('',#1078,.T.);
#541=FACE_OUTER_BOUND('',#1079,.T.);
#542=FACE_OUTER_BOUND('',#1080,.T.);
#543=FACE_OUTER_BOUND('',#1081,.T.);
#544=FACE_OUTER_BOUND('',#1082,.T.);
#545=FACE_OUTER_BOUND('',#1086,.T.);
#546=FACE_OUTER_BOUND('',#1088,.T.);
#547=FACE_OUTER_BOUND('',#1089,.T.);
#548=FACE_OUTER_BOUND('',#1090,.T.);
#549=FACE_OUTER_BOUND('',#1092,.T.);
#550=FACE_OUTER_BOUND('',#1093,.T.);
#551=FACE_OUTER_BOUND('',#1094,.T.);
#552=FACE_OUTER_BOUND('',#1096,.T.);
#553=FACE_OUTER_BOUND('',#1097,.T.);
#554=FACE_OUTER_BOUND('',#1098,.T.);
#555=FACE_OUTER_BOUND('',#1099,.T.);
#556=FACE_OUTER_BOUND('',#1100,.T.);
#557=FACE_OUTER_BOUND('',#1101,.T.);
#558=FACE_OUTER_BOUND('',#1102,.T.);
#559=FACE_OUTER_BOUND('',#1103,.T.);
#560=FACE_OUTER_BOUND('',#1104,.T.);
#561=FACE_OUTER_BOUND('',#1105,.T.);
#562=FACE_OUTER_BOUND('',#1106,.T.);
#563=FACE_OUTER_BOUND('',#1107,.T.);
#564=FACE_OUTER_BOUND('',#1108,.T.);
#565=FACE_OUTER_BOUND('',#1109,.T.);
#566=FACE_OUTER_BOUND('',#1110,.T.);
#567=FACE_OUTER_BOUND('',#1111,.T.);
#568=FACE_OUTER_BOUND('',#1112,.T.);
#569=FACE_OUTER_BOUND('',#1113,.T.);
#570=FACE_OUTER_BOUND('',#1114,.T.);
#571=FACE_OUTER_BOUND('',#1115,.T.);
#572=FACE_OUTER_BOUND('',#1116,.T.);
#573=FACE_OUTER_BOUND('',#1117,.T.);
#574=FACE_OUTER_BOUND('',#1118,.T.);
#575=FACE_OUTER_BOUND('',#1119,.T.);
#576=FACE_OUTER_BOUND('',#1120,.T.);
#577=FACE_OUTER_BOUND('',#1121,.T.);
#578=FACE_OUTER_BOUND('',#1122,.T.);
#579=FACE_OUTER_BOUND('',#1123,.T.);
#580=FACE_OUTER_BOUND('',#1124,.T.);
#581=FACE_OUTER_BOUND('',#1125,.T.);
#582=FACE_OUTER_BOUND('',#1126,.T.);
#583=FACE_OUTER_BOUND('',#1127,.T.);
#584=FACE_OUTER_BOUND('',#1129,.T.);
#585=FACE_OUTER_BOUND('',#1130,.T.);
#586=FACE_OUTER_BOUND('',#1131,.T.);
#587=FACE_OUTER_BOUND('',#1132,.T.);
#588=FACE_OUTER_BOUND('',#1134,.T.);
#589=FACE_OUTER_BOUND('',#1135,.T.);
#590=FACE_OUTER_BOUND('',#1136,.T.);
#591=FACE_OUTER_BOUND('',#1138,.T.);
#592=FACE_OUTER_BOUND('',#1139,.T.);
#593=FACE_OUTER_BOUND('',#1140,.T.);
#594=FACE_OUTER_BOUND('',#1141,.T.);
#595=FACE_OUTER_BOUND('',#1142,.T.);
#596=FACE_OUTER_BOUND('',#1144,.T.);
#597=FACE_OUTER_BOUND('',#1145,.T.);
#598=FACE_OUTER_BOUND('',#1151,.T.);
#599=FACE_OUTER_BOUND('',#1156,.T.);
#600=FACE_OUTER_BOUND('',#1157,.T.);
#601=FACE_OUTER_BOUND('',#1158,.T.);
#602=FACE_OUTER_BOUND('',#1159,.T.);
#603=FACE_OUTER_BOUND('',#1160,.T.);
#604=FACE_OUTER_BOUND('',#1161,.T.);
#605=FACE_OUTER_BOUND('',#1162,.T.);
#606=FACE_OUTER_BOUND('',#1163,.T.);
#607=FACE_OUTER_BOUND('',#1164,.T.);
#608=FACE_OUTER_BOUND('',#1165,.T.);
#609=FACE_OUTER_BOUND('',#1171,.T.);
#610=FACE_OUTER_BOUND('',#1177,.T.);
#611=FACE_OUTER_BOUND('',#1179,.T.);
#612=FACE_OUTER_BOUND('',#1180,.T.);
#613=FACE_OUTER_BOUND('',#1182,.T.);
#614=FACE_OUTER_BOUND('',#1183,.T.);
#615=FACE_OUTER_BOUND('',#1184,.T.);
#616=FACE_OUTER_BOUND('',#1186,.T.);
#617=FACE_OUTER_BOUND('',#1187,.T.);
#618=FACE_OUTER_BOUND('',#1188,.T.);
#619=FACE_OUTER_BOUND('',#1189,.T.);
#620=FACE_OUTER_BOUND('',#1190,.T.);
#621=FACE_OUTER_BOUND('',#1191,.T.);
#622=FACE_OUTER_BOUND('',#1192,.T.);
#623=FACE_OUTER_BOUND('',#1193,.T.);
#624=FACE_OUTER_BOUND('',#1194,.T.);
#625=FACE_OUTER_BOUND('',#1195,.T.);
#626=FACE_OUTER_BOUND('',#1196,.T.);
#627=FACE_OUTER_BOUND('',#1197,.T.);
#628=FACE_OUTER_BOUND('',#1198,.T.);
#629=FACE_OUTER_BOUND('',#1199,.T.);
#630=FACE_OUTER_BOUND('',#1200,.T.);
#631=FACE_OUTER_BOUND('',#1201,.T.);
#632=FACE_OUTER_BOUND('',#1202,.T.);
#633=FACE_OUTER_BOUND('',#1203,.T.);
#634=FACE_OUTER_BOUND('',#1204,.T.);
#635=FACE_OUTER_BOUND('',#1205,.T.);
#636=FACE_OUTER_BOUND('',#1206,.T.);
#637=FACE_OUTER_BOUND('',#1207,.T.);
#638=FACE_OUTER_BOUND('',#1208,.T.);
#639=FACE_OUTER_BOUND('',#1209,.T.);
#640=FACE_OUTER_BOUND('',#1210,.T.);
#641=FACE_OUTER_BOUND('',#1211,.T.);
#642=FACE_OUTER_BOUND('',#1212,.T.);
#643=FACE_OUTER_BOUND('',#1213,.T.);
#644=FACE_OUTER_BOUND('',#1214,.T.);
#645=FACE_OUTER_BOUND('',#1215,.T.);
#646=FACE_OUTER_BOUND('',#1216,.T.);
#647=FACE_OUTER_BOUND('',#1217,.T.);
#648=FACE_OUTER_BOUND('',#1218,.T.);
#649=FACE_OUTER_BOUND('',#1219,.T.);
#650=FACE_OUTER_BOUND('',#1220,.T.);
#651=FACE_OUTER_BOUND('',#1221,.T.);
#652=FACE_OUTER_BOUND('',#1224,.T.);
#653=FACE_OUTER_BOUND('',#1225,.T.);
#654=FACE_OUTER_BOUND('',#1226,.T.);
#655=FACE_OUTER_BOUND('',#1227,.T.);
#656=FACE_OUTER_BOUND('',#1228,.T.);
#657=FACE_OUTER_BOUND('',#1229,.T.);
#658=FACE_OUTER_BOUND('',#1230,.T.);
#659=FACE_OUTER_BOUND('',#1231,.T.);
#660=FACE_OUTER_BOUND('',#1233,.T.);
#661=FACE_OUTER_BOUND('',#1234,.T.);
#662=FACE_OUTER_BOUND('',#1235,.T.);
#663=FACE_OUTER_BOUND('',#1236,.T.);
#664=FACE_OUTER_BOUND('',#1238,.T.);
#665=FACE_OUTER_BOUND('',#1239,.T.);
#666=FACE_OUTER_BOUND('',#1240,.T.);
#667=FACE_OUTER_BOUND('',#1241,.T.);
#668=FACE_OUTER_BOUND('',#1242,.T.);
#669=FACE_OUTER_BOUND('',#1244,.T.);
#670=FACE_OUTER_BOUND('',#1246,.T.);
#671=FACE_OUTER_BOUND('',#1247,.T.);
#672=FACE_OUTER_BOUND('',#1248,.T.);
#673=FACE_OUTER_BOUND('',#1249,.T.);
#674=FACE_OUTER_BOUND('',#1250,.T.);
#675=FACE_OUTER_BOUND('',#1251,.T.);
#676=FACE_OUTER_BOUND('',#1252,.T.);
#677=FACE_OUTER_BOUND('',#1253,.T.);
#678=FACE_OUTER_BOUND('',#1257,.T.);
#679=FACE_OUTER_BOUND('',#1258,.T.);
#680=FACE_OUTER_BOUND('',#1259,.T.);
#681=FACE_OUTER_BOUND('',#1260,.T.);
#682=FACE_OUTER_BOUND('',#1261,.T.);
#683=FACE_OUTER_BOUND('',#1262,.T.);
#684=FACE_OUTER_BOUND('',#1263,.T.);
#685=FACE_OUTER_BOUND('',#1266,.T.);
#686=FACE_OUTER_BOUND('',#1269,.T.);
#687=FACE_OUTER_BOUND('',#1270,.T.);
#688=FACE_OUTER_BOUND('',#1271,.T.);
#689=FACE_OUTER_BOUND('',#1273,.T.);
#690=FACE_OUTER_BOUND('',#1274,.T.);
#691=FACE_OUTER_BOUND('',#1276,.T.);
#692=FACE_OUTER_BOUND('',#1277,.T.);
#693=FACE_OUTER_BOUND('',#1278,.T.);
#694=FACE_OUTER_BOUND('',#1279,.T.);
#695=FACE_OUTER_BOUND('',#1280,.T.);
#696=FACE_OUTER_BOUND('',#1281,.T.);
#697=FACE_OUTER_BOUND('',#1282,.T.);
#698=FACE_OUTER_BOUND('',#1283,.T.);
#699=FACE_OUTER_BOUND('',#1284,.T.);
#700=FACE_OUTER_BOUND('',#1285,.T.);
#701=FACE_OUTER_BOUND('',#1286,.T.);
#702=FACE_OUTER_BOUND('',#1287,.T.);
#703=FACE_OUTER_BOUND('',#1288,.T.);
#704=FACE_OUTER_BOUND('',#1289,.T.);
#705=FACE_OUTER_BOUND('',#1290,.T.);
#706=FACE_OUTER_BOUND('',#1291,.T.);
#707=FACE_OUTER_BOUND('',#1292,.T.);
#708=FACE_OUTER_BOUND('',#1293,.T.);
#709=FACE_OUTER_BOUND('',#1294,.T.);
#710=FACE_OUTER_BOUND('',#1295,.T.);
#711=FACE_OUTER_BOUND('',#1296,.T.);
#712=FACE_OUTER_BOUND('',#1297,.T.);
#713=FACE_OUTER_BOUND('',#1298,.T.);
#714=FACE_OUTER_BOUND('',#1299,.T.);
#715=FACE_OUTER_BOUND('',#1300,.T.);
#716=FACE_OUTER_BOUND('',#1301,.T.);
#717=FACE_OUTER_BOUND('',#1302,.T.);
#718=FACE_OUTER_BOUND('',#1303,.T.);
#719=FACE_OUTER_BOUND('',#1304,.T.);
#720=FACE_OUTER_BOUND('',#1305,.T.);
#721=FACE_OUTER_BOUND('',#1306,.T.);
#722=FACE_OUTER_BOUND('',#1307,.T.);
#723=FACE_OUTER_BOUND('',#1308,.T.);
#724=FACE_OUTER_BOUND('',#1309,.T.);
#725=FACE_OUTER_BOUND('',#1310,.T.);
#726=FACE_OUTER_BOUND('',#1311,.T.);
#727=FACE_OUTER_BOUND('',#1312,.T.);
#728=FACE_OUTER_BOUND('',#1313,.T.);
#729=FACE_OUTER_BOUND('',#1314,.T.);
#730=FACE_OUTER_BOUND('',#1315,.T.);
#731=FACE_OUTER_BOUND('',#1316,.T.);
#732=FACE_OUTER_BOUND('',#1317,.T.);
#733=FACE_OUTER_BOUND('',#1318,.T.);
#734=FACE_OUTER_BOUND('',#1319,.T.);
#735=FACE_OUTER_BOUND('',#1320,.T.);
#736=FACE_OUTER_BOUND('',#1321,.T.);
#737=FACE_OUTER_BOUND('',#1322,.T.);
#738=FACE_OUTER_BOUND('',#1323,.T.);
#739=FACE_OUTER_BOUND('',#1324,.T.);
#740=FACE_OUTER_BOUND('',#1325,.T.);
#741=FACE_OUTER_BOUND('',#1326,.T.);
#742=FACE_OUTER_BOUND('',#1327,.T.);
#743=FACE_OUTER_BOUND('',#1328,.T.);
#744=FACE_OUTER_BOUND('',#1329,.T.);
#745=FACE_OUTER_BOUND('',#1330,.T.);
#746=FACE_OUTER_BOUND('',#1331,.T.);
#747=FACE_OUTER_BOUND('',#1332,.T.);
#748=FACE_OUTER_BOUND('',#1333,.T.);
#749=FACE_OUTER_BOUND('',#1334,.T.);
#750=FACE_OUTER_BOUND('',#1335,.T.);
#751=FACE_OUTER_BOUND('',#1336,.T.);
#752=FACE_OUTER_BOUND('',#1337,.T.);
#753=FACE_OUTER_BOUND('',#1338,.T.);
#754=FACE_OUTER_BOUND('',#1339,.T.);
#755=FACE_OUTER_BOUND('',#1340,.T.);
#756=FACE_OUTER_BOUND('',#1341,.T.);
#757=FACE_OUTER_BOUND('',#1342,.T.);
#758=FACE_OUTER_BOUND('',#1343,.T.);
#759=FACE_OUTER_BOUND('',#1344,.T.);
#760=FACE_OUTER_BOUND('',#1345,.T.);
#761=FACE_OUTER_BOUND('',#1346,.T.);
#762=FACE_OUTER_BOUND('',#1347,.T.);
#763=FACE_OUTER_BOUND('',#1348,.T.);
#764=FACE_OUTER_BOUND('',#1349,.T.);
#765=FACE_OUTER_BOUND('',#1350,.T.);
#766=FACE_OUTER_BOUND('',#1351,.T.);
#767=FACE_OUTER_BOUND('',#1352,.T.);
#768=FACE_OUTER_BOUND('',#1353,.T.);
#769=FACE_OUTER_BOUND('',#1354,.T.);
#770=FACE_OUTER_BOUND('',#1355,.T.);
#771=FACE_OUTER_BOUND('',#1356,.T.);
#772=FACE_OUTER_BOUND('',#1358,.T.);
#773=FACE_OUTER_BOUND('',#1360,.T.);
#774=FACE_OUTER_BOUND('',#1361,.T.);
#775=FACE_OUTER_BOUND('',#1362,.T.);
#776=FACE_OUTER_BOUND('',#1363,.T.);
#777=FACE_OUTER_BOUND('',#1364,.T.);
#778=FACE_OUTER_BOUND('',#1365,.T.);
#779=FACE_OUTER_BOUND('',#1366,.T.);
#780=FACE_OUTER_BOUND('',#1367,.T.);
#781=FACE_OUTER_BOUND('',#1368,.T.);
#782=FACE_OUTER_BOUND('',#1369,.T.);
#783=FACE_OUTER_BOUND('',#1370,.T.);
#784=FACE_OUTER_BOUND('',#1371,.T.);
#785=FACE_OUTER_BOUND('',#1372,.T.);
#786=FACE_OUTER_BOUND('',#1373,.T.);
#787=FACE_OUTER_BOUND('',#1374,.T.);
#788=FACE_OUTER_BOUND('',#1375,.T.);
#789=FACE_OUTER_BOUND('',#1376,.T.);
#790=FACE_OUTER_BOUND('',#1377,.T.);
#791=FACE_OUTER_BOUND('',#1378,.T.);
#792=FACE_OUTER_BOUND('',#1379,.T.);
#793=FACE_OUTER_BOUND('',#1380,.T.);
#794=FACE_OUTER_BOUND('',#1381,.T.);
#795=FACE_OUTER_BOUND('',#1382,.T.);
#796=FACE_OUTER_BOUND('',#1383,.T.);
#797=FACE_OUTER_BOUND('',#1384,.T.);
#798=FACE_OUTER_BOUND('',#1385,.T.);
#799=FACE_OUTER_BOUND('',#1386,.T.);
#800=FACE_OUTER_BOUND('',#1387,.T.);
#801=FACE_OUTER_BOUND('',#1388,.T.);
#802=FACE_OUTER_BOUND('',#1390,.T.);
#803=FACE_OUTER_BOUND('',#1391,.T.);
#804=FACE_OUTER_BOUND('',#1392,.T.);
#805=FACE_OUTER_BOUND('',#1393,.T.);
#806=FACE_OUTER_BOUND('',#1394,.T.);
#807=FACE_OUTER_BOUND('',#1397,.T.);
#808=FACE_OUTER_BOUND('',#1398,.T.);
#809=FACE_OUTER_BOUND('',#1399,.T.);
#810=FACE_OUTER_BOUND('',#1400,.T.);
#811=FACE_OUTER_BOUND('',#1401,.T.);
#812=FACE_OUTER_BOUND('',#1402,.T.);
#813=FACE_OUTER_BOUND('',#1403,.T.);
#814=FACE_OUTER_BOUND('',#1405,.T.);
#815=FACE_OUTER_BOUND('',#1407,.T.);
#816=FACE_OUTER_BOUND('',#1408,.T.);
#817=FACE_OUTER_BOUND('',#1409,.T.);
#818=FACE_OUTER_BOUND('',#1411,.T.);
#819=FACE_OUTER_BOUND('',#1413,.T.);
#820=FACE_OUTER_BOUND('',#1414,.T.);
#821=FACE_OUTER_BOUND('',#1416,.T.);
#822=FACE_OUTER_BOUND('',#1418,.T.);
#823=FACE_OUTER_BOUND('',#1419,.T.);
#824=FACE_OUTER_BOUND('',#1421,.T.);
#825=FACE_OUTER_BOUND('',#1422,.T.);
#826=FACE_OUTER_BOUND('',#1423,.T.);
#827=FACE_OUTER_BOUND('',#1424,.T.);
#828=FACE_OUTER_BOUND('',#1425,.T.);
#829=FACE_OUTER_BOUND('',#1426,.T.);
#830=FACE_OUTER_BOUND('',#1427,.T.);
#831=FACE_OUTER_BOUND('',#1428,.T.);
#832=FACE_OUTER_BOUND('',#1429,.T.);
#833=FACE_OUTER_BOUND('',#1430,.T.);
#834=FACE_OUTER_BOUND('',#1431,.T.);
#835=FACE_OUTER_BOUND('',#1432,.T.);
#836=FACE_OUTER_BOUND('',#1433,.T.);
#837=FACE_OUTER_BOUND('',#1434,.T.);
#838=FACE_OUTER_BOUND('',#1435,.T.);
#839=FACE_OUTER_BOUND('',#1436,.T.);
#840=FACE_OUTER_BOUND('',#1438,.T.);
#841=FACE_OUTER_BOUND('',#1440,.T.);
#842=FACE_OUTER_BOUND('',#1441,.T.);
#843=FACE_OUTER_BOUND('',#1442,.T.);
#844=FACE_OUTER_BOUND('',#1443,.T.);
#845=FACE_OUTER_BOUND('',#1444,.T.);
#846=FACE_OUTER_BOUND('',#1445,.T.);
#847=FACE_OUTER_BOUND('',#1446,.T.);
#848=FACE_OUTER_BOUND('',#1447,.T.);
#849=FACE_OUTER_BOUND('',#1448,.T.);
#850=FACE_OUTER_BOUND('',#1449,.T.);
#851=FACE_OUTER_BOUND('',#1450,.T.);
#852=FACE_OUTER_BOUND('',#1451,.T.);
#853=FACE_OUTER_BOUND('',#1452,.T.);
#854=FACE_OUTER_BOUND('',#1453,.T.);
#855=FACE_OUTER_BOUND('',#1454,.T.);
#856=FACE_OUTER_BOUND('',#1455,.T.);
#857=FACE_OUTER_BOUND('',#1456,.T.);
#858=FACE_OUTER_BOUND('',#1457,.T.);
#859=FACE_OUTER_BOUND('',#1458,.T.);
#860=FACE_OUTER_BOUND('',#1459,.T.);
#861=FACE_OUTER_BOUND('',#1460,.T.);
#862=FACE_OUTER_BOUND('',#1461,.T.);
#863=FACE_OUTER_BOUND('',#1462,.T.);
#864=FACE_OUTER_BOUND('',#1463,.T.);
#865=FACE_OUTER_BOUND('',#1464,.T.);
#866=FACE_OUTER_BOUND('',#1465,.T.);
#867=FACE_OUTER_BOUND('',#1466,.T.);
#868=FACE_OUTER_BOUND('',#1467,.T.);
#869=FACE_OUTER_BOUND('',#1468,.T.);
#870=FACE_OUTER_BOUND('',#1469,.T.);
#871=FACE_OUTER_BOUND('',#1470,.T.);
#872=FACE_OUTER_BOUND('',#1471,.T.);
#873=FACE_OUTER_BOUND('',#1472,.T.);
#874=FACE_OUTER_BOUND('',#1473,.T.);
#875=FACE_OUTER_BOUND('',#1474,.T.);
#876=FACE_OUTER_BOUND('',#1475,.T.);
#877=FACE_OUTER_BOUND('',#1476,.T.);
#878=FACE_OUTER_BOUND('',#1477,.T.);
#879=FACE_OUTER_BOUND('',#1478,.T.);
#880=FACE_OUTER_BOUND('',#1479,.T.);
#881=FACE_OUTER_BOUND('',#1480,.T.);
#882=FACE_OUTER_BOUND('',#1481,.T.);
#883=FACE_OUTER_BOUND('',#1482,.T.);
#884=FACE_OUTER_BOUND('',#1483,.T.);
#885=FACE_OUTER_BOUND('',#1484,.T.);
#886=FACE_OUTER_BOUND('',#1486,.T.);
#887=FACE_OUTER_BOUND('',#1487,.T.);
#888=FACE_OUTER_BOUND('',#1489,.T.);
#889=FACE_OUTER_BOUND('',#1490,.T.);
#890=FACE_OUTER_BOUND('',#1491,.T.);
#891=FACE_OUTER_BOUND('',#1492,.T.);
#892=FACE_OUTER_BOUND('',#1493,.T.);
#893=FACE_OUTER_BOUND('',#1494,.T.);
#894=FACE_OUTER_BOUND('',#1495,.T.);
#895=FACE_OUTER_BOUND('',#1496,.T.);
#896=FACE_OUTER_BOUND('',#1497,.T.);
#897=FACE_OUTER_BOUND('',#1498,.T.);
#898=FACE_OUTER_BOUND('',#1499,.T.);
#899=FACE_OUTER_BOUND('',#1500,.T.);
#900=FACE_OUTER_BOUND('',#1501,.T.);
#901=FACE_OUTER_BOUND('',#1502,.T.);
#902=FACE_OUTER_BOUND('',#1503,.T.);
#903=FACE_OUTER_BOUND('',#1504,.T.);
#904=FACE_OUTER_BOUND('',#1505,.T.);
#905=FACE_OUTER_BOUND('',#1506,.T.);
#906=FACE_OUTER_BOUND('',#1507,.T.);
#907=FACE_OUTER_BOUND('',#1508,.T.);
#908=FACE_OUTER_BOUND('',#1509,.T.);
#909=FACE_OUTER_BOUND('',#1510,.T.);
#910=FACE_OUTER_BOUND('',#1511,.T.);
#911=FACE_OUTER_BOUND('',#1512,.T.);
#912=FACE_OUTER_BOUND('',#1513,.T.);
#913=FACE_OUTER_BOUND('',#1514,.T.);
#914=FACE_OUTER_BOUND('',#1515,.T.);
#915=FACE_OUTER_BOUND('',#1516,.T.);
#916=FACE_OUTER_BOUND('',#1517,.T.);
#917=FACE_OUTER_BOUND('',#1518,.T.);
#918=FACE_OUTER_BOUND('',#1519,.T.);
#919=FACE_OUTER_BOUND('',#1520,.T.);
#920=FACE_OUTER_BOUND('',#1521,.T.);
#921=FACE_OUTER_BOUND('',#1522,.T.);
#922=FACE_OUTER_BOUND('',#1524,.T.);
#923=FACE_OUTER_BOUND('',#1525,.T.);
#924=FACE_OUTER_BOUND('',#1527,.T.);
#925=FACE_OUTER_BOUND('',#1528,.T.);
#926=FACE_OUTER_BOUND('',#1529,.T.);
#927=FACE_OUTER_BOUND('',#1530,.T.);
#928=FACE_OUTER_BOUND('',#1531,.T.);
#929=FACE_OUTER_BOUND('',#1532,.T.);
#930=FACE_OUTER_BOUND('',#1533,.T.);
#931=FACE_OUTER_BOUND('',#1534,.T.);
#932=FACE_OUTER_BOUND('',#1535,.T.);
#933=FACE_OUTER_BOUND('',#1536,.T.);
#934=FACE_OUTER_BOUND('',#1537,.T.);
#935=FACE_OUTER_BOUND('',#1538,.T.);
#936=FACE_OUTER_BOUND('',#1539,.T.);
#937=FACE_OUTER_BOUND('',#1540,.T.);
#938=FACE_OUTER_BOUND('',#1541,.T.);
#939=FACE_OUTER_BOUND('',#1542,.T.);
#940=FACE_OUTER_BOUND('',#1543,.T.);
#941=FACE_OUTER_BOUND('',#1544,.T.);
#942=FACE_OUTER_BOUND('',#1545,.T.);
#943=FACE_OUTER_BOUND('',#1546,.T.);
#944=FACE_OUTER_BOUND('',#1547,.T.);
#945=FACE_OUTER_BOUND('',#1548,.T.);
#946=FACE_OUTER_BOUND('',#1549,.T.);
#947=FACE_OUTER_BOUND('',#1550,.T.);
#948=FACE_OUTER_BOUND('',#1551,.T.);
#949=FACE_OUTER_BOUND('',#1552,.T.);
#950=FACE_OUTER_BOUND('',#1553,.T.);
#951=FACE_OUTER_BOUND('',#1554,.T.);
#952=FACE_OUTER_BOUND('',#1555,.T.);
#953=FACE_OUTER_BOUND('',#1556,.T.);
#954=FACE_OUTER_BOUND('',#1557,.T.);
#955=FACE_OUTER_BOUND('',#1558,.T.);
#956=FACE_OUTER_BOUND('',#1559,.T.);
#957=FACE_OUTER_BOUND('',#1560,.T.);
#958=FACE_OUTER_BOUND('',#1561,.T.);
#959=FACE_OUTER_BOUND('',#1562,.T.);
#960=FACE_OUTER_BOUND('',#1563,.T.);
#961=FACE_OUTER_BOUND('',#1564,.T.);
#962=FACE_OUTER_BOUND('',#1565,.T.);
#963=FACE_OUTER_BOUND('',#1566,.T.);
#964=FACE_OUTER_BOUND('',#1567,.T.);
#965=FACE_OUTER_BOUND('',#1568,.T.);
#966=FACE_OUTER_BOUND('',#1569,.T.);
#967=FACE_OUTER_BOUND('',#1570,.T.);
#968=FACE_OUTER_BOUND('',#1571,.T.);
#969=FACE_OUTER_BOUND('',#1572,.T.);
#970=FACE_OUTER_BOUND('',#1573,.T.);
#971=FACE_OUTER_BOUND('',#1574,.T.);
#972=FACE_OUTER_BOUND('',#1575,.T.);
#973=FACE_OUTER_BOUND('',#1576,.T.);
#974=FACE_OUTER_BOUND('',#1578,.T.);
#975=FACE_OUTER_BOUND('',#1579,.T.);
#976=FACE_OUTER_BOUND('',#1581,.T.);
#977=EDGE_LOOP('',(#5986,#5987,#5988,#5989,#5990,#5991,#5992,#5993));
#978=EDGE_LOOP('',(#5994,#5995,#5996,#5997));
#979=EDGE_LOOP('',(#5998,#5999,#6000,#6001));
#980=EDGE_LOOP('',(#6002,#6003,#6004,#6005));
#981=EDGE_LOOP('',(#6006,#6007,#6008,#6009));
#982=EDGE_LOOP('',(#6010,#6011,#6012,#6013));
#983=EDGE_LOOP('',(#6014,#6015,#6016,#6017));
#984=EDGE_LOOP('',(#6018,#6019,#6020,#6021));
#985=EDGE_LOOP('',(#6022,#6023,#6024,#6025));
#986=EDGE_LOOP('',(#6026,#6027,#6028,#6029));
#987=EDGE_LOOP('',(#6030,#6031,#6032,#6033));
#988=EDGE_LOOP('',(#6034,#6035,#6036,#6037));
#989=EDGE_LOOP('',(#6038,#6039,#6040,#6041));
#990=EDGE_LOOP('',(#6042,#6043,#6044,#6045));
#991=EDGE_LOOP('',(#6046,#6047,#6048,#6049));
#992=EDGE_LOOP('',(#6050,#6051,#6052,#6053));
#993=EDGE_LOOP('',(#6054,#6055,#6056,#6057));
#994=EDGE_LOOP('',(#6058,#6059,#6060,#6061));
#995=EDGE_LOOP('',(#6062,#6063,#6064,#6065));
#996=EDGE_LOOP('',(#6066,#6067,#6068,#6069));
#997=EDGE_LOOP('',(#6070,#6071,#6072,#6073));
#998=EDGE_LOOP('',(#6074,#6075,#6076,#6077));
#999=EDGE_LOOP('',(#6078,#6079,#6080,#6081));
#1000=EDGE_LOOP('',(#6082,#6083,#6084,#6085));
#1001=EDGE_LOOP('',(#6086,#6087,#6088,#6089));
#1002=EDGE_LOOP('',(#6090,#6091,#6092,#6093,#6094,#6095,#6096,#6097));
#1003=EDGE_LOOP('',(#6098,#6099,#6100,#6101));
#1004=EDGE_LOOP('',(#6102,#6103,#6104,#6105));
#1005=EDGE_LOOP('',(#6106,#6107,#6108,#6109));
#1006=EDGE_LOOP('',(#6110,#6111,#6112,#6113));
#1007=EDGE_LOOP('',(#6114,#6115,#6116,#6117));
#1008=EDGE_LOOP('',(#6118,#6119,#6120,#6121));
#1009=EDGE_LOOP('',(#6122,#6123,#6124,#6125));
#1010=EDGE_LOOP('',(#6126,#6127,#6128,#6129));
#1011=EDGE_LOOP('',(#6130,#6131,#6132,#6133));
#1012=EDGE_LOOP('',(#6134,#6135,#6136,#6137));
#1013=EDGE_LOOP('',(#6138,#6139,#6140,#6141));
#1014=EDGE_LOOP('',(#6142,#6143,#6144,#6145));
#1015=EDGE_LOOP('',(#6146,#6147,#6148,#6149));
#1016=EDGE_LOOP('',(#6150,#6151,#6152,#6153));
#1017=EDGE_LOOP('',(#6154,#6155,#6156,#6157));
#1018=EDGE_LOOP('',(#6158,#6159,#6160,#6161));
#1019=EDGE_LOOP('',(#6162,#6163,#6164,#6165));
#1020=EDGE_LOOP('',(#6166,#6167,#6168,#6169));
#1021=EDGE_LOOP('',(#6170,#6171,#6172,#6173));
#1022=EDGE_LOOP('',(#6174,#6175,#6176,#6177));
#1023=EDGE_LOOP('',(#6178,#6179,#6180,#6181));
#1024=EDGE_LOOP('',(#6182,#6183,#6184,#6185));
#1025=EDGE_LOOP('',(#6186,#6187,#6188,#6189));
#1026=EDGE_LOOP('',(#6190,#6191,#6192,#6193));
#1027=EDGE_LOOP('',(#6194,#6195,#6196,#6197,#6198,#6199,#6200,#6201));
#1028=EDGE_LOOP('',(#6202,#6203,#6204,#6205));
#1029=EDGE_LOOP('',(#6206,#6207,#6208,#6209));
#1030=EDGE_LOOP('',(#6210,#6211,#6212,#6213));
#1031=EDGE_LOOP('',(#6214,#6215,#6216,#6217));
#1032=EDGE_LOOP('',(#6218,#6219,#6220,#6221));
#1033=EDGE_LOOP('',(#6222,#6223,#6224,#6225));
#1034=EDGE_LOOP('',(#6226,#6227,#6228,#6229));
#1035=EDGE_LOOP('',(#6230,#6231,#6232,#6233));
#1036=EDGE_LOOP('',(#6234,#6235,#6236,#6237));
#1037=EDGE_LOOP('',(#6238,#6239,#6240,#6241));
#1038=EDGE_LOOP('',(#6242,#6243,#6244,#6245));
#1039=EDGE_LOOP('',(#6246,#6247,#6248,#6249));
#1040=EDGE_LOOP('',(#6250,#6251,#6252,#6253));
#1041=EDGE_LOOP('',(#6254,#6255,#6256,#6257));
#1042=EDGE_LOOP('',(#6258,#6259,#6260,#6261));
#1043=EDGE_LOOP('',(#6262,#6263,#6264,#6265));
#1044=EDGE_LOOP('',(#6266,#6267,#6268,#6269));
#1045=EDGE_LOOP('',(#6270,#6271,#6272,#6273));
#1046=EDGE_LOOP('',(#6274,#6275,#6276,#6277));
#1047=EDGE_LOOP('',(#6278,#6279,#6280,#6281));
#1048=EDGE_LOOP('',(#6282,#6283,#6284,#6285));
#1049=EDGE_LOOP('',(#6286,#6287,#6288,#6289));
#1050=EDGE_LOOP('',(#6290,#6291,#6292,#6293));
#1051=EDGE_LOOP('',(#6294,#6295,#6296,#6297));
#1052=EDGE_LOOP('',(#6298,#6299,#6300,#6301,#6302,#6303,#6304,#6305));
#1053=EDGE_LOOP('',(#6306,#6307,#6308,#6309));
#1054=EDGE_LOOP('',(#6310,#6311,#6312,#6313));
#1055=EDGE_LOOP('',(#6314,#6315,#6316,#6317));
#1056=EDGE_LOOP('',(#6318,#6319,#6320,#6321));
#1057=EDGE_LOOP('',(#6322,#6323,#6324,#6325));
#1058=EDGE_LOOP('',(#6326,#6327,#6328,#6329));
#1059=EDGE_LOOP('',(#6330,#6331,#6332,#6333));
#1060=EDGE_LOOP('',(#6334,#6335,#6336,#6337));
#1061=EDGE_LOOP('',(#6338,#6339,#6340,#6341));
#1062=EDGE_LOOP('',(#6342,#6343,#6344,#6345));
#1063=EDGE_LOOP('',(#6346,#6347,#6348,#6349));
#1064=EDGE_LOOP('',(#6350,#6351,#6352,#6353));
#1065=EDGE_LOOP('',(#6354,#6355,#6356,#6357));
#1066=EDGE_LOOP('',(#6358,#6359,#6360,#6361));
#1067=EDGE_LOOP('',(#6362,#6363,#6364,#6365));
#1068=EDGE_LOOP('',(#6366,#6367,#6368,#6369));
#1069=EDGE_LOOP('',(#6370,#6371,#6372,#6373));
#1070=EDGE_LOOP('',(#6374,#6375,#6376,#6377));
#1071=EDGE_LOOP('',(#6378,#6379,#6380,#6381));
#1072=EDGE_LOOP('',(#6382,#6383,#6384,#6385));
#1073=EDGE_LOOP('',(#6386,#6387,#6388,#6389));
#1074=EDGE_LOOP('',(#6390,#6391,#6392,#6393));
#1075=EDGE_LOOP('',(#6394,#6395,#6396,#6397));
#1076=EDGE_LOOP('',(#6398,#6399,#6400,#6401));
#1077=EDGE_LOOP('',(#6402,#6403,#6404,#6405));
#1078=EDGE_LOOP('',(#6406,#6407,#6408,#6409));
#1079=EDGE_LOOP('',(#6410,#6411,#6412,#6413));
#1080=EDGE_LOOP('',(#6414,#6415,#6416,#6417));
#1081=EDGE_LOOP('',(#6418,#6419,#6420,#6421));
#1082=EDGE_LOOP('',(#6422,#6423,#6424,#6425,#6426,#6427,#6428,#6429));
#1083=EDGE_LOOP('',(#6430));
#1084=EDGE_LOOP('',(#6431));
#1085=EDGE_LOOP('',(#6432));
#1086=EDGE_LOOP('',(#6433,#6434,#6435,#6436));
#1087=EDGE_LOOP('',(#6437));
#1088=EDGE_LOOP('',(#6438,#6439,#6440,#6441));
#1089=EDGE_LOOP('',(#6442,#6443,#6444,#6445));
#1090=EDGE_LOOP('',(#6446));
#1091=EDGE_LOOP('',(#6447));
#1092=EDGE_LOOP('',(#6448,#6449,#6450,#6451));
#1093=EDGE_LOOP('',(#6452,#6453,#6454,#6455));
#1094=EDGE_LOOP('',(#6456));
#1095=EDGE_LOOP('',(#6457));
#1096=EDGE_LOOP('',(#6458,#6459,#6460,#6461));
#1097=EDGE_LOOP('',(#6462,#6463,#6464,#6465));
#1098=EDGE_LOOP('',(#6466,#6467,#6468,#6469));
#1099=EDGE_LOOP('',(#6470,#6471,#6472,#6473));
#1100=EDGE_LOOP('',(#6474,#6475,#6476,#6477,#6478,#6479,#6480,#6481,#6482,
#6483,#6484,#6485,#6486,#6487,#6488,#6489,#6490,#6491,#6492,#6493,#6494,
#6495,#6496,#6497,#6498,#6499,#6500,#6501,#6502,#6503));
#1101=EDGE_LOOP('',(#6504,#6505,#6506,#6507,#6508,#6509,#6510,#6511,#6512,
#6513,#6514,#6515,#6516,#6517,#6518,#6519,#6520,#6521,#6522,#6523,#6524,
#6525,#6526,#6527,#6528,#6529,#6530,#6531,#6532));
#1102=EDGE_LOOP('',(#6533,#6534,#6535,#6536));
#1103=EDGE_LOOP('',(#6537,#6538,#6539,#6540));
#1104=EDGE_LOOP('',(#6541,#6542,#6543,#6544));
#1105=EDGE_LOOP('',(#6545,#6546,#6547,#6548,#6549,#6550,#6551,#6552,#6553,
#6554,#6555,#6556,#6557,#6558,#6559,#6560,#6561,#6562,#6563,#6564,#6565,
#6566,#6567,#6568,#6569,#6570,#6571,#6572,#6573,#6574));
#1106=EDGE_LOOP('',(#6575,#6576,#6577,#6578,#6579,#6580,#6581,#6582,#6583,
#6584,#6585,#6586,#6587,#6588,#6589,#6590,#6591,#6592,#6593,#6594,#6595,
#6596,#6597,#6598,#6599,#6600,#6601,#6602,#6603));
#1107=EDGE_LOOP('',(#6604,#6605,#6606,#6607));
#1108=EDGE_LOOP('',(#6608,#6609,#6610,#6611));
#1109=EDGE_LOOP('',(#6612,#6613,#6614,#6615));
#1110=EDGE_LOOP('',(#6616,#6617,#6618,#6619,#6620,#6621,#6622,#6623,#6624,
#6625,#6626,#6627,#6628,#6629,#6630,#6631,#6632,#6633,#6634,#6635,#6636,
#6637,#6638,#6639,#6640,#6641,#6642,#6643,#6644,#6645));
#1111=EDGE_LOOP('',(#6646,#6647,#6648,#6649,#6650,#6651,#6652,#6653,#6654,
#6655,#6656,#6657,#6658,#6659,#6660,#6661,#6662,#6663,#6664,#6665,#6666,
#6667,#6668,#6669,#6670,#6671,#6672,#6673,#6674));
#1112=EDGE_LOOP('',(#6675,#6676,#6677,#6678));
#1113=EDGE_LOOP('',(#6679,#6680,#6681,#6682));
#1114=EDGE_LOOP('',(#6683,#6684,#6685,#6686));
#1115=EDGE_LOOP('',(#6687,#6688,#6689,#6690,#6691,#6692,#6693,#6694,#6695,
#6696,#6697,#6698,#6699,#6700,#6701,#6702,#6703,#6704,#6705,#6706,#6707,
#6708,#6709,#6710,#6711,#6712,#6713,#6714,#6715,#6716));
#1116=EDGE_LOOP('',(#6717,#6718,#6719,#6720,#6721,#6722,#6723,#6724,#6725,
#6726,#6727,#6728,#6729,#6730,#6731,#6732,#6733,#6734,#6735,#6736,#6737,
#6738,#6739,#6740,#6741,#6742,#6743,#6744,#6745));
#1117=EDGE_LOOP('',(#6746,#6747,#6748,#6749));
#1118=EDGE_LOOP('',(#6750));
#1119=EDGE_LOOP('',(#6751));
#1120=EDGE_LOOP('',(#6752));
#1121=EDGE_LOOP('',(#6753));
#1122=EDGE_LOOP('',(#6754,#6755,#6756,#6757));
#1123=EDGE_LOOP('',(#6758,#6759,#6760,#6761));
#1124=EDGE_LOOP('',(#6762,#6763,#6764,#6765));
#1125=EDGE_LOOP('',(#6766,#6767,#6768,#6769));
#1126=EDGE_LOOP('',(#6770,#6771,#6772,#6773));
#1127=EDGE_LOOP('',(#6774,#6775,#6776,#6777));
#1128=EDGE_LOOP('',(#6778));
#1129=EDGE_LOOP('',(#6779,#6780,#6781,#6782));
#1130=EDGE_LOOP('',(#6783,#6784,#6785,#6786));
#1131=EDGE_LOOP('',(#6787,#6788,#6789,#6790));
#1132=EDGE_LOOP('',(#6791,#6792,#6793,#6794));
#1133=EDGE_LOOP('',(#6795));
#1134=EDGE_LOOP('',(#6796,#6797,#6798,#6799));
#1135=EDGE_LOOP('',(#6800,#6801,#6802,#6803));
#1136=EDGE_LOOP('',(#6804));
#1137=EDGE_LOOP('',(#6805));
#1138=EDGE_LOOP('',(#6806,#6807,#6808,#6809));
#1139=EDGE_LOOP('',(#6810));
#1140=EDGE_LOOP('',(#6811,#6812,#6813,#6814));
#1141=EDGE_LOOP('',(#6815,#6816,#6817,#6818,#6819,#6820,#6821,#6822));
#1142=EDGE_LOOP('',(#6823,#6824,#6825,#6826));
#1143=EDGE_LOOP('',(#6827));
#1144=EDGE_LOOP('',(#6828,#6829,#6830,#6831,#6832,#6833,#6834,#6835));
#1145=EDGE_LOOP('',(#6836,#6837,#6838,#6839));
#1146=EDGE_LOOP('',(#6840,#6841,#6842,#6843));
#1147=EDGE_LOOP('',(#6844,#6845,#6846,#6847));
#1148=EDGE_LOOP('',(#6848,#6849,#6850,#6851));
#1149=EDGE_LOOP('',(#6852,#6853,#6854,#6855));
#1150=EDGE_LOOP('',(#6856,#6857,#6858,#6859,#6860,#6861,#6862,#6863));
#1151=EDGE_LOOP('',(#6864,#6865,#6866,#6867,#6868,#6869,#6870,#6871,#6872,
#6873,#6874,#6875));
#1152=EDGE_LOOP('',(#6876));
#1153=EDGE_LOOP('',(#6877));
#1154=EDGE_LOOP('',(#6878));
#1155=EDGE_LOOP('',(#6879));
#1156=EDGE_LOOP('',(#6880,#6881,#6882,#6883));
#1157=EDGE_LOOP('',(#6884,#6885,#6886,#6887));
#1158=EDGE_LOOP('',(#6888,#6889,#6890,#6891));
#1159=EDGE_LOOP('',(#6892,#6893,#6894,#6895));
#1160=EDGE_LOOP('',(#6896,#6897,#6898,#6899));
#1161=EDGE_LOOP('',(#6900,#6901,#6902,#6903));
#1162=EDGE_LOOP('',(#6904,#6905,#6906,#6907));
#1163=EDGE_LOOP('',(#6908,#6909,#6910,#6911));
#1164=EDGE_LOOP('',(#6912,#6913,#6914,#6915));
#1165=EDGE_LOOP('',(#6916,#6917,#6918,#6919));
#1166=EDGE_LOOP('',(#6920));
#1167=EDGE_LOOP('',(#6921));
#1168=EDGE_LOOP('',(#6922));
#1169=EDGE_LOOP('',(#6923));
#1170=EDGE_LOOP('',(#6924));
#1171=EDGE_LOOP('',(#6925,#6926,#6927,#6928));
#1172=EDGE_LOOP('',(#6929));
#1173=EDGE_LOOP('',(#6930));
#1174=EDGE_LOOP('',(#6931));
#1175=EDGE_LOOP('',(#6932));
#1176=EDGE_LOOP('',(#6933));
#1177=EDGE_LOOP('',(#6934));
#1178=EDGE_LOOP('',(#6935));
#1179=EDGE_LOOP('',(#6936,#6937,#6938,#6939));
#1180=EDGE_LOOP('',(#6940));
#1181=EDGE_LOOP('',(#6941));
#1182=EDGE_LOOP('',(#6942,#6943,#6944,#6945));
#1183=EDGE_LOOP('',(#6946,#6947,#6948,#6949));
#1184=EDGE_LOOP('',(#6950));
#1185=EDGE_LOOP('',(#6951));
#1186=EDGE_LOOP('',(#6952,#6953,#6954,#6955));
#1187=EDGE_LOOP('',(#6956,#6957,#6958,#6959));
#1188=EDGE_LOOP('',(#6960,#6961,#6962,#6963));
#1189=EDGE_LOOP('',(#6964,#6965,#6966,#6967));
#1190=EDGE_LOOP('',(#6968,#6969,#6970,#6971));
#1191=EDGE_LOOP('',(#6972,#6973,#6974,#6975));
#1192=EDGE_LOOP('',(#6976,#6977,#6978,#6979));
#1193=EDGE_LOOP('',(#6980,#6981,#6982,#6983));
#1194=EDGE_LOOP('',(#6984,#6985,#6986,#6987));
#1195=EDGE_LOOP('',(#6988,#6989,#6990,#6991));
#1196=EDGE_LOOP('',(#6992,#6993,#6994,#6995));
#1197=EDGE_LOOP('',(#6996,#6997,#6998,#6999));
#1198=EDGE_LOOP('',(#7000,#7001,#7002,#7003));
#1199=EDGE_LOOP('',(#7004,#7005,#7006,#7007));
#1200=EDGE_LOOP('',(#7008,#7009,#7010,#7011));
#1201=EDGE_LOOP('',(#7012,#7013,#7014,#7015));
#1202=EDGE_LOOP('',(#7016,#7017,#7018,#7019));
#1203=EDGE_LOOP('',(#7020,#7021,#7022,#7023));
#1204=EDGE_LOOP('',(#7024,#7025,#7026,#7027));
#1205=EDGE_LOOP('',(#7028,#7029,#7030,#7031));
#1206=EDGE_LOOP('',(#7032,#7033,#7034,#7035));
#1207=EDGE_LOOP('',(#7036,#7037,#7038,#7039));
#1208=EDGE_LOOP('',(#7040,#7041,#7042,#7043));
#1209=EDGE_LOOP('',(#7044,#7045,#7046,#7047));
#1210=EDGE_LOOP('',(#7048,#7049,#7050,#7051));
#1211=EDGE_LOOP('',(#7052,#7053,#7054,#7055));
#1212=EDGE_LOOP('',(#7056,#7057,#7058,#7059));
#1213=EDGE_LOOP('',(#7060,#7061,#7062,#7063));
#1214=EDGE_LOOP('',(#7064,#7065,#7066,#7067));
#1215=EDGE_LOOP('',(#7068,#7069,#7070,#7071));
#1216=EDGE_LOOP('',(#7072,#7073,#7074,#7075));
#1217=EDGE_LOOP('',(#7076,#7077,#7078,#7079));
#1218=EDGE_LOOP('',(#7080,#7081,#7082,#7083));
#1219=EDGE_LOOP('',(#7084,#7085,#7086,#7087,#7088,#7089,#7090,#7091,#7092,
#7093,#7094,#7095,#7096,#7097,#7098,#7099,#7100,#7101,#7102,#7103));
#1220=EDGE_LOOP('',(#7104,#7105,#7106,#7107,#7108,#7109,#7110,#7111,#7112,
#7113,#7114,#7115,#7116,#7117,#7118,#7119,#7120,#7121,#7122,#7123));
#1221=EDGE_LOOP('',(#7124,#7125,#7126,#7127,#7128,#7129));
#1222=EDGE_LOOP('',(#7130,#7131,#7132,#7133));
#1223=EDGE_LOOP('',(#7134,#7135,#7136,#7137));
#1224=EDGE_LOOP('',(#7138,#7139,#7140,#7141));
#1225=EDGE_LOOP('',(#7142,#7143,#7144,#7145,#7146,#7147,#7148,#7149,#7150,
#7151,#7152,#7153,#7154,#7155,#7156,#7157,#7158,#7159,#7160,#7161));
#1226=EDGE_LOOP('',(#7162,#7163,#7164,#7165,#7166,#7167,#7168,#7169,#7170,
#7171,#7172,#7173,#7174,#7175,#7176,#7177,#7178,#7179,#7180,#7181));
#1227=EDGE_LOOP('',(#7182,#7183,#7184,#7185));
#1228=EDGE_LOOP('',(#7186,#7187,#7188,#7189));
#1229=EDGE_LOOP('',(#7190,#7191,#7192,#7193));
#1230=EDGE_LOOP('',(#7194,#7195,#7196,#7197));
#1231=EDGE_LOOP('',(#7198,#7199,#7200,#7201));
#1232=EDGE_LOOP('',(#7202));
#1233=EDGE_LOOP('',(#7203,#7204,#7205,#7206));
#1234=EDGE_LOOP('',(#7207,#7208,#7209,#7210,#7211,#7212,#7213,#7214,#7215));
#1235=EDGE_LOOP('',(#7216,#7217,#7218,#7219));
#1236=EDGE_LOOP('',(#7220,#7221,#7222,#7223));
#1237=EDGE_LOOP('',(#7224));
#1238=EDGE_LOOP('',(#7225,#7226,#7227,#7228));
#1239=EDGE_LOOP('',(#7229,#7230,#7231,#7232));
#1240=EDGE_LOOP('',(#7233,#7234,#7235,#7236,#7237));
#1241=EDGE_LOOP('',(#7238,#7239,#7240,#7241,#7242,#7243,#7244,#7245,#7246));
#1242=EDGE_LOOP('',(#7247,#7248,#7249,#7250));
#1243=EDGE_LOOP('',(#7251));
#1244=EDGE_LOOP('',(#7252,#7253,#7254,#7255));
#1245=EDGE_LOOP('',(#7256));
#1246=EDGE_LOOP('',(#7257,#7258,#7259,#7260));
#1247=EDGE_LOOP('',(#7261,#7262,#7263,#7264));
#1248=EDGE_LOOP('',(#7265,#7266,#7267,#7268));
#1249=EDGE_LOOP('',(#7269,#7270,#7271,#7272));
#1250=EDGE_LOOP('',(#7273,#7274,#7275,#7276));
#1251=EDGE_LOOP('',(#7277,#7278,#7279,#7280));
#1252=EDGE_LOOP('',(#7281,#7282,#7283,#7284,#7285,#7286));
#1253=EDGE_LOOP('',(#7287,#7288,#7289,#7290,#7291,#7292));
#1254=EDGE_LOOP('',(#7293,#7294,#7295,#7296));
#1255=EDGE_LOOP('',(#7297,#7298,#7299,#7300));
#1256=EDGE_LOOP('',(#7301));
#1257=EDGE_LOOP('',(#7302,#7303,#7304,#7305));
#1258=EDGE_LOOP('',(#7306,#7307,#7308,#7309));
#1259=EDGE_LOOP('',(#7310,#7311,#7312,#7313));
#1260=EDGE_LOOP('',(#7314,#7315,#7316,#7317));
#1261=EDGE_LOOP('',(#7318,#7319,#7320,#7321));
#1262=EDGE_LOOP('',(#7322,#7323,#7324,#7325));
#1263=EDGE_LOOP('',(#7326,#7327,#7328,#7329));
#1264=EDGE_LOOP('',(#7330));
#1265=EDGE_LOOP('',(#7331));
#1266=EDGE_LOOP('',(#7332,#7333,#7334,#7335));
#1267=EDGE_LOOP('',(#7336));
#1268=EDGE_LOOP('',(#7337));
#1269=EDGE_LOOP('',(#7338,#7339,#7340,#7341));
#1270=EDGE_LOOP('',(#7342,#7343,#7344,#7345));
#1271=EDGE_LOOP('',(#7346));
#1272=EDGE_LOOP('',(#7347));
#1273=EDGE_LOOP('',(#7348,#7349,#7350,#7351));
#1274=EDGE_LOOP('',(#7352));
#1275=EDGE_LOOP('',(#7353));
#1276=EDGE_LOOP('',(#7354,#7355,#7356,#7357));
#1277=EDGE_LOOP('',(#7358,#7359,#7360,#7361));
#1278=EDGE_LOOP('',(#7362,#7363,#7364,#7365));
#1279=EDGE_LOOP('',(#7366,#7367,#7368,#7369,#7370,#7371,#7372,#7373));
#1280=EDGE_LOOP('',(#7374,#7375,#7376,#7377));
#1281=EDGE_LOOP('',(#7378,#7379,#7380,#7381));
#1282=EDGE_LOOP('',(#7382,#7383,#7384,#7385));
#1283=EDGE_LOOP('',(#7386,#7387,#7388,#7389));
#1284=EDGE_LOOP('',(#7390,#7391,#7392,#7393));
#1285=EDGE_LOOP('',(#7394,#7395,#7396,#7397));
#1286=EDGE_LOOP('',(#7398,#7399,#7400,#7401));
#1287=EDGE_LOOP('',(#7402,#7403,#7404,#7405));
#1288=EDGE_LOOP('',(#7406,#7407,#7408,#7409));
#1289=EDGE_LOOP('',(#7410,#7411,#7412,#7413));
#1290=EDGE_LOOP('',(#7414,#7415,#7416,#7417));
#1291=EDGE_LOOP('',(#7418,#7419,#7420,#7421));
#1292=EDGE_LOOP('',(#7422,#7423,#7424,#7425));
#1293=EDGE_LOOP('',(#7426,#7427,#7428,#7429));
#1294=EDGE_LOOP('',(#7430,#7431,#7432,#7433));
#1295=EDGE_LOOP('',(#7434,#7435,#7436,#7437));
#1296=EDGE_LOOP('',(#7438,#7439,#7440,#7441));
#1297=EDGE_LOOP('',(#7442,#7443,#7444,#7445));
#1298=EDGE_LOOP('',(#7446,#7447,#7448,#7449));
#1299=EDGE_LOOP('',(#7450,#7451,#7452,#7453));
#1300=EDGE_LOOP('',(#7454,#7455,#7456,#7457));
#1301=EDGE_LOOP('',(#7458,#7459,#7460,#7461));
#1302=EDGE_LOOP('',(#7462,#7463,#7464,#7465));
#1303=EDGE_LOOP('',(#7466,#7467,#7468,#7469));
#1304=EDGE_LOOP('',(#7470,#7471,#7472,#7473,#7474,#7475,#7476,#7477));
#1305=EDGE_LOOP('',(#7478,#7479,#7480,#7481));
#1306=EDGE_LOOP('',(#7482,#7483,#7484,#7485));
#1307=EDGE_LOOP('',(#7486,#7487,#7488,#7489));
#1308=EDGE_LOOP('',(#7490,#7491,#7492,#7493));
#1309=EDGE_LOOP('',(#7494,#7495,#7496,#7497));
#1310=EDGE_LOOP('',(#7498,#7499,#7500,#7501));
#1311=EDGE_LOOP('',(#7502,#7503,#7504,#7505));
#1312=EDGE_LOOP('',(#7506,#7507,#7508,#7509));
#1313=EDGE_LOOP('',(#7510,#7511,#7512,#7513));
#1314=EDGE_LOOP('',(#7514,#7515,#7516,#7517));
#1315=EDGE_LOOP('',(#7518,#7519,#7520,#7521));
#1316=EDGE_LOOP('',(#7522,#7523,#7524,#7525));
#1317=EDGE_LOOP('',(#7526,#7527,#7528,#7529));
#1318=EDGE_LOOP('',(#7530,#7531,#7532,#7533));
#1319=EDGE_LOOP('',(#7534,#7535,#7536,#7537));
#1320=EDGE_LOOP('',(#7538,#7539,#7540,#7541));
#1321=EDGE_LOOP('',(#7542,#7543,#7544,#7545));
#1322=EDGE_LOOP('',(#7546,#7547,#7548,#7549));
#1323=EDGE_LOOP('',(#7550,#7551,#7552,#7553));
#1324=EDGE_LOOP('',(#7554,#7555,#7556,#7557));
#1325=EDGE_LOOP('',(#7558,#7559,#7560,#7561));
#1326=EDGE_LOOP('',(#7562,#7563,#7564,#7565));
#1327=EDGE_LOOP('',(#7566,#7567,#7568,#7569));
#1328=EDGE_LOOP('',(#7570,#7571,#7572,#7573));
#1329=EDGE_LOOP('',(#7574,#7575,#7576,#7577));
#1330=EDGE_LOOP('',(#7578,#7579,#7580,#7581));
#1331=EDGE_LOOP('',(#7582,#7583,#7584,#7585));
#1332=EDGE_LOOP('',(#7586,#7587,#7588,#7589));
#1333=EDGE_LOOP('',(#7590,#7591,#7592,#7593));
#1334=EDGE_LOOP('',(#7594,#7595,#7596,#7597));
#1335=EDGE_LOOP('',(#7598,#7599,#7600,#7601));
#1336=EDGE_LOOP('',(#7602,#7603,#7604,#7605));
#1337=EDGE_LOOP('',(#7606,#7607,#7608,#7609));
#1338=EDGE_LOOP('',(#7610,#7611,#7612,#7613));
#1339=EDGE_LOOP('',(#7614,#7615,#7616,#7617));
#1340=EDGE_LOOP('',(#7618,#7619,#7620,#7621,#7622));
#1341=EDGE_LOOP('',(#7623,#7624,#7625,#7626));
#1342=EDGE_LOOP('',(#7627,#7628,#7629,#7630,#7631,#7632,#7633,#7634,#7635,
#7636,#7637,#7638,#7639,#7640,#7641,#7642,#7643,#7644,#7645,#7646,#7647,
#7648,#7649,#7650,#7651,#7652,#7653,#7654,#7655,#7656,#7657,#7658,#7659,
#7660,#7661,#7662,#7663,#7664,#7665,#7666));
#1343=EDGE_LOOP('',(#7667,#7668,#7669,#7670,#7671,#7672,#7673,#7674,#7675,
#7676,#7677,#7678,#7679,#7680,#7681,#7682,#7683,#7684,#7685,#7686,#7687,
#7688,#7689,#7690,#7691,#7692,#7693,#7694,#7695,#7696,#7697,#7698,#7699,
#7700,#7701,#7702,#7703,#7704,#7705,#7706));
#1344=EDGE_LOOP('',(#7707,#7708,#7709,#7710));
#1345=EDGE_LOOP('',(#7711));
#1346=EDGE_LOOP('',(#7712,#7713,#7714,#7715));
#1347=EDGE_LOOP('',(#7716,#7717,#7718,#7719));
#1348=EDGE_LOOP('',(#7720,#7721,#7722,#7723,#7724,#7725,#7726,#7727,#7728,
#7729,#7730,#7731,#7732,#7733,#7734,#7735,#7736,#7737,#7738,#7739,#7740,
#7741,#7742,#7743,#7744,#7745,#7746,#7747,#7748,#7749));
#1349=EDGE_LOOP('',(#7750,#7751,#7752,#7753,#7754,#7755,#7756,#7757,#7758,
#7759,#7760,#7761,#7762,#7763,#7764,#7765,#7766,#7767,#7768,#7769,#7770,
#7771,#7772,#7773,#7774,#7775,#7776,#7777,#7778));
#1350=EDGE_LOOP('',(#7779,#7780,#7781,#7782));
#1351=EDGE_LOOP('',(#7783));
#1352=EDGE_LOOP('',(#7784,#7785,#7786,#7787));
#1353=EDGE_LOOP('',(#7788,#7789,#7790,#7791));
#1354=EDGE_LOOP('',(#7792,#7793,#7794,#7795));
#1355=EDGE_LOOP('',(#7796,#7797,#7798,#7799));
#1356=EDGE_LOOP('',(#7800,#7801,#7802,#7803));
#1357=EDGE_LOOP('',(#7804,#7805,#7806,#7807));
#1358=EDGE_LOOP('',(#7808,#7809,#7810,#7811));
#1359=EDGE_LOOP('',(#7812,#7813,#7814,#7815));
#1360=EDGE_LOOP('',(#7816,#7817,#7818,#7819,#7820,#7821,#7822,#7823));
#1361=EDGE_LOOP('',(#7824,#7825,#7826,#7827));
#1362=EDGE_LOOP('',(#7828,#7829,#7830,#7831));
#1363=EDGE_LOOP('',(#7832,#7833,#7834,#7835));
#1364=EDGE_LOOP('',(#7836,#7837,#7838,#7839));
#1365=EDGE_LOOP('',(#7840,#7841,#7842,#7843));
#1366=EDGE_LOOP('',(#7844,#7845,#7846,#7847));
#1367=EDGE_LOOP('',(#7848,#7849,#7850,#7851));
#1368=EDGE_LOOP('',(#7852,#7853,#7854,#7855));
#1369=EDGE_LOOP('',(#7856,#7857,#7858,#7859));
#1370=EDGE_LOOP('',(#7860,#7861,#7862,#7863));
#1371=EDGE_LOOP('',(#7864,#7865,#7866,#7867));
#1372=EDGE_LOOP('',(#7868,#7869,#7870,#7871));
#1373=EDGE_LOOP('',(#7872,#7873,#7874,#7875));
#1374=EDGE_LOOP('',(#7876,#7877,#7878,#7879));
#1375=EDGE_LOOP('',(#7880,#7881,#7882,#7883));
#1376=EDGE_LOOP('',(#7884,#7885,#7886,#7887));
#1377=EDGE_LOOP('',(#7888,#7889,#7890,#7891));
#1378=EDGE_LOOP('',(#7892,#7893,#7894,#7895));
#1379=EDGE_LOOP('',(#7896,#7897,#7898,#7899));
#1380=EDGE_LOOP('',(#7900,#7901,#7902,#7903,#7904));
#1381=EDGE_LOOP('',(#7905,#7906,#7907,#7908));
#1382=EDGE_LOOP('',(#7909,#7910,#7911,#7912,#7913,#7914,#7915,#7916,#7917,
#7918,#7919,#7920,#7921,#7922,#7923,#7924,#7925,#7926,#7927,#7928,#7929,
#7930,#7931,#7932));
#1383=EDGE_LOOP('',(#7933,#7934,#7935,#7936,#7937,#7938,#7939,#7940,#7941,
#7942,#7943,#7944,#7945,#7946,#7947,#7948,#7949,#7950,#7951,#7952,#7953,
#7954,#7955,#7956));
#1384=EDGE_LOOP('',(#7957,#7958,#7959,#7960));
#1385=EDGE_LOOP('',(#7961));
#1386=EDGE_LOOP('',(#7962,#7963,#7964,#7965));
#1387=EDGE_LOOP('',(#7966,#7967,#7968,#7969));
#1388=EDGE_LOOP('',(#7970,#7971,#7972,#7973));
#1389=EDGE_LOOP('',(#7974));
#1390=EDGE_LOOP('',(#7975,#7976,#7977,#7978,#7979,#7980));
#1391=EDGE_LOOP('',(#7981,#7982,#7983,#7984));
#1392=EDGE_LOOP('',(#7985,#7986,#7987,#7988,#7989,#7990));
#1393=EDGE_LOOP('',(#7991,#7992,#7993,#7994));
#1394=EDGE_LOOP('',(#7995,#7996,#7997,#7998));
#1395=EDGE_LOOP('',(#7999,#8000,#8001,#8002));
#1396=EDGE_LOOP('',(#8003));
#1397=EDGE_LOOP('',(#8004,#8005,#8006,#8007));
#1398=EDGE_LOOP('',(#8008,#8009,#8010,#8011));
#1399=EDGE_LOOP('',(#8012,#8013,#8014,#8015));
#1400=EDGE_LOOP('',(#8016,#8017,#8018,#8019));
#1401=EDGE_LOOP('',(#8020,#8021,#8022,#8023));
#1402=EDGE_LOOP('',(#8024,#8025,#8026,#8027));
#1403=EDGE_LOOP('',(#8028,#8029,#8030,#8031));
#1404=EDGE_LOOP('',(#8032));
#1405=EDGE_LOOP('',(#8033,#8034,#8035,#8036));
#1406=EDGE_LOOP('',(#8037));
#1407=EDGE_LOOP('',(#8038,#8039,#8040,#8041));
#1408=EDGE_LOOP('',(#8042,#8043,#8044,#8045));
#1409=EDGE_LOOP('',(#8046));
#1410=EDGE_LOOP('',(#8047));
#1411=EDGE_LOOP('',(#8048));
#1412=EDGE_LOOP('',(#8049));
#1413=EDGE_LOOP('',(#8050,#8051,#8052,#8053));
#1414=EDGE_LOOP('',(#8054));
#1415=EDGE_LOOP('',(#8055));
#1416=EDGE_LOOP('',(#8056));
#1417=EDGE_LOOP('',(#8057));
#1418=EDGE_LOOP('',(#8058,#8059,#8060,#8061));
#1419=EDGE_LOOP('',(#8062));
#1420=EDGE_LOOP('',(#8063));
#1421=EDGE_LOOP('',(#8064,#8065,#8066,#8067));
#1422=EDGE_LOOP('',(#8068));
#1423=EDGE_LOOP('',(#8069,#8070,#8071,#8072));
#1424=EDGE_LOOP('',(#8073));
#1425=EDGE_LOOP('',(#8074,#8075,#8076,#8077));
#1426=EDGE_LOOP('',(#8078,#8079,#8080,#8081));
#1427=EDGE_LOOP('',(#8082,#8083,#8084,#8085));
#1428=EDGE_LOOP('',(#8086,#8087,#8088,#8089));
#1429=EDGE_LOOP('',(#8090,#8091,#8092,#8093));
#1430=EDGE_LOOP('',(#8094,#8095,#8096,#8097));
#1431=EDGE_LOOP('',(#8098,#8099,#8100,#8101));
#1432=EDGE_LOOP('',(#8102));
#1433=EDGE_LOOP('',(#8103));
#1434=EDGE_LOOP('',(#8104,#8105,#8106,#8107));
#1435=EDGE_LOOP('',(#8108,#8109,#8110,#8111));
#1436=EDGE_LOOP('',(#8112));
#1437=EDGE_LOOP('',(#8113));
#1438=EDGE_LOOP('',(#8114));
#1439=EDGE_LOOP('',(#8115));
#1440=EDGE_LOOP('',(#8116,#8117,#8118,#8119));
#1441=EDGE_LOOP('',(#8120,#8121,#8122,#8123));
#1442=EDGE_LOOP('',(#8124,#8125,#8126,#8127));
#1443=EDGE_LOOP('',(#8128,#8129,#8130,#8131));
#1444=EDGE_LOOP('',(#8132,#8133,#8134,#8135));
#1445=EDGE_LOOP('',(#8136,#8137,#8138,#8139));
#1446=EDGE_LOOP('',(#8140,#8141,#8142,#8143));
#1447=EDGE_LOOP('',(#8144,#8145,#8146,#8147));
#1448=EDGE_LOOP('',(#8148,#8149,#8150,#8151));
#1449=EDGE_LOOP('',(#8152,#8153,#8154,#8155));
#1450=EDGE_LOOP('',(#8156,#8157,#8158,#8159));
#1451=EDGE_LOOP('',(#8160,#8161,#8162,#8163));
#1452=EDGE_LOOP('',(#8164,#8165,#8166,#8167));
#1453=EDGE_LOOP('',(#8168,#8169,#8170,#8171));
#1454=EDGE_LOOP('',(#8172,#8173,#8174,#8175));
#1455=EDGE_LOOP('',(#8176,#8177,#8178,#8179));
#1456=EDGE_LOOP('',(#8180,#8181,#8182,#8183));
#1457=EDGE_LOOP('',(#8184,#8185,#8186,#8187));
#1458=EDGE_LOOP('',(#8188,#8189,#8190,#8191));
#1459=EDGE_LOOP('',(#8192,#8193,#8194,#8195));
#1460=EDGE_LOOP('',(#8196,#8197,#8198,#8199));
#1461=EDGE_LOOP('',(#8200,#8201,#8202,#8203));
#1462=EDGE_LOOP('',(#8204,#8205,#8206,#8207));
#1463=EDGE_LOOP('',(#8208,#8209,#8210,#8211));
#1464=EDGE_LOOP('',(#8212,#8213,#8214,#8215));
#1465=EDGE_LOOP('',(#8216,#8217,#8218,#8219));
#1466=EDGE_LOOP('',(#8220,#8221,#8222,#8223));
#1467=EDGE_LOOP('',(#8224,#8225,#8226,#8227));
#1468=EDGE_LOOP('',(#8228,#8229,#8230,#8231));
#1469=EDGE_LOOP('',(#8232,#8233,#8234,#8235));
#1470=EDGE_LOOP('',(#8236,#8237,#8238,#8239));
#1471=EDGE_LOOP('',(#8240,#8241,#8242,#8243));
#1472=EDGE_LOOP('',(#8244,#8245,#8246,#8247,#8248,#8249,#8250,#8251));
#1473=EDGE_LOOP('',(#8252,#8253,#8254,#8255,#8256,#8257,#8258,#8259,#8260,
#8261,#8262,#8263,#8264,#8265,#8266,#8267,#8268,#8269,#8270,#8271,#8272,
#8273,#8274,#8275,#8276,#8277,#8278,#8279,#8280,#8281,#8282,#8283,#8284,
#8285,#8286,#8287));
#1474=EDGE_LOOP('',(#8288,#8289,#8290,#8291));
#1475=EDGE_LOOP('',(#8292,#8293,#8294,#8295,#8296,#8297,#8298,#8299,#8300,
#8301,#8302,#8303,#8304,#8305,#8306,#8307,#8308,#8309,#8310,#8311,#8312,
#8313,#8314,#8315,#8316,#8317,#8318,#8319,#8320,#8321,#8322,#8323,#8324,
#8325,#8326,#8327,#8328));
#1476=EDGE_LOOP('',(#8329,#8330,#8331,#8332));
#1477=EDGE_LOOP('',(#8333,#8334,#8335,#8336));
#1478=EDGE_LOOP('',(#8337,#8338,#8339,#8340));
#1479=EDGE_LOOP('',(#8341,#8342,#8343,#8344));
#1480=EDGE_LOOP('',(#8345,#8346,#8347,#8348));
#1481=EDGE_LOOP('',(#8349,#8350,#8351,#8352));
#1482=EDGE_LOOP('',(#8353,#8354,#8355,#8356));
#1483=EDGE_LOOP('',(#8357,#8358,#8359,#8360,#8361,#8362));
#1484=EDGE_LOOP('',(#8363));
#1485=EDGE_LOOP('',(#8364,#8365,#8366,#8367));
#1486=EDGE_LOOP('',(#8368,#8369,#8370,#8371));
#1487=EDGE_LOOP('',(#8372));
#1488=EDGE_LOOP('',(#8373,#8374,#8375,#8376,#8377,#8378));
#1489=EDGE_LOOP('',(#8379));
#1490=EDGE_LOOP('',(#8380,#8381,#8382,#8383));
#1491=EDGE_LOOP('',(#8384,#8385,#8386,#8387));
#1492=EDGE_LOOP('',(#8388,#8389,#8390,#8391));
#1493=EDGE_LOOP('',(#8392,#8393,#8394,#8395));
#1494=EDGE_LOOP('',(#8396,#8397,#8398,#8399));
#1495=EDGE_LOOP('',(#8400,#8401,#8402,#8403));
#1496=EDGE_LOOP('',(#8404,#8405,#8406,#8407));
#1497=EDGE_LOOP('',(#8408,#8409,#8410,#8411));
#1498=EDGE_LOOP('',(#8412,#8413,#8414,#8415));
#1499=EDGE_LOOP('',(#8416,#8417,#8418,#8419));
#1500=EDGE_LOOP('',(#8420,#8421,#8422,#8423));
#1501=EDGE_LOOP('',(#8424,#8425,#8426,#8427));
#1502=EDGE_LOOP('',(#8428,#8429,#8430,#8431));
#1503=EDGE_LOOP('',(#8432,#8433,#8434,#8435));
#1504=EDGE_LOOP('',(#8436,#8437,#8438,#8439));
#1505=EDGE_LOOP('',(#8440,#8441,#8442,#8443));
#1506=EDGE_LOOP('',(#8444,#8445,#8446,#8447));
#1507=EDGE_LOOP('',(#8448,#8449,#8450,#8451));
#1508=EDGE_LOOP('',(#8452,#8453,#8454,#8455));
#1509=EDGE_LOOP('',(#8456,#8457,#8458,#8459));
#1510=EDGE_LOOP('',(#8460,#8461,#8462,#8463,#8464,#8465,#8466,#8467));
#1511=EDGE_LOOP('',(#8468,#8469,#8470,#8471,#8472,#8473,#8474,#8475,#8476,
#8477,#8478,#8479,#8480,#8481,#8482,#8483,#8484,#8485,#8486,#8487,#8488,
#8489,#8490,#8491));
#1512=EDGE_LOOP('',(#8492,#8493,#8494,#8495));
#1513=EDGE_LOOP('',(#8496,#8497,#8498,#8499,#8500,#8501,#8502,#8503,#8504,
#8505,#8506,#8507,#8508,#8509,#8510,#8511,#8512,#8513,#8514,#8515,#8516,
#8517,#8518,#8519,#8520));
#1514=EDGE_LOOP('',(#8521,#8522,#8523,#8524));
#1515=EDGE_LOOP('',(#8525,#8526,#8527,#8528));
#1516=EDGE_LOOP('',(#8529,#8530,#8531,#8532));
#1517=EDGE_LOOP('',(#8533,#8534,#8535,#8536));
#1518=EDGE_LOOP('',(#8537,#8538,#8539,#8540));
#1519=EDGE_LOOP('',(#8541,#8542,#8543,#8544));
#1520=EDGE_LOOP('',(#8545,#8546,#8547,#8548));
#1521=EDGE_LOOP('',(#8549,#8550,#8551,#8552,#8553,#8554));
#1522=EDGE_LOOP('',(#8555));
#1523=EDGE_LOOP('',(#8556,#8557,#8558,#8559));
#1524=EDGE_LOOP('',(#8560,#8561,#8562,#8563));
#1525=EDGE_LOOP('',(#8564));
#1526=EDGE_LOOP('',(#8565,#8566,#8567,#8568,#8569,#8570));
#1527=EDGE_LOOP('',(#8571));
#1528=EDGE_LOOP('',(#8572,#8573,#8574,#8575));
#1529=EDGE_LOOP('',(#8576,#8577,#8578,#8579));
#1530=EDGE_LOOP('',(#8580,#8581,#8582,#8583));
#1531=EDGE_LOOP('',(#8584,#8585,#8586,#8587));
#1532=EDGE_LOOP('',(#8588,#8589,#8590,#8591));
#1533=EDGE_LOOP('',(#8592,#8593,#8594,#8595));
#1534=EDGE_LOOP('',(#8596,#8597,#8598,#8599));
#1535=EDGE_LOOP('',(#8600,#8601,#8602,#8603));
#1536=EDGE_LOOP('',(#8604,#8605,#8606,#8607));
#1537=EDGE_LOOP('',(#8608,#8609,#8610,#8611));
#1538=EDGE_LOOP('',(#8612,#8613,#8614,#8615));
#1539=EDGE_LOOP('',(#8616,#8617,#8618,#8619));
#1540=EDGE_LOOP('',(#8620,#8621,#8622,#8623));
#1541=EDGE_LOOP('',(#8624,#8625,#8626,#8627));
#1542=EDGE_LOOP('',(#8628,#8629,#8630,#8631));
#1543=EDGE_LOOP('',(#8632,#8633,#8634,#8635));
#1544=EDGE_LOOP('',(#8636,#8637,#8638,#8639));
#1545=EDGE_LOOP('',(#8640,#8641,#8642,#8643));
#1546=EDGE_LOOP('',(#8644,#8645,#8646,#8647));
#1547=EDGE_LOOP('',(#8648,#8649,#8650,#8651));
#1548=EDGE_LOOP('',(#8652,#8653,#8654,#8655));
#1549=EDGE_LOOP('',(#8656,#8657,#8658,#8659));
#1550=EDGE_LOOP('',(#8660,#8661,#8662,#8663));
#1551=EDGE_LOOP('',(#8664,#8665,#8666,#8667));
#1552=EDGE_LOOP('',(#8668,#8669,#8670,#8671));
#1553=EDGE_LOOP('',(#8672,#8673,#8674,#8675));
#1554=EDGE_LOOP('',(#8676,#8677,#8678,#8679));
#1555=EDGE_LOOP('',(#8680,#8681,#8682,#8683));
#1556=EDGE_LOOP('',(#8684,#8685,#8686,#8687));
#1557=EDGE_LOOP('',(#8688,#8689,#8690,#8691));
#1558=EDGE_LOOP('',(#8692,#8693,#8694,#8695));
#1559=EDGE_LOOP('',(#8696,#8697,#8698,#8699));
#1560=EDGE_LOOP('',(#8700,#8701,#8702,#8703));
#1561=EDGE_LOOP('',(#8704,#8705,#8706,#8707));
#1562=EDGE_LOOP('',(#8708,#8709,#8710,#8711));
#1563=EDGE_LOOP('',(#8712,#8713,#8714,#8715));
#1564=EDGE_LOOP('',(#8716,#8717,#8718,#8719,#8720,#8721,#8722,#8723));
#1565=EDGE_LOOP('',(#8724,#8725,#8726,#8727,#8728,#8729,#8730,#8731,#8732,
#8733,#8734,#8735,#8736,#8737,#8738,#8739,#8740,#8741,#8742,#8743,#8744,
#8745,#8746,#8747,#8748,#8749,#8750,#8751,#8752,#8753,#8754,#8755,#8756,
#8757,#8758,#8759,#8760,#8761,#8762,#8763));
#1566=EDGE_LOOP('',(#8764,#8765,#8766,#8767));
#1567=EDGE_LOOP('',(#8768,#8769,#8770,#8771,#8772,#8773,#8774,#8775,#8776,
#8777,#8778,#8779,#8780,#8781,#8782,#8783,#8784,#8785,#8786,#8787,#8788,
#8789,#8790,#8791,#8792,#8793,#8794,#8795,#8796,#8797,#8798,#8799,#8800,
#8801,#8802,#8803,#8804,#8805,#8806,#8807,#8808));
#1568=EDGE_LOOP('',(#8809,#8810,#8811,#8812));
#1569=EDGE_LOOP('',(#8813,#8814,#8815,#8816));
#1570=EDGE_LOOP('',(#8817,#8818,#8819,#8820));
#1571=EDGE_LOOP('',(#8821,#8822,#8823,#8824));
#1572=EDGE_LOOP('',(#8825,#8826,#8827,#8828));
#1573=EDGE_LOOP('',(#8829,#8830,#8831,#8832));
#1574=EDGE_LOOP('',(#8833,#8834,#8835,#8836));
#1575=EDGE_LOOP('',(#8837,#8838,#8839,#8840,#8841,#8842));
#1576=EDGE_LOOP('',(#8843));
#1577=EDGE_LOOP('',(#8844,#8845,#8846,#8847));
#1578=EDGE_LOOP('',(#8848,#8849,#8850,#8851));
#1579=EDGE_LOOP('',(#8852));
#1580=EDGE_LOOP('',(#8853,#8854,#8855,#8856,#8857,#8858));
#1581=EDGE_LOOP('',(#8859));
#1582=CIRCLE('',#9975,0.1666);
#1583=CIRCLE('',#9976,0.1666);
#1584=CIRCLE('',#9988,0.1666);
#1585=CIRCLE('',#9990,0.205475);
#1586=CIRCLE('',#10003,0.205475);
#1587=CIRCLE('',#10005,0.1666);
#1588=CIRCLE('',#10006,0.1666);
#1589=CIRCLE('',#10018,0.1666);
#1590=CIRCLE('',#10020,0.205475000000001);
#1591=CIRCLE('',#10033,0.205475000000001);
#1592=CIRCLE('',#10035,0.1666);
#1593=CIRCLE('',#10036,0.1666);
#1594=CIRCLE('',#10048,0.1666);
#1595=CIRCLE('',#10050,0.205475000000001);
#1596=CIRCLE('',#10063,0.205475000000001);
#1597=CIRCLE('',#10065,0.1666);
#1598=CIRCLE('',#10066,0.1666);
#1599=CIRCLE('',#10078,0.1666);
#1600=CIRCLE('',#10080,0.205475);
#1601=CIRCLE('',#10093,0.205475);
#1602=CIRCLE('',#10095,0.2);
#1603=CIRCLE('',#10096,0.2);
#1604=CIRCLE('',#10099,0.2);
#1605=CIRCLE('',#10100,0.2);
#1606=CIRCLE('',#10103,0.2);
#1607=CIRCLE('',#10104,0.2);
#1608=CIRCLE('',#10106,0.2);
#1609=CIRCLE('',#10107,0.8);
#1610=CIRCLE('',#10108,0.25);
#1611=CIRCLE('',#10109,0.25);
#1612=CIRCLE('',#10111,0.6);
#1613=CIRCLE('',#10113,0.2);
#1614=CIRCLE('',#10115,0.6);
#1615=CIRCLE('',#10117,0.4);
#1616=CIRCLE('',#10118,0.25);
#1617=CIRCLE('',#10120,0.4);
#1618=CIRCLE('',#10123,0.4);
#1619=CIRCLE('',#10124,0.25);
#1620=CIRCLE('',#10126,0.4);
#1621=CIRCLE('',#10145,0.3);
#1622=CIRCLE('',#10146,0.3);
#1623=CIRCLE('',#10148,0.3);
#1624=CIRCLE('',#10149,0.3);
#1625=CIRCLE('',#10159,0.65);
#1626=CIRCLE('',#10160,0.65);
#1627=CIRCLE('',#10162,0.8);
#1628=CIRCLE('',#10174,0.25);
#1629=CIRCLE('',#10175,0.25);
#1630=CIRCLE('',#10177,0.25);
#1631=CIRCLE('',#10178,0.25);
#1632=CIRCLE('',#10180,0.25);
#1633=CIRCLE('',#10181,0.25);
#1634=CIRCLE('',#10183,0.25);
#1635=CIRCLE('',#10184,0.25);
#1636=CIRCLE('',#10186,0.6);
#1637=CIRCLE('',#10187,0.6);
#1638=CIRCLE('',#10196,0.8);
#1639=CIRCLE('',#10197,0.6);
#1640=CIRCLE('',#10199,0.8);
#1641=CIRCLE('',#10201,0.4);
#1642=CIRCLE('',#10203,0.4);
#1643=CIRCLE('',#10205,0.6);
#1644=CIRCLE('',#10209,0.12645);
#1645=CIRCLE('',#10217,0.12645);
#1646=CIRCLE('',#10219,0.12645);
#1647=CIRCLE('',#10227,0.12645);
#1648=CIRCLE('',#10229,0.1543);
#1649=CIRCLE('',#10237,0.1543);
#1650=CIRCLE('',#10239,0.1543);
#1651=CIRCLE('',#10247,0.1543);
#1652=CIRCLE('',#10250,1.);
#1653=CIRCLE('',#10255,0.2);
#1654=CIRCLE('',#10256,0.2);
#1655=CIRCLE('',#10258,0.2);
#1656=CIRCLE('',#10259,0.2);
#1657=CIRCLE('',#10267,0.6);
#1658=CIRCLE('',#10269,0.6);
#1659=CIRCLE('',#10270,0.6);
#1660=CIRCLE('',#10280,1.);
#1661=CIRCLE('',#10282,0.6);
#1662=CIRCLE('',#10286,0.2);
#1663=CIRCLE('',#10287,0.2);
#1664=CIRCLE('',#10289,0.2);
#1665=CIRCLE('',#10290,0.2);
#1666=CIRCLE('',#10299,0.7);
#1667=CIRCLE('',#10300,0.6);
#1668=CIRCLE('',#10302,0.7);
#1669=CIRCLE('',#10304,0.4);
#1670=CIRCLE('',#10306,0.6);
#1671=CIRCLE('',#10308,0.4);
#1672=CIRCLE('',#10310,0.3);
#1673=CIRCLE('',#10312,0.3);
#1674=CIRCLE('',#10316,0.1666);
#1675=CIRCLE('',#10317,0.1666);
#1676=CIRCLE('',#10329,0.1666);
#1677=CIRCLE('',#10331,0.205475);
#1678=CIRCLE('',#10344,0.205475);
#1679=CIRCLE('',#10346,0.12645);
#1680=CIRCLE('',#10347,0.12645);
#1681=CIRCLE('',#10348,0.12645);
#1682=CIRCLE('',#10366,0.12645);
#1683=CIRCLE('',#10368,0.1543);
#1684=CIRCLE('',#10386,0.1543);
#1685=CIRCLE('',#10403,0.12645);
#1686=CIRCLE('',#10404,0.12645);
#1687=CIRCLE('',#10405,0.12645);
#1688=CIRCLE('',#10415,0.12645);
#1689=CIRCLE('',#10417,0.1543);
#1690=CIRCLE('',#10427,0.1543);
#1691=CIRCLE('',#10433,0.2);
#1692=CIRCLE('',#10434,0.2);
#1693=CIRCLE('',#10445,0.2);
#1694=CIRCLE('',#10446,0.2);
#1695=CIRCLE('',#10455,0.2);
#1696=CIRCLE('',#10456,0.2);
#1697=CIRCLE('',#10458,0.3);
#1698=CIRCLE('',#10459,0.3);
#1699=CIRCLE('',#10464,0.15);
#1700=CIRCLE('',#10465,0.15);
#1701=CIRCLE('',#10467,0.2);
#1702=CIRCLE('',#10469,0.2);
#1703=CIRCLE('',#10471,0.2);
#1704=CIRCLE('',#10473,0.4);
#1705=CIRCLE('',#10474,0.2);
#1706=CIRCLE('',#10476,0.4);
#1707=CIRCLE('',#10484,0.35);
#1708=CIRCLE('',#10485,0.15);
#1709=CIRCLE('',#10487,0.15);
#1710=CIRCLE('',#10489,0.35);
#1711=CIRCLE('',#10492,0.1);
#1712=CIRCLE('',#10493,0.1);
#1713=CIRCLE('',#10498,0.2);
#1714=CIRCLE('',#10499,0.2);
#1715=CIRCLE('',#10501,0.4);
#1716=CIRCLE('',#10502,0.4);
#1717=CIRCLE('',#10507,0.1954);
#1718=CIRCLE('',#10524,0.15555);
#1719=CIRCLE('',#10541,0.1954);
#1720=CIRCLE('',#10542,0.1);
#1721=CIRCLE('',#10544,0.15555);
#1722=CIRCLE('',#10554,0.35);
#1723=CIRCLE('',#10556,0.35);
#1724=CIRCLE('',#10561,0.14635);
#1725=CIRCLE('',#10572,0.117775);
#1726=CIRCLE('',#10583,0.14635);
#1727=CIRCLE('',#10584,0.05);
#1728=CIRCLE('',#10586,0.117775);
#1729=CIRCLE('',#10596,0.3);
#1730=CIRCLE('',#10598,0.3);
#1731=CIRCLE('',#10603,0.14635);
#1732=CIRCLE('',#10622,0.117775);
#1733=CIRCLE('',#10641,0.14635);
#1734=CIRCLE('',#10642,0.05);
#1735=CIRCLE('',#10644,0.117775);
#1736=CIRCLE('',#10654,0.3);
#1737=CIRCLE('',#10656,0.3);
#1738=B_SPLINE_CURVE_WITH_KNOTS('',3,(#12707,#12708,#12709,#12710,#12711,
#12712,#12713,#12714,#12715,#12716,#12717,#12718,#12719,#12720,#12721,#12722,
#12723,#12724,#12725,#12726,#12727,#12728),.UNSPECIFIED.,.F.,.F.,(4,3,3,
3,3,3,3,4),(76.708045941327,76.8129957196859,77.8105670926688,78.8081384656518,
79.8057098386347,80.8032812116176,81.8008525846006,82.7984239575835),
 .UNSPECIFIED.);
#1739=B_SPLINE_CURVE_WITH_KNOTS('',3,(#12732,#12733,#12734,#12735,#12736,
#12737,#12738),.UNSPECIFIED.,.F.,.F.,(4,3,4),(-80.783811092309,-79.8057098386347,
-79.2446069498473),.UNSPECIFIED.);
#1740=B_SPLINE_CURVE_WITH_KNOTS('',3,(#12742,#12743,#12744,#12745,#12746,
#12747,#12748,#12749,#12750,#12751,#12752,#12753,#12754,#12755,#12756,#12757,
#12758,#12759,#12760,#12761,#12762,#12763),.UNSPECIFIED.,.F.,.F.,(4,3,3,
3,3,3,3,4),(-79.2446069498473,-78.8081384656518,-77.8105670926688,-76.8129957196859,
-75.815424346703,-74.81785297372,-73.8202816007371,-72.9614216426678),
 .UNSPECIFIED.);
#1741=B_SPLINE_CURVE_WITH_KNOTS('',3,(#12768,#12769,#12770,#12771,#12772,
#12773,#12774,#12775,#12776,#12777,#12778,#12779,#12780,#12781,#12782,#12783,
#12784,#12785,#12786,#12787,#12788,#12789),.UNSPECIFIED.,.F.,.F.,(4,3,3,
3,3,3,3,4),(70.4248606341475,70.8275674817883,71.8251388547712,72.8227102277542,
73.8202816007371,74.81785297372,75.815424346703,76.708045941327),
 .UNSPECIFIED.);
#1742=B_SPLINE_CURVE_WITH_KNOTS('',3,(#12790,#12791,#12792,#12793,#12794,
#12795,#12796,#12797,#12798,#12799,#12800,#12801,#12802,#12803,#12804,#12805,
#12806,#12807,#12808,#12809,#12810,#12811,#12812,#12813,#12814),
 .UNSPECIFIED.,.F.,.F.,(4,3,3,3,3,3,3,3,4),(-72.9614216426678,-72.8227102277542,
-71.8251388547712,-70.8275674817883,-69.8299961088054,-68.8324247358224,
-67.8348533628395,-66.8372819898566,-66.6782363354882),.UNSPECIFIED.);
#1743=B_SPLINE_CURVE_WITH_KNOTS('',3,(#12819,#12820,#12821,#12822,#12823,
#12824,#12825,#12826,#12827,#12828,#12829,#12830,#12831,#12832,#12833,#12834,
#12835,#12836,#12837,#12838,#12839,#12840),.UNSPECIFIED.,.F.,.F.,(4,3,3,
3,3,3,3,4),(64.1416753269678,64.8421392438907,65.8397106168736,66.8372819898565,
67.8348533628395,68.8324247358224,69.8299961088054,70.4248606341475),
 .UNSPECIFIED.);
#1744=B_SPLINE_CURVE_WITH_KNOTS('',3,(#12841,#12842,#12843,#12844,#12845,
#12846,#12847,#12848,#12849,#12850,#12851,#12852,#12853,#12854,#12855,#12856,
#12857,#12858,#12859,#12860,#12861,#12862),.UNSPECIFIED.,.F.,.F.,(4,3,3,
3,3,3,3,4),(-66.6782363354882,-65.8397106168736,-64.8421392438907,-63.8445678709078,
-62.8469964979248,-61.8494251249419,-60.851853751959,-60.3950510283085),
 .UNSPECIFIED.);
#1745=B_SPLINE_CURVE_WITH_KNOTS('',3,(#12867,#12868,#12869,#12870,#12871,
#12872,#12873,#12874,#12875,#12876,#12877,#12878,#12879,#12880,#12881,#12882,
#12883,#12884,#12885,#12886,#12887,#12888),.UNSPECIFIED.,.F.,.F.,(4,3,3,
3,3,3,3,4),(57.8584900197882,58.8567110059931,59.854282378976,60.8518537519589,
61.8494251249419,62.8469964979248,63.8445678709078,64.1416753269678),
 .UNSPECIFIED.);
#1746=B_SPLINE_CURVE_WITH_KNOTS('',3,(#12889,#12890,#12891,#12892,#12893,
#12894,#12895,#12896,#12897,#12898,#12899,#12900,#12901,#12902,#12903,#12904,
#12905,#12906,#12907,#12908,#12909,#12910),.UNSPECIFIED.,.F.,.F.,(4,3,3,
3,3,3,3,4),(-60.3950510283085,-59.854282378976,-58.8567110059931,-57.8591396330102,
-56.8615682600272,-55.8639968870443,-54.8664255140614,-54.1118657211289),
 .UNSPECIFIED.);
#1747=B_SPLINE_CURVE_WITH_KNOTS('',3,(#12915,#12916,#12917,#12918,#12919,
#12920,#12921,#12922,#12923,#12924,#12925,#12926,#12927,#12928,#12929,#12930,
#12931,#12932,#12933,#12934,#12935,#12936),.UNSPECIFIED.,.F.,.F.,(4,3,3,
3,3,3,3,4),(51.5753047126087,51.8737113951126,52.8712827680955,53.8688541410784,
54.8664255140614,55.8639968870443,56.8615682600272,57.8584900197882),
 .UNSPECIFIED.);
#1748=B_SPLINE_CURVE_WITH_KNOTS('',3,(#12937,#12938,#12939,#12940,#12941,
#12942,#12943,#12944,#12945,#12946,#12947,#12948,#12949,#12950,#12951,#12952,
#12953,#12954,#12955,#12956,#12957,#12958,#12959,#12960,#12961),
 .UNSPECIFIED.,.F.,.F.,(4,3,3,3,3,3,3,3,4),(-54.1118657211289,-53.8688541410784,
-52.8712827680955,-51.8737113951126,-50.8761400221296,-49.8785686491467,
-48.8809972761638,-47.8834259031808,-47.8286804139493),.UNSPECIFIED.);
#1749=B_SPLINE_CURVE_WITH_KNOTS('',3,(#12966,#12967,#12968,#12969,#12970,
#12971,#12972,#12973,#12974,#12975,#12976,#12977,#12978,#12979,#12980,#12981,
#12982,#12983,#12984,#12985,#12986,#12987),.UNSPECIFIED.,.F.,.F.,(4,3,3,
3,3,3,3,4),(45.2921194054291,45.888283157215,46.8858545301979,47.8834259031808,
48.8809972761637,49.8785686491467,50.8761400221296,51.5753047126087),
 .UNSPECIFIED.);
#1750=B_SPLINE_CURVE_WITH_KNOTS('',3,(#12988,#12989,#12990,#12991,#12992,
#12993,#12994,#12995,#12996,#12997,#12998,#12999,#13000,#13001,#13002,#13003,
#13004,#13005,#13006,#13007,#13008,#13009),.UNSPECIFIED.,.F.,.F.,(4,3,3,
3,3,3,3,4),(-47.8286804139493,-46.8858545301979,-45.888283157215,-44.890711784232,
-43.8931404112491,-42.8955690382662,-41.8979976652832,-41.5454951067698),
 .UNSPECIFIED.);
#1751=B_SPLINE_CURVE_WITH_KNOTS('',3,(#13014,#13015,#13016,#13017,#13018,
#13019,#13020,#13021,#13022,#13023,#13024,#13025,#13026,#13027,#13028,#13029,
#13030,#13031,#13032,#13033,#13034,#13035),.UNSPECIFIED.,.F.,.F.,(4,3,3,
3,3,3,3,4),(39.0089340982495,39.9028549193174,40.9004262923003,41.8979976652832,
42.8955690382662,43.8931404112491,44.890711784232,45.2921194054291),
 .UNSPECIFIED.);
#1752=B_SPLINE_CURVE_WITH_KNOTS('',3,(#13036,#13037,#13038,#13039,#13040,
#13041,#13042,#13043,#13044,#13045,#13046,#13047,#13048,#13049,#13050,#13051,
#13052,#13053,#13054,#13055,#13056,#13057),.UNSPECIFIED.,.F.,.F.,(4,3,3,
3,3,3,3,4),(-41.5454951067698,-40.9004262923003,-39.9028549193174,-38.9052835463344,
-37.9077121733515,-36.9101408003686,-35.9125694273856,-35.2623097995902),
 .UNSPECIFIED.);
#1753=B_SPLINE_CURVE_WITH_KNOTS('',3,(#13062,#13063,#13064,#13065,#13066,
#13067,#13068,#13069,#13070,#13071,#13072,#13073,#13074,#13075,#13076,#13077,
#13078,#13079,#13080,#13081,#13082,#13083,#13084,#13085,#13086),
 .UNSPECIFIED.,.F.,.F.,(4,3,3,3,3,3,3,3,4),(32.7257487910699,32.9198553084368,
33.9174266814197,34.9149980544027,35.9125694273856,36.9101408003685,37.9077121733515,
38.9052835463344,39.0089340982495),.UNSPECIFIED.);
#1754=B_SPLINE_CURVE_WITH_KNOTS('',3,(#13087,#13088,#13089,#13090,#13091,
#13092,#13093,#13094,#13095,#13096,#13097,#13098,#13099,#13100,#13101,#13102,
#13103,#13104,#13105,#13106,#13107,#13108),.UNSPECIFIED.,.F.,.F.,(4,3,3,
3,3,3,3,4),(-35.2623097995902,-34.9149980544027,-33.9174266814198,-32.9198553084368,
-31.9222839354539,-30.924712562471,-29.927141189488,-28.9791244924106),
 .UNSPECIFIED.);
#1755=B_SPLINE_CURVE_WITH_KNOTS('',3,(#13113,#13114,#13115,#13116,#13117,
#13118,#13119,#13120,#13121,#13122,#13123,#13124,#13125,#13126,#13127,#13128,
#13129,#13130,#13131,#13132,#13133,#13134),.UNSPECIFIED.,.F.,.F.,(4,3,3,
3,3,3,3,4),(26.4425634838903,26.9344270705392,27.9319984435221,28.9295698165051,
29.927141189488,30.9247125624709,31.9222839354539,32.7257487910699),
 .UNSPECIFIED.);
#1756=B_SPLINE_CURVE_WITH_KNOTS('',3,(#13135,#13136,#13137,#13138,#13139,
#13140,#13141,#13142,#13143,#13144,#13145,#13146,#13147,#13148,#13149,#13150,
#13151,#13152,#13153,#13154,#13155,#13156,#13157,#13158,#13159),
 .UNSPECIFIED.,.F.,.F.,(4,3,3,3,3,3,3,3,4),(-28.9791244924106,-28.9295698165051,
-27.9319984435222,-26.9344270705392,-25.9368556975563,-24.9392843245734,
-23.9417129515904,-22.9441415786075,-22.695939185231),.UNSPECIFIED.);
#1757=B_SPLINE_CURVE_WITH_KNOTS('',3,(#13164,#13165,#13166,#13167,#13168,
#13169,#13170,#13171,#13172,#13173,#13174,#13175,#13176,#13177,#13178,#13179,
#13180,#13181,#13182,#13183,#13184,#13185),.UNSPECIFIED.,.F.,.F.,(4,3,3,
3,3,3,3,4),(20.1593781767107,20.9489988326416,21.9465702056245,22.9441415786075,
23.9417129515904,24.9392843245733,25.9368556975563,26.4425634838903),
 .UNSPECIFIED.);
#1758=B_SPLINE_CURVE_WITH_KNOTS('',3,(#13186,#13187,#13188,#13189,#13190,
#13191,#13192,#13193,#13194,#13195,#13196,#13197,#13198,#13199,#13200,#13201,
#13202,#13203,#13204,#13205,#13206,#13207),.UNSPECIFIED.,.F.,.F.,(4,3,3,
3,3,3,3,4),(-22.695939185231,-21.9465702056245,-20.9489988326416,-19.9514274596587,
-18.9538560866757,-17.9562847136928,-16.9587133407099,-16.4127538780514),
 .UNSPECIFIED.);
#1759=B_SPLINE_CURVE_WITH_KNOTS('',3,(#13212,#13213,#13214,#13215,#13216,
#13217,#13218,#13219,#13220,#13221,#13222,#13223,#13224,#13225,#13226,#13227,
#13228,#13229,#13230,#13231,#13232,#13233,#13234,#13235,#13236),
 .UNSPECIFIED.,.F.,.F.,(4,3,3,3,3,3,3,3,4),(13.8761928695311,13.9659992217611,
14.963570594744,15.9611419677269,16.9587133407099,17.9562847136928,18.9538560866757,
19.9514274596587,20.1593781767107),.UNSPECIFIED.);
#1760=B_SPLINE_CURVE_WITH_KNOTS('',3,(#13237,#13238,#13239,#13240,#13241,
#13242,#13243,#13244,#13245,#13246,#13247,#13248,#13249,#13250,#13251,#13252,
#13253,#13254,#13255,#13256,#13257,#13258),.UNSPECIFIED.,.F.,.F.,(4,3,3,
3,3,3,3,4),(-16.4127538780514,-15.9611419677269,-14.963570594744,-13.9659992217611,
-12.9684278487781,-11.9708564757952,-10.9732851028123,-10.1295685708718),
 .UNSPECIFIED.);
#1761=B_SPLINE_CURVE_WITH_KNOTS('',3,(#13264,#13265,#13266,#13267,#13268,
#13269,#13270,#13271,#13272,#13273,#13274,#13275,#13276),.UNSPECIFIED.,
 .F.,.F.,(4,3,3,3,4),(-3.84638326369226,-2.9927141189488,-1.99514274596587,
-0.997571372982934,0.),.UNSPECIFIED.);
#1762=B_SPLINE_CURVE_WITH_KNOTS('',3,(#13279,#13280,#13281,#13282,#13283,
#13284,#13285,#13286,#13287,#13288,#13289,#13290,#13291,#13292,#13293,#13294,
#13295,#13296,#13297),.UNSPECIFIED.,.F.,.F.,(4,3,3,3,3,3,4),(2.01461286527449,
2.9927141189488,3.99028549193174,4.98785686491467,5.9854282378976,6.98299961088054,
7.59300756235157),.UNSPECIFIED.);
#1763=B_SPLINE_CURVE_WITH_KNOTS('',3,(#13303,#13304,#13305,#13306,#13307,
#13308,#13309),.UNSPECIFIED.,.F.,.F.,(4,1,1,1,4),(91.106186954104,91.6672898428914,
92.6648612158743,93.6624325888573,94.6600039618402),.UNSPECIFIED.);
#1764=B_SPLINE_CURVE_WITH_KNOTS('',3,(#13312,#13313,#13314,#13315,#13316,
#13317,#13318,#13319),.UNSPECIFIED.,.F.,.F.,(4,1,1,1,1,4),(91.106186954104,
91.2111367324628,92.2087081054457,93.2062794784287,94.2038508514116,95.1819521050859),
 .UNSPECIFIED.);
#1765=B_SPLINE_CURVE_WITH_KNOTS('',3,(#13324,#13325,#13326,#13327,#13328,
#13329,#13330,#13331,#13332,#13333),.UNSPECIFIED.,.F.,.F.,(4,1,1,1,1,1,
1,4),(84.8230016469245,85.6818616049938,86.6794329779767,87.6770043509596,
88.6745757239426,89.6721470969255,90.6697184699085,91.106186954104),
 .UNSPECIFIED.);
#1766=B_SPLINE_CURVE_WITH_KNOTS('',3,(#13334,#13335,#13336,#13337,#13338,
#13339,#13340,#13341,#13342,#13343),.UNSPECIFIED.,.F.,.F.,(4,1,1,1,1,1,
1,4),(84.8230016469244,85.2257084945652,86.2232798675481,87.2208512405311,
88.218422613514,89.2159939864969,90.2135653594799,91.106186954104),
 .UNSPECIFIED.);
#1767=B_SPLINE_CURVE_WITH_KNOTS('',3,(#13348,#13349,#13350,#13351,#13352,
#13353,#13354,#13355,#13356,#13357,#13358),.UNSPECIFIED.,.F.,.F.,(4,1,1,
1,1,1,1,1,4),(78.5398163397448,78.6988619941132,79.6964333670962,80.6940047400791,
81.6915761130621,82.689147486045,83.6867188590279,84.6842902320109,84.8230016469245),
 .UNSPECIFIED.);
#1768=B_SPLINE_CURVE_WITH_KNOTS('',3,(#13359,#13360,#13361,#13362,#13363,
#13364,#13365,#13366,#13367,#13368),.UNSPECIFIED.,.F.,.F.,(4,1,1,1,1,1,
1,4),(78.5398163397448,79.2402802566676,80.2378516296505,81.2354230026335,
82.2329943756164,83.2305657485993,84.2281371215823,84.8230016469244),
 .UNSPECIFIED.);
#1769=B_SPLINE_CURVE_WITH_KNOTS('',3,(#13373,#13374,#13375,#13376,#13377,
#13378,#13379,#13380,#13381,#13382),.UNSPECIFIED.,.F.,.F.,(4,1,1,1,1,1,
1,4),(72.2566310325652,72.7134337562156,73.7110051291986,74.7085765021815,
75.7061478751644,76.7037192481474,77.7012906211303,78.5398163397448),
 .UNSPECIFIED.);
#1770=B_SPLINE_CURVE_WITH_KNOTS('',3,(#13383,#13384,#13385,#13386,#13387,
#13388,#13389,#13390,#13391,#13392,#13393),.UNSPECIFIED.,.F.,.F.,(4,1,1,
1,1,1,1,1,4),(72.2566310325652,72.2572806457871,73.25485201877,74.2524233917529,
75.2499947647359,76.2475661377188,77.2451375107017,78.2427088836847,78.5398163397448),
 .UNSPECIFIED.);
#1771=B_SPLINE_CURVE_WITH_KNOTS('',3,(#13398,#13399,#13400,#13401,#13402,
#13403,#13404,#13405,#13406,#13407),.UNSPECIFIED.,.F.,.F.,(4,1,1,1,1,1,
1,4),(65.9734457253856,66.728005518318,67.725576891301,68.7231482642839,
69.7207196372669,70.7182910102498,71.7158623832327,72.2566310325652),
 .UNSPECIFIED.);
#1772=B_SPLINE_CURVE_WITH_KNOTS('',3,(#13408,#13409,#13410,#13411,#13412,
#13413,#13414,#13415,#13416,#13417),.UNSPECIFIED.,.F.,.F.,(4,1,1,1,1,1,
1,4),(65.9734457253856,66.2718524078895,67.2694237808724,68.2669951538553,
69.2645665268383,70.2621378998212,71.2597092728041,72.2566310325652),
 .UNSPECIFIED.);
#1773=B_SPLINE_CURVE_WITH_KNOTS('',3,(#13422,#13423,#13424,#13425,#13426,
#13427,#13428,#13429,#13430,#13431,#13432),.UNSPECIFIED.,.F.,.F.,(4,1,1,
1,1,1,1,1,4),(59.690260418206,59.7450059074375,60.7425772804204,61.7401486534034,
62.7377200263863,63.7352913993692,64.7328627723522,65.7304341453351,65.9734457253856),
 .UNSPECIFIED.);
#1774=B_SPLINE_CURVE_WITH_KNOTS('',3,(#13433,#13434,#13435,#13436,#13437,
#13438,#13439,#13440,#13441,#13442),.UNSPECIFIED.,.F.,.F.,(4,1,1,1,1,1,
1,4),(59.690260418206,60.2864241699919,61.2839955429748,62.2815669159577,
63.2791382889407,64.2767096619236,65.2742810349065,65.9734457253856),
 .UNSPECIFIED.);
#1775=B_SPLINE_CURVE_WITH_KNOTS('',3,(#13447,#13448,#13449,#13450,#13451,
#13452,#13453,#13454,#13455,#13456),.UNSPECIFIED.,.F.,.F.,(4,1,1,1,1,1,
1,4),(53.4070751110265,53.7595776695399,54.7571490425228,55.7547204155058,
56.7522917884887,57.7498631614716,58.7474345344546,59.690260418206),
 .UNSPECIFIED.);
#1776=B_SPLINE_CURVE_WITH_KNOTS('',3,(#13457,#13458,#13459,#13460,#13461,
#13462,#13463,#13464,#13465,#13466),.UNSPECIFIED.,.F.,.F.,(4,1,1,1,1,1,
1,4),(53.4070751110264,54.3009959320943,55.2985673050772,56.2961386780601,
57.2937100510431,58.291281424026,59.2888527970089,59.690260418206),
 .UNSPECIFIED.);
#1777=B_SPLINE_CURVE_WITH_KNOTS('',3,(#13471,#13472,#13473,#13474,#13475,
#13476,#13477,#13478,#13479,#13480),.UNSPECIFIED.,.F.,.F.,(4,1,1,1,1,1,
1,4),(47.1238898038469,47.7741494316423,48.7717208046252,49.7692921776082,
50.7668635505911,51.764434923574,52.762006296557,53.4070751110265),
 .UNSPECIFIED.);
#1778=B_SPLINE_CURVE_WITH_KNOTS('',3,(#13481,#13482,#13483,#13484,#13485,
#13486,#13487,#13488,#13489,#13490,#13491),.UNSPECIFIED.,.F.,.F.,(4,1,1,
1,1,1,1,1,4),(47.1238898038469,47.3179963212137,48.3155676941967,49.3131390671796,
50.3107104401625,51.3082818131455,52.3058531861284,53.3034245591113,53.4070751110264),
 .UNSPECIFIED.);
#1779=B_SPLINE_CURVE_WITH_KNOTS('',3,(#13496,#13497,#13498,#13499,#13500,
#13501,#13502,#13503,#13504,#13505),.UNSPECIFIED.,.F.,.F.,(4,1,1,1,1,1,
1,4),(40.8407044966673,41.7887211937447,42.7862925667276,43.7838639397106,
44.7814353126935,45.7790066856764,46.7765780586594,47.1238898038469),
 .UNSPECIFIED.);
#1780=B_SPLINE_CURVE_WITH_KNOTS('',3,(#13506,#13507,#13508,#13509,#13510,
#13511,#13512,#13513,#13514,#13515),.UNSPECIFIED.,.F.,.F.,(4,1,1,1,1,1,
1,4),(40.8407044966673,41.3325680833161,42.3301394562991,43.327710829282,
44.3252822022649,45.3228535752479,46.3204249482308,47.1238898038469),
 .UNSPECIFIED.);
#1781=B_SPLINE_CURVE_WITH_KNOTS('',3,(#13520,#13521,#13522,#13523,#13524,
#13525,#13526,#13527,#13528,#13529,#13530),.UNSPECIFIED.,.F.,.F.,(4,1,1,
1,1,1,1,1,4),(34.5575191894876,34.8057215828642,35.8032929558471,36.80086432883,
37.798435701813,38.7960070747959,39.7935784477788,40.7911498207618,40.8407044966673),
 .UNSPECIFIED.);
#1782=B_SPLINE_CURVE_WITH_KNOTS('',3,(#13531,#13532,#13533,#13534,#13535,
#13536,#13537,#13538,#13539,#13540),.UNSPECIFIED.,.F.,.F.,(4,1,1,1,1,1,
1,4),(34.5575191894876,35.3471398454185,36.3447112184015,37.3422825913844,
38.3398539643673,39.3374253373503,40.3349967103332,40.8407044966673),
 .UNSPECIFIED.);
#1783=B_SPLINE_CURVE_WITH_KNOTS('',3,(#13545,#13546,#13547,#13548,#13549,
#13550,#13551,#13552,#13553,#13554),.UNSPECIFIED.,.F.,.F.,(4,1,1,1,1,1,
1,4),(28.2743338823081,28.8202933449666,29.8178647179495,30.8154360909324,
31.8130074639154,32.8105788368983,33.8081502098812,34.5575191894876),
 .UNSPECIFIED.);
#1784=B_SPLINE_CURVE_WITH_KNOTS('',3,(#13555,#13556,#13557,#13558,#13559,
#13560,#13561,#13562,#13563,#13564,#13565),.UNSPECIFIED.,.F.,.F.,(4,1,1,
1,1,1,1,1,4),(28.2743338823081,28.364140234538,29.3617116075209,30.3592829805039,
31.3568543534868,32.3544257264697,33.3519970994527,34.3495684724356,34.5575191894876),
 .UNSPECIFIED.);
#1785=B_SPLINE_CURVE_WITH_KNOTS('',3,(#13570,#13571,#13572,#13573,#13574,
#13575,#13576,#13577,#13578,#13579),.UNSPECIFIED.,.F.,.F.,(4,1,1,1,1,1,
1,4),(21.9911485751285,22.834865107069,23.8324364800519,24.8300078530348,
25.8275792260178,26.8251505990007,27.8227219719836,28.2743338823081),
 .UNSPECIFIED.);
#1786=B_SPLINE_CURVE_WITH_KNOTS('',3,(#13580,#13581,#13582,#13583,#13584,
#13585,#13586,#13587,#13588,#13589),.UNSPECIFIED.,.F.,.F.,(4,1,1,1,1,1,
1,4),(21.9911485751285,22.3787119966404,23.3762833696233,24.3738547426063,
25.3714261155892,26.3689974885721,27.3665688615551,28.2743338823081),
 .UNSPECIFIED.);
#1787=B_SPLINE_CURVE_WITH_KNOTS('',3,(#13595,#13596,#13597,#13598,#13599),
 .UNSPECIFIED.,.F.,.F.,(4,1,4),(14.3981410127769,15.3957123857599,15.7079632679489),
 .UNSPECIFIED.);
#1788=B_SPLINE_CURVE_WITH_KNOTS('',3,(#13602,#13603,#13604,#13605,#13606),
 .UNSPECIFIED.,.F.,.F.,(4,1,4),(13.8761928695312,14.8542941232055,15.7079632679489),
 .UNSPECIFIED.);
#1789=B_SPLINE_CURVE_WITH_KNOTS('',3,(#13612,#13613,#13614,#13615,#13616,
#13617,#13618,#13619,#13620,#13621,#13622,#13623,#13624,#13625,#13626,#13627,
#13628,#13629,#13630,#13631,#13632,#13633),.UNSPECIFIED.,.F.,.F.,(4,3,3,
3,3,3,3,4),(76.7080459413271,76.8129957196859,77.8105670926688,78.8081384656517,
79.8057098386347,80.8032812116176,81.8008525846006,82.7984239575835),
 .UNSPECIFIED.);
#1790=B_SPLINE_CURVE_WITH_KNOTS('',3,(#13637,#13638,#13639,#13640,#13641,
#13642,#13643),.UNSPECIFIED.,.F.,.F.,(4,3,4),(-80.783811092309,-79.8057098386347,
-79.2446069498473),.UNSPECIFIED.);
#1791=B_SPLINE_CURVE_WITH_KNOTS('',3,(#13647,#13648,#13649,#13650,#13651,
#13652,#13653,#13654,#13655,#13656,#13657,#13658,#13659,#13660,#13661,#13662,
#13663,#13664,#13665,#13666,#13667,#13668),.UNSPECIFIED.,.F.,.F.,(4,3,3,
3,3,3,3,4),(-79.2446069498473,-78.8081384656518,-77.8105670926688,-76.8129957196859,
-75.815424346703,-74.81785297372,-73.8202816007371,-72.9614216426678),
 .UNSPECIFIED.);
#1792=B_SPLINE_CURVE_WITH_KNOTS('',3,(#13673,#13674,#13675,#13676,#13677,
#13678,#13679,#13680,#13681,#13682,#13683,#13684,#13685,#13686,#13687,#13688,
#13689,#13690,#13691,#13692,#13693,#13694),.UNSPECIFIED.,.F.,.F.,(4,3,3,
3,3,3,3,4),(70.4248606341475,70.8275674817883,71.8251388547712,72.8227102277542,
73.8202816007371,74.81785297372,75.815424346703,76.7080459413271),
 .UNSPECIFIED.);
#1793=B_SPLINE_CURVE_WITH_KNOTS('',3,(#13695,#13696,#13697,#13698,#13699,
#13700,#13701,#13702,#13703,#13704,#13705,#13706,#13707,#13708,#13709,#13710,
#13711,#13712,#13713,#13714,#13715,#13716,#13717,#13718,#13719),
 .UNSPECIFIED.,.F.,.F.,(4,3,3,3,3,3,3,3,4),(-72.9614216426678,-72.8227102277542,
-71.8251388547712,-70.8275674817883,-69.8299961088054,-68.8324247358224,
-67.8348533628395,-66.8372819898566,-66.6782363354882),.UNSPECIFIED.);
#1794=B_SPLINE_CURVE_WITH_KNOTS('',3,(#13724,#13725,#13726,#13727,#13728,
#13729,#13730,#13731,#13732,#13733,#13734,#13735,#13736,#13737,#13738,#13739,
#13740,#13741,#13742,#13743,#13744,#13745),.UNSPECIFIED.,.F.,.F.,(4,3,3,
3,3,3,3,4),(64.1416753269678,64.8421392438907,65.8397106168736,66.8372819898565,
67.8348533628395,68.8324247358224,69.8299961088054,70.4248606341475),
 .UNSPECIFIED.);
#1795=B_SPLINE_CURVE_WITH_KNOTS('',3,(#13746,#13747,#13748,#13749,#13750,
#13751,#13752,#13753,#13754,#13755,#13756,#13757,#13758,#13759,#13760,#13761,
#13762,#13763,#13764,#13765,#13766,#13767),.UNSPECIFIED.,.F.,.F.,(4,3,3,
3,3,3,3,4),(-66.6782363354882,-65.8397106168736,-64.8421392438907,-63.8445678709078,
-62.8469964979248,-61.8494251249419,-60.851853751959,-60.3950510283085),
 .UNSPECIFIED.);
#1796=B_SPLINE_CURVE_WITH_KNOTS('',3,(#13772,#13773,#13774,#13775,#13776,
#13777,#13778,#13779,#13780,#13781,#13782,#13783,#13784,#13785,#13786,#13787,
#13788,#13789,#13790,#13791,#13792,#13793),.UNSPECIFIED.,.F.,.F.,(4,3,3,
3,3,3,3,4),(57.8584900197882,58.8567110059931,59.854282378976,60.851853751959,
61.8494251249419,62.8469964979248,63.8445678709078,64.1416753269678),
 .UNSPECIFIED.);
#1797=B_SPLINE_CURVE_WITH_KNOTS('',3,(#13794,#13795,#13796,#13797,#13798,
#13799,#13800,#13801,#13802,#13803,#13804,#13805,#13806,#13807,#13808,#13809,
#13810,#13811,#13812,#13813,#13814,#13815),.UNSPECIFIED.,.F.,.F.,(4,3,3,
3,3,3,3,4),(-60.3950510283085,-59.854282378976,-58.8567110059931,-57.8591396330102,
-56.8615682600272,-55.8639968870443,-54.8664255140614,-54.1118657211289),
 .UNSPECIFIED.);
#1798=B_SPLINE_CURVE_WITH_KNOTS('',3,(#13820,#13821,#13822,#13823,#13824,
#13825,#13826,#13827,#13828,#13829,#13830,#13831,#13832,#13833,#13834,#13835,
#13836,#13837,#13838,#13839,#13840,#13841),.UNSPECIFIED.,.F.,.F.,(4,3,3,
3,3,3,3,4),(51.5753047126086,51.8737113951126,52.8712827680955,53.8688541410784,
54.8664255140613,55.8639968870443,56.8615682600272,57.8584900197882),
 .UNSPECIFIED.);
#1799=B_SPLINE_CURVE_WITH_KNOTS('',3,(#13842,#13843,#13844,#13845,#13846,
#13847,#13848,#13849,#13850,#13851,#13852,#13853,#13854,#13855,#13856,#13857,
#13858,#13859,#13860,#13861,#13862,#13863,#13864,#13865,#13866),
 .UNSPECIFIED.,.F.,.F.,(4,3,3,3,3,3,3,3,4),(-54.1118657211289,-53.8688541410784,
-52.8712827680955,-51.8737113951126,-50.8761400221296,-49.8785686491467,
-48.8809972761638,-47.8834259031808,-47.8286804139494),.UNSPECIFIED.);
#1800=B_SPLINE_CURVE_WITH_KNOTS('',3,(#13871,#13872,#13873,#13874,#13875,
#13876,#13877,#13878,#13879,#13880,#13881,#13882,#13883,#13884,#13885,#13886,
#13887,#13888,#13889,#13890,#13891,#13892),.UNSPECIFIED.,.F.,.F.,(4,3,3,
3,3,3,3,4),(45.2921194054291,45.8882831572149,46.8858545301979,47.8834259031808,
48.8809972761637,49.8785686491467,50.8761400221296,51.5753047126086),
 .UNSPECIFIED.);
#1801=B_SPLINE_CURVE_WITH_KNOTS('',3,(#13893,#13894,#13895,#13896,#13897,
#13898,#13899,#13900,#13901,#13902,#13903,#13904,#13905,#13906,#13907,#13908,
#13909,#13910,#13911,#13912,#13913,#13914),.UNSPECIFIED.,.F.,.F.,(4,3,3,
3,3,3,3,4),(-47.8286804139494,-46.8858545301979,-45.888283157215,-44.890711784232,
-43.8931404112491,-42.8955690382662,-41.8979976652832,-41.5454951067698),
 .UNSPECIFIED.);
#1802=B_SPLINE_CURVE_WITH_KNOTS('',3,(#13919,#13920,#13921,#13922,#13923,
#13924,#13925,#13926,#13927,#13928,#13929,#13930,#13931,#13932,#13933,#13934,
#13935,#13936,#13937,#13938,#13939,#13940),.UNSPECIFIED.,.F.,.F.,(4,3,3,
3,3,3,3,4),(39.0089340982495,39.9028549193173,40.9004262923003,41.8979976652832,
42.8955690382661,43.8931404112491,44.890711784232,45.2921194054291),
 .UNSPECIFIED.);
#1803=B_SPLINE_CURVE_WITH_KNOTS('',3,(#13941,#13942,#13943,#13944,#13945,
#13946,#13947,#13948,#13949,#13950,#13951,#13952,#13953,#13954,#13955,#13956,
#13957,#13958,#13959,#13960,#13961,#13962),.UNSPECIFIED.,.F.,.F.,(4,3,3,
3,3,3,3,4),(-41.5454951067698,-40.9004262923003,-39.9028549193174,-38.9052835463344,
-37.9077121733515,-36.9101408003686,-35.9125694273856,-35.2623097995902),
 .UNSPECIFIED.);
#1804=B_SPLINE_CURVE_WITH_KNOTS('',3,(#13967,#13968,#13969,#13970,#13971,
#13972,#13973,#13974,#13975,#13976,#13977,#13978,#13979,#13980,#13981,#13982,
#13983,#13984,#13985,#13986,#13987,#13988,#13989,#13990,#13991),
 .UNSPECIFIED.,.F.,.F.,(4,3,3,3,3,3,3,3,4),(32.7257487910699,32.9198553084368,
33.9174266814197,34.9149980544027,35.9125694273856,36.9101408003685,37.9077121733515,
38.9052835463344,39.0089340982495),.UNSPECIFIED.);
#1805=B_SPLINE_CURVE_WITH_KNOTS('',3,(#13992,#13993,#13994,#13995,#13996,
#13997,#13998,#13999,#14000,#14001,#14002,#14003,#14004,#14005,#14006,#14007,
#14008,#14009,#14010,#14011,#14012,#14013),.UNSPECIFIED.,.F.,.F.,(4,3,3,
3,3,3,3,4),(-35.2623097995902,-34.9149980544027,-33.9174266814198,-32.9198553084368,
-31.9222839354539,-30.924712562471,-29.927141189488,-28.9791244924106),
 .UNSPECIFIED.);
#1806=B_SPLINE_CURVE_WITH_KNOTS('',3,(#14018,#14019,#14020,#14021,#14022,
#14023,#14024,#14025,#14026,#14027,#14028,#14029,#14030,#14031,#14032,#14033,
#14034,#14035,#14036,#14037,#14038,#14039),.UNSPECIFIED.,.F.,.F.,(4,3,3,
3,3,3,3,4),(26.4425634838903,26.9344270705392,27.9319984435221,28.9295698165051,
29.927141189488,30.9247125624709,31.9222839354539,32.7257487910699),
 .UNSPECIFIED.);
#1807=B_SPLINE_CURVE_WITH_KNOTS('',3,(#14040,#14041,#14042,#14043,#14044,
#14045,#14046,#14047,#14048,#14049,#14050,#14051,#14052,#14053,#14054,#14055,
#14056,#14057,#14058,#14059,#14060,#14061,#14062,#14063,#14064),
 .UNSPECIFIED.,.F.,.F.,(4,3,3,3,3,3,3,3,4),(-28.9791244924106,-28.9295698165051,
-27.9319984435222,-26.9344270705392,-25.9368556975563,-24.9392843245733,
-23.9417129515904,-22.9441415786075,-22.695939185231),.UNSPECIFIED.);
#1808=B_SPLINE_CURVE_WITH_KNOTS('',3,(#14069,#14070,#14071,#14072,#14073,
#14074,#14075,#14076,#14077,#14078,#14079,#14080,#14081,#14082,#14083,#14084,
#14085,#14086,#14087,#14088,#14089,#14090),.UNSPECIFIED.,.F.,.F.,(4,3,3,
3,3,3,3,4),(20.1593781767107,20.9489988326416,21.9465702056245,22.9441415786075,
23.9417129515904,24.9392843245733,25.9368556975563,26.4425634838903),
 .UNSPECIFIED.);
#1809=B_SPLINE_CURVE_WITH_KNOTS('',3,(#14091,#14092,#14093,#14094,#14095,
#14096,#14097,#14098,#14099,#14100,#14101,#14102,#14103,#14104,#14105,#14106,
#14107,#14108,#14109,#14110,#14111,#14112),.UNSPECIFIED.,.F.,.F.,(4,3,3,
3,3,3,3,4),(-22.695939185231,-21.9465702056245,-20.9489988326416,-19.9514274596587,
-18.9538560866757,-17.9562847136928,-16.9587133407099,-16.4127538780514),
 .UNSPECIFIED.);
#1810=B_SPLINE_CURVE_WITH_KNOTS('',3,(#14117,#14118,#14119,#14120,#14121,
#14122,#14123,#14124,#14125,#14126,#14127,#14128,#14129,#14130,#14131,#14132,
#14133,#14134,#14135,#14136,#14137,#14138,#14139,#14140,#14141),
 .UNSPECIFIED.,.F.,.F.,(4,3,3,3,3,3,3,3,4),(13.8761928695311,13.9659992217611,
14.963570594744,15.9611419677269,16.9587133407099,17.9562847136928,18.9538560866757,
19.9514274596587,20.1593781767107),.UNSPECIFIED.);
#1811=B_SPLINE_CURVE_WITH_KNOTS('',3,(#14142,#14143,#14144,#14145,#14146,
#14147,#14148,#14149,#14150,#14151,#14152,#14153,#14154,#14155,#14156,#14157,
#14158,#14159,#14160,#14161,#14162,#14163),.UNSPECIFIED.,.F.,.F.,(4,3,3,
3,3,3,3,4),(-16.4127538780514,-15.9611419677269,-14.963570594744,-13.9659992217611,
-12.9684278487781,-11.9708564757952,-10.9732851028123,-10.1295685708718),
 .UNSPECIFIED.);
#1812=B_SPLINE_CURVE_WITH_KNOTS('',3,(#14169,#14170,#14171,#14172,#14173,
#14174,#14175,#14176,#14177,#14178,#14179,#14180,#14181),.UNSPECIFIED.,
 .F.,.F.,(4,3,3,3,4),(-3.84638326369226,-2.9927141189488,-1.99514274596587,
-0.997571372982934,0.),.UNSPECIFIED.);
#1813=B_SPLINE_CURVE_WITH_KNOTS('',3,(#14184,#14185,#14186,#14187,#14188,
#14189,#14190,#14191,#14192,#14193,#14194,#14195,#14196,#14197,#14198,#14199,
#14200,#14201,#14202),.UNSPECIFIED.,.F.,.F.,(4,3,3,3,3,3,4),(2.01461286527457,
2.9927141189488,3.99028549193173,4.98785686491467,5.9854282378976,6.98299961088054,
7.59300756235157),.UNSPECIFIED.);
#1814=B_SPLINE_CURVE_WITH_KNOTS('',3,(#14208,#14209,#14210,#14211,#14212,
#14213,#14214),.UNSPECIFIED.,.F.,.F.,(4,1,1,1,4),(91.106186954104,91.6672898428914,
92.6648612158743,93.6624325888573,94.6600039618402),.UNSPECIFIED.);
#1815=B_SPLINE_CURVE_WITH_KNOTS('',3,(#14217,#14218,#14219,#14220,#14221,
#14222,#14223,#14224),.UNSPECIFIED.,.F.,.F.,(4,1,1,1,1,4),(91.106186954104,
91.2111367324628,92.2087081054457,93.2062794784287,94.2038508514116,95.1819521050859),
 .UNSPECIFIED.);
#1816=B_SPLINE_CURVE_WITH_KNOTS('',3,(#14229,#14230,#14231,#14232,#14233,
#14234,#14235,#14236,#14237,#14238),.UNSPECIFIED.,.F.,.F.,(4,1,1,1,1,1,
1,4),(84.8230016469244,85.6818616049938,86.6794329779767,87.6770043509596,
88.6745757239426,89.6721470969255,90.6697184699085,91.106186954104),
 .UNSPECIFIED.);
#1817=B_SPLINE_CURVE_WITH_KNOTS('',3,(#14239,#14240,#14241,#14242,#14243,
#14244,#14245,#14246,#14247,#14248),.UNSPECIFIED.,.F.,.F.,(4,1,1,1,1,1,
1,4),(84.8230016469244,85.2257084945652,86.2232798675481,87.2208512405311,
88.218422613514,89.2159939864969,90.2135653594799,91.106186954104),
 .UNSPECIFIED.);
#1818=B_SPLINE_CURVE_WITH_KNOTS('',3,(#14253,#14254,#14255,#14256,#14257,
#14258,#14259,#14260,#14261,#14262,#14263),.UNSPECIFIED.,.F.,.F.,(4,1,1,
1,1,1,1,1,4),(78.5398163397448,78.6988619941132,79.6964333670962,80.6940047400791,
81.6915761130621,82.689147486045,83.6867188590279,84.6842902320109,84.8230016469244),
 .UNSPECIFIED.);
#1819=B_SPLINE_CURVE_WITH_KNOTS('',3,(#14264,#14265,#14266,#14267,#14268,
#14269,#14270,#14271,#14272,#14273),.UNSPECIFIED.,.F.,.F.,(4,1,1,1,1,1,
1,4),(78.5398163397448,79.2402802566676,80.2378516296505,81.2354230026335,
82.2329943756164,83.2305657485993,84.2281371215823,84.8230016469244),
 .UNSPECIFIED.);
#1820=B_SPLINE_CURVE_WITH_KNOTS('',3,(#14278,#14279,#14280,#14281,#14282,
#14283,#14284,#14285,#14286,#14287),.UNSPECIFIED.,.F.,.F.,(4,1,1,1,1,1,
1,4),(72.2566310325652,72.7134337562156,73.7110051291986,74.7085765021815,
75.7061478751644,76.7037192481474,77.7012906211303,78.5398163397448),
 .UNSPECIFIED.);
#1821=B_SPLINE_CURVE_WITH_KNOTS('',3,(#14288,#14289,#14290,#14291,#14292,
#14293,#14294,#14295,#14296,#14297,#14298),.UNSPECIFIED.,.F.,.F.,(4,1,1,
1,1,1,1,1,4),(72.2566310325652,72.2572806457871,73.25485201877,74.2524233917529,
75.2499947647359,76.2475661377188,77.2451375107017,78.2427088836847,78.5398163397448),
 .UNSPECIFIED.);
#1822=B_SPLINE_CURVE_WITH_KNOTS('',3,(#14303,#14304,#14305,#14306,#14307,
#14308,#14309,#14310,#14311,#14312),.UNSPECIFIED.,.F.,.F.,(4,1,1,1,1,1,
1,4),(65.9734457253856,66.728005518318,67.725576891301,68.7231482642839,
69.7207196372668,70.7182910102498,71.7158623832327,72.2566310325652),
 .UNSPECIFIED.);
#1823=B_SPLINE_CURVE_WITH_KNOTS('',3,(#14313,#14314,#14315,#14316,#14317,
#14318,#14319,#14320,#14321,#14322),.UNSPECIFIED.,.F.,.F.,(4,1,1,1,1,1,
1,4),(65.9734457253856,66.2718524078895,67.2694237808724,68.2669951538553,
69.2645665268383,70.2621378998212,71.2597092728041,72.2566310325652),
 .UNSPECIFIED.);
#1824=B_SPLINE_CURVE_WITH_KNOTS('',3,(#14327,#14328,#14329,#14330,#14331,
#14332,#14333,#14334,#14335,#14336,#14337),.UNSPECIFIED.,.F.,.F.,(4,1,1,
1,1,1,1,1,4),(59.690260418206,59.7450059074375,60.7425772804204,61.7401486534034,
62.7377200263863,63.7352913993692,64.7328627723522,65.7304341453351,65.9734457253856),
 .UNSPECIFIED.);
#1825=B_SPLINE_CURVE_WITH_KNOTS('',3,(#14338,#14339,#14340,#14341,#14342,
#14343,#14344,#14345,#14346,#14347),.UNSPECIFIED.,.F.,.F.,(4,1,1,1,1,1,
1,4),(59.690260418206,60.2864241699919,61.2839955429748,62.2815669159577,
63.2791382889407,64.2767096619236,65.2742810349065,65.9734457253856),
 .UNSPECIFIED.);
#1826=B_SPLINE_CURVE_WITH_KNOTS('',3,(#14352,#14353,#14354,#14355,#14356,
#14357,#14358,#14359,#14360,#14361),.UNSPECIFIED.,.F.,.F.,(4,1,1,1,1,1,
1,4),(53.4070751110264,53.7595776695399,54.7571490425228,55.7547204155058,
56.7522917884887,57.7498631614716,58.7474345344546,59.690260418206),
 .UNSPECIFIED.);
#1827=B_SPLINE_CURVE_WITH_KNOTS('',3,(#14362,#14363,#14364,#14365,#14366,
#14367,#14368,#14369,#14370,#14371),.UNSPECIFIED.,.F.,.F.,(4,1,1,1,1,1,
1,4),(53.4070751110264,54.3009959320943,55.2985673050772,56.2961386780601,
57.2937100510431,58.291281424026,59.2888527970089,59.690260418206),
 .UNSPECIFIED.);
#1828=B_SPLINE_CURVE_WITH_KNOTS('',3,(#14376,#14377,#14378,#14379,#14380,
#14381,#14382,#14383,#14384,#14385),.UNSPECIFIED.,.F.,.F.,(4,1,1,1,1,1,
1,4),(47.1238898038469,47.7741494316423,48.7717208046252,49.7692921776082,
50.7668635505911,51.764434923574,52.762006296557,53.4070751110264),
 .UNSPECIFIED.);
#1829=B_SPLINE_CURVE_WITH_KNOTS('',3,(#14386,#14387,#14388,#14389,#14390,
#14391,#14392,#14393,#14394,#14395,#14396),.UNSPECIFIED.,.F.,.F.,(4,1,1,
1,1,1,1,1,4),(47.1238898038469,47.3179963212137,48.3155676941967,49.3131390671796,
50.3107104401625,51.3082818131455,52.3058531861284,53.3034245591113,53.4070751110264),
 .UNSPECIFIED.);
#1830=B_SPLINE_CURVE_WITH_KNOTS('',3,(#14401,#14402,#14403,#14404,#14405,
#14406,#14407,#14408,#14409,#14410),.UNSPECIFIED.,.F.,.F.,(4,1,1,1,1,1,
1,4),(40.8407044966673,41.7887211937447,42.7862925667276,43.7838639397106,
44.7814353126935,45.7790066856764,46.7765780586594,47.1238898038469),
 .UNSPECIFIED.);
#1831=B_SPLINE_CURVE_WITH_KNOTS('',3,(#14411,#14412,#14413,#14414,#14415,
#14416,#14417,#14418,#14419,#14420),.UNSPECIFIED.,.F.,.F.,(4,1,1,1,1,1,
1,4),(40.8407044966673,41.3325680833161,42.3301394562991,43.327710829282,
44.3252822022649,45.3228535752479,46.3204249482308,47.1238898038469),
 .UNSPECIFIED.);
#1832=B_SPLINE_CURVE_WITH_KNOTS('',3,(#14425,#14426,#14427,#14428,#14429,
#14430,#14431,#14432,#14433,#14434,#14435),.UNSPECIFIED.,.F.,.F.,(4,1,1,
1,1,1,1,1,4),(34.5575191894876,34.8057215828642,35.8032929558471,36.80086432883,
37.798435701813,38.7960070747959,39.7935784477788,40.7911498207618,40.8407044966673),
 .UNSPECIFIED.);
#1833=B_SPLINE_CURVE_WITH_KNOTS('',3,(#14436,#14437,#14438,#14439,#14440,
#14441,#14442,#14443,#14444,#14445),.UNSPECIFIED.,.F.,.F.,(4,1,1,1,1,1,
1,4),(34.5575191894876,35.3471398454185,36.3447112184015,37.3422825913844,
38.3398539643673,39.3374253373503,40.3349967103332,40.8407044966673),
 .UNSPECIFIED.);
#1834=B_SPLINE_CURVE_WITH_KNOTS('',3,(#14450,#14451,#14452,#14453,#14454,
#14455,#14456,#14457,#14458,#14459),.UNSPECIFIED.,.F.,.F.,(4,1,1,1,1,1,
1,4),(28.2743338823081,28.8202933449666,29.8178647179495,30.8154360909324,
31.8130074639154,32.8105788368983,33.8081502098812,34.5575191894876),
 .UNSPECIFIED.);
#1835=B_SPLINE_CURVE_WITH_KNOTS('',3,(#14460,#14461,#14462,#14463,#14464,
#14465,#14466,#14467,#14468,#14469,#14470),.UNSPECIFIED.,.F.,.F.,(4,1,1,
1,1,1,1,1,4),(28.2743338823081,28.364140234538,29.3617116075209,30.3592829805039,
31.3568543534868,32.3544257264697,33.3519970994527,34.3495684724356,34.5575191894876),
 .UNSPECIFIED.);
#1836=B_SPLINE_CURVE_WITH_KNOTS('',3,(#14475,#14476,#14477,#14478,#14479,
#14480,#14481,#14482,#14483,#14484),.UNSPECIFIED.,.F.,.F.,(4,1,1,1,1,1,
1,4),(21.9911485751285,22.8348651070689,23.8324364800519,24.8300078530348,
25.8275792260178,26.8251505990007,27.8227219719836,28.2743338823081),
 .UNSPECIFIED.);
#1837=B_SPLINE_CURVE_WITH_KNOTS('',3,(#14485,#14486,#14487,#14488,#14489,
#14490,#14491,#14492,#14493,#14494),.UNSPECIFIED.,.F.,.F.,(4,1,1,1,1,1,
1,4),(21.9911485751285,22.3787119966404,23.3762833696233,24.3738547426063,
25.3714261155892,26.3689974885721,27.3665688615551,28.2743338823081),
 .UNSPECIFIED.);
#1838=B_SPLINE_CURVE_WITH_KNOTS('',3,(#14500,#14501,#14502,#14503,#14504),
 .UNSPECIFIED.,.F.,.F.,(4,1,4),(14.3981410127769,15.3957123857599,15.7079632679489),
 .UNSPECIFIED.);
#1839=B_SPLINE_CURVE_WITH_KNOTS('',3,(#14507,#14508,#14509,#14510,#14511),
 .UNSPECIFIED.,.F.,.F.,(4,1,4),(13.8761928695312,14.8542941232055,15.7079632679489),
 .UNSPECIFIED.);
#1840=B_SPLINE_CURVE_WITH_KNOTS('',3,(#14517,#14518,#14519,#14520,#14521,
#14522,#14523,#14524,#14525,#14526,#14527,#14528,#14529,#14530,#14531,#14532,
#14533,#14534,#14535,#14536,#14537,#14538),.UNSPECIFIED.,.F.,.F.,(4,3,3,
3,3,3,3,4),(76.7080459413271,76.812995719686,77.8105670926689,78.8081384656519,
79.8057098386348,80.8032812116178,81.8008525846007,82.7984239575837),
 .UNSPECIFIED.);
#1841=B_SPLINE_CURVE_WITH_KNOTS('',3,(#14542,#14543,#14544,#14545,#14546,
#14547,#14548),.UNSPECIFIED.,.F.,.F.,(4,3,4),(-80.7838110923091,-79.8057098386348,
-79.2446069498473),.UNSPECIFIED.);
#1842=B_SPLINE_CURVE_WITH_KNOTS('',3,(#14552,#14553,#14554,#14555,#14556,
#14557,#14558,#14559,#14560,#14561,#14562,#14563,#14564,#14565,#14566,#14567,
#14568,#14569,#14570,#14571,#14572,#14573),.UNSPECIFIED.,.F.,.F.,(4,3,3,
3,3,3,3,4),(-79.2446069498473,-78.8081384656519,-77.8105670926689,-76.812995719686,
-75.815424346703,-74.8178529737201,-73.8202816007372,-72.9614216426678),
 .UNSPECIFIED.);
#1843=B_SPLINE_CURVE_WITH_KNOTS('',3,(#14578,#14579,#14580,#14581,#14582,
#14583,#14584,#14585,#14586,#14587,#14588,#14589,#14590,#14591,#14592,#14593,
#14594,#14595,#14596,#14597,#14598,#14599),.UNSPECIFIED.,.F.,.F.,(4,3,3,
3,3,3,3,4),(70.4248606341475,70.8275674817883,71.8251388547713,72.8227102277543,
73.8202816007372,74.8178529737201,75.815424346703,76.7080459413271),
 .UNSPECIFIED.);
#1844=B_SPLINE_CURVE_WITH_KNOTS('',3,(#14600,#14601,#14602,#14603,#14604,
#14605,#14606,#14607,#14608,#14609,#14610,#14611,#14612,#14613,#14614,#14615,
#14616,#14617,#14618,#14619,#14620,#14621,#14622,#14623,#14624),
 .UNSPECIFIED.,.F.,.F.,(4,3,3,3,3,3,3,3,4),(-72.9614216426678,-72.8227102277542,
-71.8251388547713,-70.8275674817884,-69.8299961088054,-68.8324247358225,
-67.8348533628396,-66.8372819898566,-66.6782363354882),.UNSPECIFIED.);
#1845=B_SPLINE_CURVE_WITH_KNOTS('',3,(#14629,#14630,#14631,#14632,#14633,
#14634,#14635,#14636,#14637,#14638,#14639,#14640,#14641,#14642,#14643,#14644,
#14645,#14646,#14647,#14648,#14649,#14650),.UNSPECIFIED.,.F.,.F.,(4,3,3,
3,3,3,3,4),(64.1416753269678,64.8421392438907,65.8397106168737,66.8372819898566,
67.8348533628396,68.8324247358225,69.8299961088054,70.4248606341475),
 .UNSPECIFIED.);
#1846=B_SPLINE_CURVE_WITH_KNOTS('',3,(#14651,#14652,#14653,#14654,#14655,
#14656,#14657,#14658,#14659,#14660,#14661,#14662,#14663,#14664,#14665,#14666,
#14667,#14668,#14669,#14670,#14671,#14672),.UNSPECIFIED.,.F.,.F.,(4,3,3,
3,3,3,3,4),(-66.6782363354882,-65.8397106168737,-64.8421392438908,-63.8445678709078,
-62.8469964979249,-61.849425124942,-60.851853751959,-60.3950510283085),
 .UNSPECIFIED.);
#1847=B_SPLINE_CURVE_WITH_KNOTS('',3,(#14677,#14678,#14679,#14680,#14681,
#14682,#14683,#14684,#14685,#14686,#14687,#14688,#14689,#14690,#14691,#14692,
#14693,#14694,#14695,#14696,#14697,#14698),.UNSPECIFIED.,.F.,.F.,(4,3,3,
3,3,3,3,4),(57.8584900197882,58.8567110059931,59.8542823789761,60.851853751959,
61.849425124942,62.8469964979249,63.8445678709078,64.1416753269678),
 .UNSPECIFIED.);
#1848=B_SPLINE_CURVE_WITH_KNOTS('',3,(#14699,#14700,#14701,#14702,#14703,
#14704,#14705,#14706,#14707,#14708,#14709,#14710,#14711,#14712,#14713,#14714,
#14715,#14716,#14717,#14718,#14719,#14720),.UNSPECIFIED.,.F.,.F.,(4,3,3,
3,3,3,3,4),(-60.3950510283085,-59.8542823789761,-58.8567110059932,-57.8591396330102,
-56.8615682600273,-55.8639968870443,-54.8664255140614,-54.1118657211289),
 .UNSPECIFIED.);
#1849=B_SPLINE_CURVE_WITH_KNOTS('',3,(#14725,#14726,#14727,#14728,#14729,
#14730,#14731,#14732,#14733,#14734,#14735,#14736,#14737,#14738,#14739,#14740,
#14741,#14742,#14743,#14744,#14745,#14746),.UNSPECIFIED.,.F.,.F.,(4,3,3,
3,3,3,3,4),(51.5753047126086,51.8737113951126,52.8712827680955,53.8688541410785,
54.8664255140614,55.8639968870444,56.8615682600273,57.8584900197882),
 .UNSPECIFIED.);
#1850=B_SPLINE_CURVE_WITH_KNOTS('',3,(#14747,#14748,#14749,#14750,#14751,
#14752,#14753,#14754,#14755,#14756,#14757,#14758,#14759,#14760,#14761,#14762,
#14763,#14764,#14765,#14766,#14767,#14768,#14769,#14770,#14771),
 .UNSPECIFIED.,.F.,.F.,(4,3,3,3,3,3,3,3,4),(-54.1118657211289,-53.8688541410785,
-52.8712827680955,-51.8737113951126,-50.8761400221297,-49.8785686491467,
-48.8809972761638,-47.8834259031809,-47.8286804139493),.UNSPECIFIED.);
#1851=B_SPLINE_CURVE_WITH_KNOTS('',3,(#14776,#14777,#14778,#14779,#14780,
#14781,#14782,#14783,#14784,#14785,#14786,#14787,#14788,#14789,#14790,#14791,
#14792,#14793,#14794,#14795,#14796,#14797),.UNSPECIFIED.,.F.,.F.,(4,3,3,
3,3,3,3,4),(45.2921194054291,45.888283157215,46.8858545301979,47.8834259031809,
48.8809972761638,49.8785686491467,50.8761400221297,51.5753047126086),
 .UNSPECIFIED.);
#1852=B_SPLINE_CURVE_WITH_KNOTS('',3,(#14798,#14799,#14800,#14801,#14802,
#14803,#14804,#14805,#14806,#14807,#14808,#14809,#14810,#14811,#14812,#14813,
#14814,#14815,#14816,#14817,#14818,#14819),.UNSPECIFIED.,.F.,.F.,(4,3,3,
3,3,3,3,4),(-47.8286804139493,-46.8858545301979,-45.888283157215,-44.8907117842321,
-43.8931404112491,-42.8955690382662,-41.8979976652833,-41.5454951067698),
 .UNSPECIFIED.);
#1853=B_SPLINE_CURVE_WITH_KNOTS('',3,(#14824,#14825,#14826,#14827,#14828,
#14829,#14830,#14831,#14832,#14833,#14834,#14835,#14836,#14837,#14838,#14839,
#14840,#14841,#14842,#14843,#14844,#14845),.UNSPECIFIED.,.F.,.F.,(4,3,3,
3,3,3,3,4),(39.0089340982495,39.9028549193174,40.9004262923003,41.8979976652833,
42.8955690382662,43.8931404112491,44.8907117842321,45.2921194054291),
 .UNSPECIFIED.);
#1854=B_SPLINE_CURVE_WITH_KNOTS('',3,(#14846,#14847,#14848,#14849,#14850,
#14851,#14852,#14853,#14854,#14855,#14856,#14857,#14858,#14859,#14860,#14861,
#14862,#14863,#14864,#14865,#14866,#14867),.UNSPECIFIED.,.F.,.F.,(4,3,3,
3,3,3,3,4),(-41.5454951067698,-40.9004262923003,-39.9028549193174,-38.9052835463345,
-37.9077121733515,-36.9101408003686,-35.9125694273856,-35.2623097995902),
 .UNSPECIFIED.);
#1855=B_SPLINE_CURVE_WITH_KNOTS('',3,(#14872,#14873,#14874,#14875,#14876,
#14877,#14878,#14879,#14880,#14881,#14882,#14883,#14884,#14885,#14886,#14887,
#14888,#14889,#14890,#14891,#14892,#14893,#14894,#14895,#14896),
 .UNSPECIFIED.,.F.,.F.,(4,3,3,3,3,3,3,3,4),(32.7257487910699,32.9198553084368,
33.9174266814198,34.9149980544027,35.9125694273856,36.9101408003686,37.9077121733515,
38.9052835463345,39.0089340982495),.UNSPECIFIED.);
#1856=B_SPLINE_CURVE_WITH_KNOTS('',3,(#14897,#14898,#14899,#14900,#14901,
#14902,#14903,#14904,#14905,#14906,#14907,#14908,#14909,#14910,#14911,#14912,
#14913,#14914,#14915,#14916,#14917,#14918),.UNSPECIFIED.,.F.,.F.,(4,3,3,
3,3,3,3,4),(-35.2623097995902,-34.9149980544027,-33.9174266814198,-32.9198553084368,
-31.9222839354539,-30.924712562471,-29.927141189488,-28.9791244924106),
 .UNSPECIFIED.);
#1857=B_SPLINE_CURVE_WITH_KNOTS('',3,(#14923,#14924,#14925,#14926,#14927,
#14928,#14929,#14930,#14931,#14932,#14933,#14934,#14935,#14936,#14937,#14938,
#14939,#14940,#14941,#14942,#14943,#14944),.UNSPECIFIED.,.F.,.F.,(4,3,3,
3,3,3,3,4),(26.4425634838903,26.9344270705392,27.9319984435222,28.9295698165051,
29.927141189488,30.924712562471,31.9222839354539,32.7257487910699),
 .UNSPECIFIED.);
#1858=B_SPLINE_CURVE_WITH_KNOTS('',3,(#14945,#14946,#14947,#14948,#14949,
#14950,#14951,#14952,#14953,#14954,#14955,#14956,#14957,#14958,#14959,#14960,
#14961,#14962,#14963,#14964,#14965,#14966,#14967,#14968,#14969),
 .UNSPECIFIED.,.F.,.F.,(4,3,3,3,3,3,3,3,4),(-28.9791244924106,-28.9295698165051,
-27.9319984435222,-26.9344270705392,-25.9368556975563,-24.9392843245734,
-23.9417129515904,-22.9441415786075,-22.695939185231),.UNSPECIFIED.);
#1859=B_SPLINE_CURVE_WITH_KNOTS('',3,(#14974,#14975,#14976,#14977,#14978,
#14979,#14980,#14981,#14982,#14983,#14984,#14985,#14986,#14987,#14988,#14989,
#14990,#14991,#14992,#14993,#14994,#14995),.UNSPECIFIED.,.F.,.F.,(4,3,3,
3,3,3,3,4),(20.1593781767107,20.9489988326416,21.9465702056246,22.9441415786075,
23.9417129515904,24.9392843245734,25.9368556975563,26.4425634838903),
 .UNSPECIFIED.);
#1860=B_SPLINE_CURVE_WITH_KNOTS('',3,(#14996,#14997,#14998,#14999,#15000,
#15001,#15002,#15003,#15004,#15005,#15006,#15007,#15008,#15009,#15010,#15011,
#15012,#15013,#15014,#15015,#15016,#15017),.UNSPECIFIED.,.F.,.F.,(4,3,3,
3,3,3,3,4),(-22.695939185231,-21.9465702056246,-20.9489988326416,-19.9514274596587,
-18.9538560866758,-17.9562847136928,-16.9587133407099,-16.4127538780514),
 .UNSPECIFIED.);
#1861=B_SPLINE_CURVE_WITH_KNOTS('',3,(#15022,#15023,#15024,#15025,#15026,
#15027,#15028,#15029,#15030,#15031,#15032,#15033,#15034,#15035,#15036,#15037,
#15038,#15039,#15040,#15041,#15042,#15043,#15044,#15045,#15046),
 .UNSPECIFIED.,.F.,.F.,(4,3,3,3,3,3,3,3,4),(13.8761928695311,13.9659992217611,
14.963570594744,15.961141967727,16.9587133407099,17.9562847136928,18.9538560866758,
19.9514274596587,20.1593781767107),.UNSPECIFIED.);
#1862=B_SPLINE_CURVE_WITH_KNOTS('',3,(#15047,#15048,#15049,#15050,#15051,
#15052,#15053,#15054,#15055,#15056,#15057,#15058,#15059,#15060,#15061,#15062,
#15063,#15064,#15065,#15066,#15067,#15068),.UNSPECIFIED.,.F.,.F.,(4,3,3,
3,3,3,3,4),(-16.4127538780514,-15.9611419677269,-14.963570594744,-13.9659992217611,
-12.9684278487781,-11.9708564757952,-10.9732851028123,-10.1295685708718),
 .UNSPECIFIED.);
#1863=B_SPLINE_CURVE_WITH_KNOTS('',3,(#15074,#15075,#15076,#15077,#15078,
#15079,#15080,#15081,#15082,#15083,#15084,#15085,#15086),.UNSPECIFIED.,
 .F.,.F.,(4,3,3,3,4),(-3.84638326369226,-2.9927141189488,-1.99514274596587,
-0.997571372982931,0.),.UNSPECIFIED.);
#1864=B_SPLINE_CURVE_WITH_KNOTS('',3,(#15089,#15090,#15091,#15092,#15093,
#15094,#15095,#15096,#15097,#15098,#15099,#15100,#15101,#15102,#15103,#15104,
#15105,#15106,#15107),.UNSPECIFIED.,.F.,.F.,(4,3,3,3,3,3,4),(2.01461286527457,
2.9927141189488,3.99028549193174,4.98785686491468,5.98542823789761,6.98299961088054,
7.59300756235157),.UNSPECIFIED.);
#1865=B_SPLINE_CURVE_WITH_KNOTS('',3,(#15113,#15114,#15115,#15116,#15117,
#15118,#15119),.UNSPECIFIED.,.F.,.F.,(4,1,1,1,4),(91.106186954104,91.6672898428915,
92.6648612158744,93.6624325888573,94.6600039618403),.UNSPECIFIED.);
#1866=B_SPLINE_CURVE_WITH_KNOTS('',3,(#15122,#15123,#15124,#15125,#15126,
#15127,#15128,#15129),.UNSPECIFIED.,.F.,.F.,(4,1,1,1,1,4),(91.106186954104,
91.2111367324629,92.2087081054458,93.2062794784288,94.2038508514117,95.181952105086),
 .UNSPECIFIED.);
#1867=B_SPLINE_CURVE_WITH_KNOTS('',3,(#15134,#15135,#15136,#15137,#15138,
#15139,#15140,#15141,#15142,#15143),.UNSPECIFIED.,.F.,.F.,(4,1,1,1,1,1,
1,4),(84.8230016469244,85.6818616049939,86.6794329779768,87.6770043509597,
88.6745757239427,89.6721470969256,90.6697184699085,91.106186954104),
 .UNSPECIFIED.);
#1868=B_SPLINE_CURVE_WITH_KNOTS('',3,(#15144,#15145,#15146,#15147,#15148,
#15149,#15150,#15151,#15152,#15153),.UNSPECIFIED.,.F.,.F.,(4,1,1,1,1,1,
1,4),(84.8230016469244,85.2257084945653,86.2232798675482,87.2208512405312,
88.2184226135141,89.215993986497,90.21356535948,91.106186954104),
 .UNSPECIFIED.);
#1869=B_SPLINE_CURVE_WITH_KNOTS('',3,(#15158,#15159,#15160,#15161,#15162,
#15163,#15164,#15165,#15166,#15167,#15168),.UNSPECIFIED.,.F.,.F.,(4,1,1,
1,1,1,1,1,4),(78.5398163397448,78.6988619941133,79.6964333670962,80.6940047400792,
81.6915761130621,82.689147486045,83.686718859028,84.6842902320109,84.8230016469244),
 .UNSPECIFIED.);
#1870=B_SPLINE_CURVE_WITH_KNOTS('',3,(#15169,#15170,#15171,#15172,#15173,
#15174,#15175,#15176,#15177,#15178),.UNSPECIFIED.,.F.,.F.,(4,1,1,1,1,1,
1,4),(78.5398163397448,79.2402802566677,80.2378516296506,81.2354230026336,
82.2329943756165,83.2305657485994,84.2281371215823,84.8230016469244),
 .UNSPECIFIED.);
#1871=B_SPLINE_CURVE_WITH_KNOTS('',3,(#15183,#15184,#15185,#15186,#15187,
#15188,#15189,#15190,#15191,#15192),.UNSPECIFIED.,.F.,.F.,(4,1,1,1,1,1,
1,4),(72.2566310325652,72.7134337562157,73.7110051291986,74.7085765021816,
75.7061478751645,76.7037192481474,77.7012906211304,78.5398163397448),
 .UNSPECIFIED.);
#1872=B_SPLINE_CURVE_WITH_KNOTS('',3,(#15193,#15194,#15195,#15196,#15197,
#15198,#15199,#15200,#15201,#15202,#15203),.UNSPECIFIED.,.F.,.F.,(4,1,1,
1,1,1,1,1,4),(72.2566310325652,72.2572806457871,73.2548520187701,74.252423391753,
75.2499947647359,76.2475661377189,77.2451375107018,78.2427088836847,78.5398163397448),
 .UNSPECIFIED.);
#1873=B_SPLINE_CURVE_WITH_KNOTS('',3,(#15208,#15209,#15210,#15211,#15212,
#15213,#15214,#15215,#15216,#15217),.UNSPECIFIED.,.F.,.F.,(4,1,1,1,1,1,
1,4),(65.9734457253856,66.7280055183181,67.725576891301,68.723148264284,
69.7207196372669,70.7182910102498,71.7158623832328,72.2566310325652),
 .UNSPECIFIED.);
#1874=B_SPLINE_CURVE_WITH_KNOTS('',3,(#15218,#15219,#15220,#15221,#15222,
#15223,#15224,#15225,#15226,#15227),.UNSPECIFIED.,.F.,.F.,(4,1,1,1,1,1,
1,4),(65.9734457253856,66.2718524078895,67.2694237808725,68.2669951538554,
69.2645665268383,70.2621378998213,71.2597092728042,72.2566310325652),
 .UNSPECIFIED.);
#1875=B_SPLINE_CURVE_WITH_KNOTS('',3,(#15232,#15233,#15234,#15235,#15236,
#15237,#15238,#15239,#15240,#15241,#15242),.UNSPECIFIED.,.F.,.F.,(4,1,1,
1,1,1,1,1,4),(59.690260418206,59.7450059074375,60.7425772804205,61.7401486534034,
62.7377200263864,63.7352913993693,64.7328627723522,65.7304341453352,65.9734457253856),
 .UNSPECIFIED.);
#1876=B_SPLINE_CURVE_WITH_KNOTS('',3,(#15243,#15244,#15245,#15246,#15247,
#15248,#15249,#15250,#15251,#15252),.UNSPECIFIED.,.F.,.F.,(4,1,1,1,1,1,
1,4),(59.690260418206,60.2864241699919,61.2839955429748,62.2815669159578,
63.2791382889407,64.2767096619237,65.2742810349066,65.9734457253856),
 .UNSPECIFIED.);
#1877=B_SPLINE_CURVE_WITH_KNOTS('',3,(#15257,#15258,#15259,#15260,#15261,
#15262,#15263,#15264,#15265,#15266),.UNSPECIFIED.,.F.,.F.,(4,1,1,1,1,1,
1,4),(53.4070751110264,53.7595776695399,54.7571490425229,55.7547204155058,
56.7522917884887,57.7498631614717,58.7474345344546,59.690260418206),
 .UNSPECIFIED.);
#1878=B_SPLINE_CURVE_WITH_KNOTS('',3,(#15267,#15268,#15269,#15270,#15271,
#15272,#15273,#15274,#15275,#15276),.UNSPECIFIED.,.F.,.F.,(4,1,1,1,1,1,
1,4),(53.4070751110264,54.3009959320943,55.2985673050772,56.2961386780602,
57.2937100510431,58.291281424026,59.288852797009,59.690260418206),
 .UNSPECIFIED.);
#1879=B_SPLINE_CURVE_WITH_KNOTS('',3,(#15281,#15282,#15283,#15284,#15285,
#15286,#15287,#15288,#15289,#15290),.UNSPECIFIED.,.F.,.F.,(4,1,1,1,1,1,
1,4),(47.1238898038469,47.7741494316423,48.7717208046253,49.7692921776082,
50.7668635505911,51.7644349235741,52.762006296557,53.4070751110264),
 .UNSPECIFIED.);
#1880=B_SPLINE_CURVE_WITH_KNOTS('',3,(#15291,#15292,#15293,#15294,#15295,
#15296,#15297,#15298,#15299,#15300,#15301),.UNSPECIFIED.,.F.,.F.,(4,1,1,
1,1,1,1,1,4),(47.1238898038469,47.3179963212138,48.3155676941967,49.3131390671796,
50.3107104401626,51.3082818131455,52.3058531861284,53.3034245591114,53.4070751110264),
 .UNSPECIFIED.);
#1881=B_SPLINE_CURVE_WITH_KNOTS('',3,(#15306,#15307,#15308,#15309,#15310,
#15311,#15312,#15313,#15314,#15315),.UNSPECIFIED.,.F.,.F.,(4,1,1,1,1,1,
1,4),(40.8407044966673,41.7887211937447,42.7862925667277,43.7838639397106,
44.7814353126935,45.7790066856765,46.7765780586594,47.1238898038469),
 .UNSPECIFIED.);
#1882=B_SPLINE_CURVE_WITH_KNOTS('',3,(#15316,#15317,#15318,#15319,#15320,
#15321,#15322,#15323,#15324,#15325),.UNSPECIFIED.,.F.,.F.,(4,1,1,1,1,1,
1,4),(40.8407044966673,41.3325680833162,42.3301394562991,43.327710829282,
44.325282202265,45.3228535752479,46.3204249482308,47.1238898038469),
 .UNSPECIFIED.);
#1883=B_SPLINE_CURVE_WITH_KNOTS('',3,(#15330,#15331,#15332,#15333,#15334,
#15335,#15336,#15337,#15338,#15339,#15340),.UNSPECIFIED.,.F.,.F.,(4,1,1,
1,1,1,1,1,4),(34.5575191894876,34.8057215828642,35.8032929558471,36.80086432883,
37.798435701813,38.7960070747959,39.7935784477789,40.7911498207618,40.8407044966673),
 .UNSPECIFIED.);
#1884=B_SPLINE_CURVE_WITH_KNOTS('',3,(#15341,#15342,#15343,#15344,#15345,
#15346,#15347,#15348,#15349,#15350),.UNSPECIFIED.,.F.,.F.,(4,1,1,1,1,1,
1,4),(34.5575191894876,35.3471398454185,36.3447112184015,37.3422825913844,
38.3398539643674,39.3374253373503,40.3349967103332,40.8407044966673),
 .UNSPECIFIED.);
#1885=B_SPLINE_CURVE_WITH_KNOTS('',3,(#15355,#15356,#15357,#15358,#15359,
#15360,#15361,#15362,#15363,#15364),.UNSPECIFIED.,.F.,.F.,(4,1,1,1,1,1,
1,4),(28.2743338823081,28.8202933449666,29.8178647179495,30.8154360909324,
31.8130074639154,32.8105788368983,33.8081502098812,34.5575191894876),
 .UNSPECIFIED.);
#1886=B_SPLINE_CURVE_WITH_KNOTS('',3,(#15365,#15366,#15367,#15368,#15369,
#15370,#15371,#15372,#15373,#15374,#15375),.UNSPECIFIED.,.F.,.F.,(4,1,1,
1,1,1,1,1,4),(28.2743338823081,28.364140234538,29.3617116075209,30.3592829805039,
31.3568543534868,32.3544257264697,33.3519970994527,34.3495684724356,34.5575191894876),
 .UNSPECIFIED.);
#1887=B_SPLINE_CURVE_WITH_KNOTS('',3,(#15380,#15381,#15382,#15383,#15384,
#15385,#15386,#15387,#15388,#15389),.UNSPECIFIED.,.F.,.F.,(4,1,1,1,1,1,
1,4),(21.9911485751285,22.834865107069,23.8324364800519,24.8300078530348,
25.8275792260178,26.8251505990007,27.8227219719836,28.2743338823081),
 .UNSPECIFIED.);
#1888=B_SPLINE_CURVE_WITH_KNOTS('',3,(#15390,#15391,#15392,#15393,#15394,
#15395,#15396,#15397,#15398,#15399),.UNSPECIFIED.,.F.,.F.,(4,1,1,1,1,1,
1,4),(21.9911485751285,22.3787119966404,23.3762833696233,24.3738547426063,
25.3714261155892,26.3689974885721,27.3665688615551,28.2743338823081),
 .UNSPECIFIED.);
#1889=B_SPLINE_CURVE_WITH_KNOTS('',3,(#15405,#15406,#15407,#15408,#15409),
 .UNSPECIFIED.,.F.,.F.,(4,1,4),(14.3981410127769,15.3957123857599,15.7079632679489),
 .UNSPECIFIED.);
#1890=B_SPLINE_CURVE_WITH_KNOTS('',3,(#15412,#15413,#15414,#15415,#15416),
 .UNSPECIFIED.,.F.,.F.,(4,1,4),(13.8761928695312,14.8542941232055,15.7079632679489),
 .UNSPECIFIED.);
#1891=B_SPLINE_CURVE_WITH_KNOTS('',3,(#15422,#15423,#15424,#15425,#15426,
#15427,#15428,#15429,#15430,#15431,#15432,#15433,#15434,#15435,#15436,#15437,
#15438,#15439,#15440,#15441,#15442,#15443),.UNSPECIFIED.,.F.,.F.,(4,3,3,
3,3,3,3,4),(76.708045941327,76.812995719686,77.8105670926689,78.8081384656519,
79.8057098386348,80.8032812116177,81.8008525846006,82.7984239575836),
 .UNSPECIFIED.);
#1892=B_SPLINE_CURVE_WITH_KNOTS('',3,(#15447,#15448,#15449,#15450,#15451,
#15452,#15453),.UNSPECIFIED.,.F.,.F.,(4,3,4),(-80.7838110923091,-79.8057098386348,
-79.2446069498473),.UNSPECIFIED.);
#1893=B_SPLINE_CURVE_WITH_KNOTS('',3,(#15457,#15458,#15459,#15460,#15461,
#15462,#15463,#15464,#15465,#15466,#15467,#15468,#15469,#15470,#15471,#15472,
#15473,#15474,#15475,#15476,#15477,#15478),.UNSPECIFIED.,.F.,.F.,(4,3,3,
3,3,3,3,4),(-79.2446069498473,-78.8081384656519,-77.8105670926689,-76.812995719686,
-75.815424346703,-74.8178529737201,-73.8202816007372,-72.9614216426678),
 .UNSPECIFIED.);
#1894=B_SPLINE_CURVE_WITH_KNOTS('',3,(#15483,#15484,#15485,#15486,#15487,
#15488,#15489,#15490,#15491,#15492,#15493,#15494,#15495,#15496,#15497,#15498,
#15499,#15500,#15501,#15502,#15503,#15504),.UNSPECIFIED.,.F.,.F.,(4,3,3,
3,3,3,3,4),(70.4248606341475,70.8275674817884,71.8251388547713,72.8227102277542,
73.8202816007372,74.8178529737201,75.815424346703,76.708045941327),
 .UNSPECIFIED.);
#1895=B_SPLINE_CURVE_WITH_KNOTS('',3,(#15505,#15506,#15507,#15508,#15509,
#15510,#15511,#15512,#15513,#15514,#15515,#15516,#15517,#15518,#15519,#15520,
#15521,#15522,#15523,#15524,#15525,#15526,#15527,#15528,#15529),
 .UNSPECIFIED.,.F.,.F.,(4,3,3,3,3,3,3,3,4),(-72.9614216426678,-72.8227102277542,
-71.8251388547713,-70.8275674817884,-69.8299961088054,-68.8324247358225,
-67.8348533628396,-66.8372819898566,-66.6782363354882),.UNSPECIFIED.);
#1896=B_SPLINE_CURVE_WITH_KNOTS('',3,(#15534,#15535,#15536,#15537,#15538,
#15539,#15540,#15541,#15542,#15543,#15544,#15545,#15546,#15547,#15548,#15549,
#15550,#15551,#15552,#15553,#15554,#15555),.UNSPECIFIED.,.F.,.F.,(4,3,3,
3,3,3,3,4),(64.1416753269678,64.8421392438907,65.8397106168737,66.8372819898566,
67.8348533628396,68.8324247358225,69.8299961088054,70.4248606341475),
 .UNSPECIFIED.);
#1897=B_SPLINE_CURVE_WITH_KNOTS('',3,(#15556,#15557,#15558,#15559,#15560,
#15561,#15562,#15563,#15564,#15565,#15566,#15567,#15568,#15569,#15570,#15571,
#15572,#15573,#15574,#15575,#15576,#15577),.UNSPECIFIED.,.F.,.F.,(4,3,3,
3,3,3,3,4),(-66.6782363354882,-65.8397106168737,-64.8421392438908,-63.8445678709078,
-62.8469964979249,-61.849425124942,-60.851853751959,-60.3950510283085),
 .UNSPECIFIED.);
#1898=B_SPLINE_CURVE_WITH_KNOTS('',3,(#15582,#15583,#15584,#15585,#15586,
#15587,#15588,#15589,#15590,#15591,#15592,#15593,#15594,#15595,#15596,#15597,
#15598,#15599,#15600,#15601,#15602,#15603),.UNSPECIFIED.,.F.,.F.,(4,3,3,
3,3,3,3,4),(57.8584900197882,58.8567110059932,59.8542823789761,60.851853751959,
61.849425124942,62.8469964979249,63.8445678709078,64.1416753269678),
 .UNSPECIFIED.);
#1899=B_SPLINE_CURVE_WITH_KNOTS('',3,(#15604,#15605,#15606,#15607,#15608,
#15609,#15610,#15611,#15612,#15613,#15614,#15615,#15616,#15617,#15618,#15619,
#15620,#15621,#15622,#15623,#15624,#15625),.UNSPECIFIED.,.F.,.F.,(4,3,3,
3,3,3,3,4),(-60.3950510283085,-59.8542823789761,-58.8567110059932,-57.8591396330102,
-56.8615682600273,-55.8639968870443,-54.8664255140614,-54.1118657211289),
 .UNSPECIFIED.);
#1900=B_SPLINE_CURVE_WITH_KNOTS('',3,(#15630,#15631,#15632,#15633,#15634,
#15635,#15636,#15637,#15638,#15639,#15640,#15641,#15642,#15643,#15644,#15645,
#15646,#15647,#15648,#15649,#15650,#15651),.UNSPECIFIED.,.F.,.F.,(4,3,3,
3,3,3,3,4),(51.5753047126087,51.8737113951126,52.8712827680955,53.8688541410785,
54.8664255140614,55.8639968870443,56.8615682600273,57.8584900197882),
 .UNSPECIFIED.);
#1901=B_SPLINE_CURVE_WITH_KNOTS('',3,(#15652,#15653,#15654,#15655,#15656,
#15657,#15658,#15659,#15660,#15661,#15662,#15663,#15664,#15665,#15666,#15667,
#15668,#15669,#15670,#15671,#15672,#15673,#15674,#15675,#15676),
 .UNSPECIFIED.,.F.,.F.,(4,3,3,3,3,3,3,3,4),(-54.1118657211289,-53.8688541410785,
-52.8712827680955,-51.8737113951126,-50.8761400221297,-49.8785686491467,
-48.8809972761638,-47.8834259031809,-47.8286804139493),.UNSPECIFIED.);
#1902=B_SPLINE_CURVE_WITH_KNOTS('',3,(#15681,#15682,#15683,#15684,#15685,
#15686,#15687,#15688,#15689,#15690,#15691,#15692,#15693,#15694,#15695,#15696,
#15697,#15698,#15699,#15700,#15701,#15702),.UNSPECIFIED.,.F.,.F.,(4,3,3,
3,3,3,3,4),(45.2921194054291,45.888283157215,46.8858545301979,47.8834259031809,
48.8809972761638,49.8785686491467,50.8761400221297,51.5753047126087),
 .UNSPECIFIED.);
#1903=B_SPLINE_CURVE_WITH_KNOTS('',3,(#15703,#15704,#15705,#15706,#15707,
#15708,#15709,#15710,#15711,#15712,#15713,#15714,#15715,#15716,#15717,#15718,
#15719,#15720,#15721,#15722,#15723,#15724),.UNSPECIFIED.,.F.,.F.,(4,3,3,
3,3,3,3,4),(-47.8286804139493,-46.8858545301979,-45.888283157215,-44.8907117842321,
-43.8931404112491,-42.8955690382662,-41.8979976652833,-41.5454951067698),
 .UNSPECIFIED.);
#1904=B_SPLINE_CURVE_WITH_KNOTS('',3,(#15729,#15730,#15731,#15732,#15733,
#15734,#15735,#15736,#15737,#15738,#15739,#15740,#15741,#15742,#15743,#15744,
#15745,#15746,#15747,#15748,#15749,#15750),.UNSPECIFIED.,.F.,.F.,(4,3,3,
3,3,3,3,4),(39.0089340982495,39.9028549193174,40.9004262923003,41.8979976652833,
42.8955690382662,43.8931404112491,44.8907117842321,45.2921194054291),
 .UNSPECIFIED.);
#1905=B_SPLINE_CURVE_WITH_KNOTS('',3,(#15751,#15752,#15753,#15754,#15755,
#15756,#15757,#15758,#15759,#15760,#15761,#15762,#15763,#15764,#15765,#15766,
#15767,#15768,#15769,#15770,#15771,#15772),.UNSPECIFIED.,.F.,.F.,(4,3,3,
3,3,3,3,4),(-41.5454951067698,-40.9004262923003,-39.9028549193174,-38.9052835463345,
-37.9077121733515,-36.9101408003686,-35.9125694273856,-35.2623097995902),
 .UNSPECIFIED.);
#1906=B_SPLINE_CURVE_WITH_KNOTS('',3,(#15777,#15778,#15779,#15780,#15781,
#15782,#15783,#15784,#15785,#15786,#15787,#15788,#15789,#15790,#15791,#15792,
#15793,#15794,#15795,#15796,#15797,#15798,#15799,#15800,#15801),
 .UNSPECIFIED.,.F.,.F.,(4,3,3,3,3,3,3,3,4),(32.7257487910699,32.9198553084369,
33.9174266814198,34.9149980544027,35.9125694273857,36.9101408003686,37.9077121733515,
38.9052835463345,39.0089340982495),.UNSPECIFIED.);
#1907=B_SPLINE_CURVE_WITH_KNOTS('',3,(#15802,#15803,#15804,#15805,#15806,
#15807,#15808,#15809,#15810,#15811,#15812,#15813,#15814,#15815,#15816,#15817,
#15818,#15819,#15820,#15821,#15822,#15823),.UNSPECIFIED.,.F.,.F.,(4,3,3,
3,3,3,3,4),(-35.2623097995902,-34.9149980544027,-33.9174266814198,-32.9198553084368,
-31.9222839354539,-30.924712562471,-29.927141189488,-28.9791244924106),
 .UNSPECIFIED.);
#1908=B_SPLINE_CURVE_WITH_KNOTS('',3,(#15828,#15829,#15830,#15831,#15832,
#15833,#15834,#15835,#15836,#15837,#15838,#15839,#15840,#15841,#15842,#15843,
#15844,#15845,#15846,#15847,#15848,#15849),.UNSPECIFIED.,.F.,.F.,(4,3,3,
3,3,3,3,4),(26.4425634838903,26.9344270705392,27.9319984435222,28.9295698165051,
29.927141189488,30.924712562471,31.9222839354539,32.7257487910699),
 .UNSPECIFIED.);
#1909=B_SPLINE_CURVE_WITH_KNOTS('',3,(#15850,#15851,#15852,#15853,#15854,
#15855,#15856,#15857,#15858,#15859,#15860,#15861,#15862,#15863,#15864,#15865,
#15866,#15867,#15868,#15869,#15870,#15871,#15872,#15873,#15874),
 .UNSPECIFIED.,.F.,.F.,(4,3,3,3,3,3,3,3,4),(-28.9791244924106,-28.9295698165051,
-27.9319984435222,-26.9344270705392,-25.9368556975563,-24.9392843245734,
-23.9417129515904,-22.9441415786075,-22.695939185231),.UNSPECIFIED.);
#1910=B_SPLINE_CURVE_WITH_KNOTS('',3,(#15879,#15880,#15881,#15882,#15883,
#15884,#15885,#15886,#15887,#15888,#15889,#15890,#15891,#15892,#15893,#15894,
#15895,#15896,#15897,#15898,#15899,#15900),.UNSPECIFIED.,.F.,.F.,(4,3,3,
3,3,3,3,4),(20.1593781767107,20.9489988326416,21.9465702056246,22.9441415786075,
23.9417129515904,24.9392843245734,25.9368556975563,26.4425634838903),
 .UNSPECIFIED.);
#1911=B_SPLINE_CURVE_WITH_KNOTS('',3,(#15901,#15902,#15903,#15904,#15905,
#15906,#15907,#15908,#15909,#15910,#15911,#15912,#15913,#15914,#15915,#15916,
#15917,#15918,#15919,#15920,#15921,#15922),.UNSPECIFIED.,.F.,.F.,(4,3,3,
3,3,3,3,4),(-22.695939185231,-21.9465702056246,-20.9489988326416,-19.9514274596587,
-18.9538560866758,-17.9562847136928,-16.9587133407099,-16.4127538780514),
 .UNSPECIFIED.);
#1912=B_SPLINE_CURVE_WITH_KNOTS('',3,(#15927,#15928,#15929,#15930,#15931,
#15932,#15933,#15934,#15935,#15936,#15937,#15938,#15939,#15940,#15941,#15942,
#15943,#15944,#15945,#15946,#15947,#15948,#15949,#15950,#15951),
 .UNSPECIFIED.,.F.,.F.,(4,3,3,3,3,3,3,3,4),(13.8761928695311,13.9659992217611,
14.963570594744,15.961141967727,16.9587133407099,17.9562847136928,18.9538560866758,
19.9514274596587,20.1593781767107),.UNSPECIFIED.);
#1913=B_SPLINE_CURVE_WITH_KNOTS('',3,(#15952,#15953,#15954,#15955,#15956,
#15957,#15958,#15959,#15960,#15961,#15962,#15963,#15964,#15965,#15966,#15967,
#15968,#15969,#15970,#15971,#15972,#15973),.UNSPECIFIED.,.F.,.F.,(4,3,3,
3,3,3,3,4),(-16.4127538780514,-15.961141967727,-14.963570594744,-13.9659992217611,
-12.9684278487782,-11.9708564757952,-10.9732851028123,-10.1295685708718),
 .UNSPECIFIED.);
#1914=B_SPLINE_CURVE_WITH_KNOTS('',3,(#15979,#15980,#15981,#15982,#15983,
#15984,#15985,#15986,#15987,#15988,#15989,#15990,#15991),.UNSPECIFIED.,
 .F.,.F.,(4,3,3,3,4),(-3.84638326369226,-2.9927141189488,-1.99514274596587,
-0.997571372982934,0.),.UNSPECIFIED.);
#1915=B_SPLINE_CURVE_WITH_KNOTS('',3,(#15994,#15995,#15996,#15997,#15998,
#15999,#16000,#16001,#16002,#16003,#16004,#16005,#16006,#16007,#16008,#16009,
#16010,#16011,#16012),.UNSPECIFIED.,.F.,.F.,(4,3,3,3,3,3,4),(2.01461286527449,
2.99271411894881,3.99028549193174,4.98785686491468,5.98542823789761,6.98299961088054,
7.59300756235157),.UNSPECIFIED.);
#1916=B_SPLINE_CURVE_WITH_KNOTS('',3,(#16018,#16019,#16020,#16021,#16022,
#16023,#16024),.UNSPECIFIED.,.F.,.F.,(4,1,1,1,4),(91.106186954104,91.6672898428915,
92.6648612158744,93.6624325888573,94.6600039618403),.UNSPECIFIED.);
#1917=B_SPLINE_CURVE_WITH_KNOTS('',3,(#16027,#16028,#16029,#16030,#16031,
#16032,#16033,#16034),.UNSPECIFIED.,.F.,.F.,(4,1,1,1,1,4),(91.106186954104,
91.2111367324629,92.2087081054458,93.2062794784288,94.2038508514117,95.181952105086),
 .UNSPECIFIED.);
#1918=B_SPLINE_CURVE_WITH_KNOTS('',3,(#16039,#16040,#16041,#16042,#16043,
#16044,#16045,#16046,#16047,#16048),.UNSPECIFIED.,.F.,.F.,(4,1,1,1,1,1,
1,4),(84.8230016469245,85.6818616049939,86.6794329779768,87.6770043509597,
88.6745757239427,89.6721470969256,90.6697184699085,91.106186954104),
 .UNSPECIFIED.);
#1919=B_SPLINE_CURVE_WITH_KNOTS('',3,(#16049,#16050,#16051,#16052,#16053,
#16054,#16055,#16056,#16057,#16058),.UNSPECIFIED.,.F.,.F.,(4,1,1,1,1,1,
1,4),(84.8230016469244,85.2257084945653,86.2232798675482,87.2208512405312,
88.2184226135141,89.215993986497,90.21356535948,91.106186954104),
 .UNSPECIFIED.);
#1920=B_SPLINE_CURVE_WITH_KNOTS('',3,(#16063,#16064,#16065,#16066,#16067,
#16068,#16069,#16070,#16071,#16072,#16073),.UNSPECIFIED.,.F.,.F.,(4,1,1,
1,1,1,1,1,4),(78.5398163397448,78.6988619941133,79.6964333670962,80.6940047400792,
81.6915761130621,82.689147486045,83.686718859028,84.6842902320109,84.8230016469245),
 .UNSPECIFIED.);
#1921=B_SPLINE_CURVE_WITH_KNOTS('',3,(#16074,#16075,#16076,#16077,#16078,
#16079,#16080,#16081,#16082,#16083),.UNSPECIFIED.,.F.,.F.,(4,1,1,1,1,1,
1,4),(78.5398163397448,79.2402802566677,80.2378516296506,81.2354230026336,
82.2329943756165,83.2305657485994,84.2281371215823,84.8230016469244),
 .UNSPECIFIED.);
#1922=B_SPLINE_CURVE_WITH_KNOTS('',3,(#16088,#16089,#16090,#16091,#16092,
#16093,#16094,#16095,#16096,#16097),.UNSPECIFIED.,.F.,.F.,(4,1,1,1,1,1,
1,4),(72.2566310325652,72.7134337562157,73.7110051291986,74.7085765021816,
75.7061478751645,76.7037192481474,77.7012906211304,78.5398163397448),
 .UNSPECIFIED.);
#1923=B_SPLINE_CURVE_WITH_KNOTS('',3,(#16098,#16099,#16100,#16101,#16102,
#16103,#16104,#16105,#16106,#16107,#16108),.UNSPECIFIED.,.F.,.F.,(4,1,1,
1,1,1,1,1,4),(72.2566310325652,72.2572806457871,73.2548520187701,74.252423391753,
75.2499947647359,76.2475661377189,77.2451375107018,78.2427088836847,78.5398163397448),
 .UNSPECIFIED.);
#1924=B_SPLINE_CURVE_WITH_KNOTS('',3,(#16113,#16114,#16115,#16116,#16117,
#16118,#16119,#16120,#16121,#16122),.UNSPECIFIED.,.F.,.F.,(4,1,1,1,1,1,
1,4),(65.9734457253856,66.7280055183181,67.725576891301,68.723148264284,
69.7207196372669,70.7182910102498,71.7158623832328,72.2566310325652),
 .UNSPECIFIED.);
#1925=B_SPLINE_CURVE_WITH_KNOTS('',3,(#16123,#16124,#16125,#16126,#16127,
#16128,#16129,#16130,#16131,#16132),.UNSPECIFIED.,.F.,.F.,(4,1,1,1,1,1,
1,4),(65.9734457253856,66.2718524078895,67.2694237808725,68.2669951538554,
69.2645665268383,70.2621378998213,71.2597092728042,72.2566310325652),
 .UNSPECIFIED.);
#1926=B_SPLINE_CURVE_WITH_KNOTS('',3,(#16137,#16138,#16139,#16140,#16141,
#16142,#16143,#16144,#16145,#16146,#16147),.UNSPECIFIED.,.F.,.F.,(4,1,1,
1,1,1,1,1,4),(59.690260418206,59.7450059074375,60.7425772804205,61.7401486534034,
62.7377200263864,63.7352913993693,64.7328627723522,65.7304341453352,65.9734457253856),
 .UNSPECIFIED.);
#1927=B_SPLINE_CURVE_WITH_KNOTS('',3,(#16148,#16149,#16150,#16151,#16152,
#16153,#16154,#16155,#16156,#16157),.UNSPECIFIED.,.F.,.F.,(4,1,1,1,1,1,
1,4),(59.690260418206,60.2864241699919,61.2839955429748,62.2815669159578,
63.2791382889407,64.2767096619236,65.2742810349066,65.9734457253856),
 .UNSPECIFIED.);
#1928=B_SPLINE_CURVE_WITH_KNOTS('',3,(#16162,#16163,#16164,#16165,#16166,
#16167,#16168,#16169,#16170,#16171),.UNSPECIFIED.,.F.,.F.,(4,1,1,1,1,1,
1,4),(53.4070751110265,53.7595776695399,54.7571490425229,55.7547204155058,
56.7522917884887,57.7498631614717,58.7474345344546,59.690260418206),
 .UNSPECIFIED.);
#1929=B_SPLINE_CURVE_WITH_KNOTS('',3,(#16172,#16173,#16174,#16175,#16176,
#16177,#16178,#16179,#16180,#16181),.UNSPECIFIED.,.F.,.F.,(4,1,1,1,1,1,
1,4),(53.4070751110264,54.3009959320943,55.2985673050772,56.2961386780602,
57.2937100510431,58.291281424026,59.288852797009,59.690260418206),
 .UNSPECIFIED.);
#1930=B_SPLINE_CURVE_WITH_KNOTS('',3,(#16186,#16187,#16188,#16189,#16190,
#16191,#16192,#16193,#16194,#16195),.UNSPECIFIED.,.F.,.F.,(4,1,1,1,1,1,
1,4),(47.1238898038469,47.7741494316423,48.7717208046253,49.7692921776082,
50.7668635505911,51.7644349235741,52.762006296557,53.4070751110265),
 .UNSPECIFIED.);
#1931=B_SPLINE_CURVE_WITH_KNOTS('',3,(#16196,#16197,#16198,#16199,#16200,
#16201,#16202,#16203,#16204,#16205,#16206),.UNSPECIFIED.,.F.,.F.,(4,1,1,
1,1,1,1,1,4),(47.1238898038469,47.3179963212138,48.3155676941967,49.3131390671796,
50.3107104401626,51.3082818131455,52.3058531861284,53.3034245591114,53.4070751110264),
 .UNSPECIFIED.);
#1932=B_SPLINE_CURVE_WITH_KNOTS('',3,(#16211,#16212,#16213,#16214,#16215,
#16216,#16217,#16218,#16219,#16220),.UNSPECIFIED.,.F.,.F.,(4,1,1,1,1,1,
1,4),(40.8407044966673,41.7887211937447,42.7862925667277,43.7838639397106,
44.7814353126935,45.7790066856765,46.7765780586594,47.1238898038469),
 .UNSPECIFIED.);
#1933=B_SPLINE_CURVE_WITH_KNOTS('',3,(#16221,#16222,#16223,#16224,#16225,
#16226,#16227,#16228,#16229,#16230),.UNSPECIFIED.,.F.,.F.,(4,1,1,1,1,1,
1,4),(40.8407044966673,41.3325680833162,42.3301394562991,43.327710829282,
44.325282202265,45.3228535752479,46.3204249482308,47.1238898038469),
 .UNSPECIFIED.);
#1934=B_SPLINE_CURVE_WITH_KNOTS('',3,(#16235,#16236,#16237,#16238,#16239,
#16240,#16241,#16242,#16243,#16244,#16245),.UNSPECIFIED.,.F.,.F.,(4,1,1,
1,1,1,1,1,4),(34.5575191894876,34.8057215828642,35.8032929558471,36.80086432883,
37.798435701813,38.7960070747959,39.7935784477789,40.7911498207618,40.8407044966673),
 .UNSPECIFIED.);
#1935=B_SPLINE_CURVE_WITH_KNOTS('',3,(#16246,#16247,#16248,#16249,#16250,
#16251,#16252,#16253,#16254,#16255),.UNSPECIFIED.,.F.,.F.,(4,1,1,1,1,1,
1,4),(34.5575191894876,35.3471398454185,36.3447112184015,37.3422825913844,
38.3398539643674,39.3374253373503,40.3349967103332,40.8407044966673),
 .UNSPECIFIED.);
#1936=B_SPLINE_CURVE_WITH_KNOTS('',3,(#16260,#16261,#16262,#16263,#16264,
#16265,#16266,#16267,#16268,#16269),.UNSPECIFIED.,.F.,.F.,(4,1,1,1,1,1,
1,4),(28.2743338823081,28.8202933449666,29.8178647179495,30.8154360909324,
31.8130074639154,32.8105788368983,33.8081502098812,34.5575191894876),
 .UNSPECIFIED.);
#1937=B_SPLINE_CURVE_WITH_KNOTS('',3,(#16270,#16271,#16272,#16273,#16274,
#16275,#16276,#16277,#16278,#16279,#16280),.UNSPECIFIED.,.F.,.F.,(4,1,1,
1,1,1,1,1,4),(28.2743338823081,28.364140234538,29.3617116075209,30.3592829805039,
31.3568543534868,32.3544257264697,33.3519970994527,34.3495684724356,34.5575191894876),
 .UNSPECIFIED.);
#1938=B_SPLINE_CURVE_WITH_KNOTS('',3,(#16285,#16286,#16287,#16288,#16289,
#16290,#16291,#16292,#16293,#16294),.UNSPECIFIED.,.F.,.F.,(4,1,1,1,1,1,
1,4),(21.9911485751285,22.834865107069,23.8324364800519,24.8300078530348,
25.8275792260178,26.8251505990007,27.8227219719836,28.2743338823081),
 .UNSPECIFIED.);
#1939=B_SPLINE_CURVE_WITH_KNOTS('',3,(#16295,#16296,#16297,#16298,#16299,
#16300,#16301,#16302,#16303,#16304),.UNSPECIFIED.,.F.,.F.,(4,1,1,1,1,1,
1,4),(21.9911485751285,22.3787119966404,23.3762833696233,24.3738547426063,
25.3714261155892,26.3689974885721,27.3665688615551,28.2743338823081),
 .UNSPECIFIED.);
#1940=B_SPLINE_CURVE_WITH_KNOTS('',3,(#16310,#16311,#16312,#16313,#16314),
 .UNSPECIFIED.,.F.,.F.,(4,1,4),(14.3981410127769,15.3957123857599,15.7079632679489),
 .UNSPECIFIED.);
#1941=B_SPLINE_CURVE_WITH_KNOTS('',3,(#16317,#16318,#16319,#16320,#16321),
 .UNSPECIFIED.,.F.,.F.,(4,1,4),(13.8761928695312,14.8542941232055,15.7079632679489),
 .UNSPECIFIED.);
#1942=B_SPLINE_CURVE_WITH_KNOTS('',3,(#16404,#16405,#16406,#16407,#16408,
#16409,#16410,#16411,#16412,#16413,#16414,#16415,#16416,#16417,#16418,#16419,
#16420,#16421,#16422,#16423,#16424,#16425,#16426,#16427,#16428,#16429,#16430,
#16431,#16432,#16433,#16434,#16435,#16436,#16437,#16438,#16439,#16440,#16441,
#16442,#16443,#16444,#16445,#16446,#16447,#16448,#16449,#16450,#16451,#16452,
#16453,#16454,#16455,#16456,#16457,#16458),.UNSPECIFIED.,.F.,.F.,(4,3,3,
3,3,3,3,3,3,3,3,3,3,3,3,3,3,3,4),(-0.378621596831442,-0.353562246097462,
-0.339726792951542,-0.324795397581524,-0.299967980662127,-0.289118724731059,
-0.252370044287308,-0.234474300298533,-0.219335629396853,-0.200829495678085,
-0.174827324623006,-0.15584693665932,-0.144923737522316,-0.109696956092963,
-0.0896699638623999,-0.0773387259299598,-0.0372142298588392,-0.00401661180490446,
0.),.UNSPECIFIED.);
#1943=B_SPLINE_CURVE_WITH_KNOTS('',3,(#16459,#16460,#16461,#16462,#16463,
#16464,#16465,#16466,#16467,#16468,#16469,#16470,#16471,#16472,#16473,#16474,
#16475,#16476,#16477,#16478,#16479,#16480,#16481,#16482,#16483,#16484,#16485,
#16486,#16487,#16488,#16489,#16490,#16491,#16492,#16493,#16494,#16495,#16496,
#16497,#16498,#16499,#16500,#16501,#16502,#16503,#16504,#16505,#16506,#16507,
#16508,#16509,#16510,#16511,#16512,#16513),.UNSPECIFIED.,.F.,.F.,(4,3,3,
3,3,3,3,3,3,3,3,3,3,3,3,3,3,3,4),(-0.376940817211619,-0.351602437043448,
-0.332519408379845,-0.318228058131088,-0.288333449384516,-0.272718117105765,
-0.234505377427356,-0.216962131374135,-0.205493408420767,-0.180854828870943,
-0.153734180151122,-0.136643041471865,-0.126205700111191,-0.0954718773410078,
-0.0666269097764766,-0.0558557551097461,-0.0219614248579871,-0.00327040903045905,
0.),.UNSPECIFIED.);
#1944=B_SPLINE_CURVE_WITH_KNOTS('',3,(#16515,#16516,#16517,#16518,#16519,
#16520,#16521,#16522,#16523,#16524,#16525),.UNSPECIFIED.,.F.,.F.,(4,1,1,
1,1,1,1,1,4),(15.7079632679489,15.8518654961884,16.8494368691714,17.8470082421543,
18.8445796151372,19.8421509881202,20.8397223611031,21.837293734086,21.9911485751285),
 .UNSPECIFIED.);
#1945=B_SPLINE_CURVE_WITH_KNOTS('',3,(#16526,#16527,#16528,#16529,#16530,
#16531,#16532,#16533,#16534,#16535),.UNSPECIFIED.,.F.,.F.,(4,1,1,1,1,1,
1,4),(15.7079632679489,16.3932837587428,17.3908551317257,18.3884265047087,
19.3859978776916,20.3835692506745,21.3811406236575,21.9911485751285),
 .UNSPECIFIED.);
#1946=B_SPLINE_CURVE_WITH_KNOTS('',3,(#16880,#16881,#16882,#16883,#16884,
#16885,#16886,#16887,#16888,#16889,#16890,#16891,#16892,#16893,#16894,#16895,
#16896,#16897,#16898,#16899,#16900,#16901,#16902,#16903,#16904,#16905,#16906,
#16907,#16908,#16909,#16910,#16911,#16912,#16913,#16914,#16915,#16916,#16917,
#16918,#16919,#16920,#16921,#16922,#16923,#16924,#16925,#16926,#16927,#16928,
#16929,#16930,#16931),.UNSPECIFIED.,.F.,.F.,(4,3,3,3,3,3,3,3,3,3,3,3,3,
3,3,3,3,4),(0.,0.0336910847235707,0.0587346654534766,0.0734852364994148,
0.109792238871862,0.132864830837164,0.143632030356024,0.17720525627004,
0.195911997060402,0.20761397219,0.244895171883038,0.269599304636634,0.282507756557061,
0.310158174405463,0.327757797512771,0.342580165552076,0.372940760482292,
0.376940817211643),.UNSPECIFIED.);
#1947=B_SPLINE_CURVE_WITH_KNOTS('',3,(#16932,#16933,#16934,#16935,#16936,
#16937,#16938,#16939,#16940,#16941,#16942,#16943,#16944,#16945,#16946,#16947,
#16948,#16949,#16950,#16951,#16952,#16953,#16954,#16955,#16956),
 .UNSPECIFIED.,.F.,.F.,(4,3,3,3,3,3,3,3,4),(-10.1295685708718,-9.97571372982935,
-8.97814235684642,-7.98057098386348,-6.98299961088054,-5.98542823789761,
-4.98785686491468,-3.99028549193174,-3.84638326369226),.UNSPECIFIED.);
#1948=B_SPLINE_CURVE_WITH_KNOTS('',3,(#17301,#17302,#17303,#17304,#17305,
#17306,#17307,#17308,#17309,#17310,#17311,#17312,#17313,#17314,#17315,#17316,
#17317,#17318,#17319,#17320,#17321,#17322),.UNSPECIFIED.,.F.,.F.,(4,3,3,
3,3,3,3,4),(7.59300756235157,7.98057098386348,8.97814235684642,9.97571372982935,
10.9732851028123,11.9708564757952,12.9684278487781,13.8761928695311),
 .UNSPECIFIED.);
#1949=B_SPLINE_CURVE_WITH_KNOTS('',3,(#17323,#17324,#17325,#17326,#17327,
#17328,#17329,#17330,#17331,#17332,#17333,#17334,#17335,#17336,#17337,#17338,
#17339,#17340,#17341,#17342,#17343,#17344,#17345,#17346,#17347,#17348,#17349,
#17350,#17351,#17352,#17353,#17354,#17355,#17356,#17357,#17358,#17359,#17360,
#17361,#17362,#17363,#17364,#17365,#17366,#17367,#17368,#17369,#17370,#17371,
#17372,#17373,#17374),.UNSPECIFIED.,.F.,.F.,(4,3,3,3,3,3,3,3,3,3,3,3,3,
3,3,3,3,4),(0.,0.039679134584082,0.0597937574063347,0.077198275206118,0.0898304469160062,
0.128492621633409,0.153526594220962,0.165101500237275,0.197163594226419,
0.224452129979101,0.234160526966568,0.26945519714964,0.287578609071477,
0.305421511169844,0.333081607138838,0.347224899232131,0.375339207698859,
0.378621596831424),.UNSPECIFIED.);
#1950=B_SPLINE_CURVE_WITH_KNOTS('',3,(#17377,#17378,#17379,#17380,#17381,
#17382,#17383,#17384,#17385,#17386,#17387,#17388,#17389,#17390,#17391,#17392,
#17393,#17394,#17395,#17396,#17397,#17398,#17399,#17400,#17401,#17402,#17403,
#17404,#17405,#17406,#17407,#17408,#17409,#17410,#17411,#17412,#17413,#17414,
#17415,#17416,#17417,#17418,#17419,#17420,#17421,#17422,#17423,#17424,#17425,
#17426,#17427,#17428,#17429,#17430,#17431),.UNSPECIFIED.,.F.,.F.,(4,3,3,
3,3,3,3,3,3,3,3,3,3,3,3,3,3,3,4),(-0.378621596831443,-0.353562246091994,
-0.33972679327765,-0.324795398102486,-0.29996799510237,-0.289118738473772,
-0.252370061457217,-0.234474320899414,-0.219335629080767,-0.200829495678084,
-0.174827314232915,-0.155846896352443,-0.144923681945981,-0.109696914410712,
-0.0896698834676189,-0.0773386968783234,-0.0372142012245099,-0.00401661180490457,
0.),.UNSPECIFIED.);
#1951=B_SPLINE_CURVE_WITH_KNOTS('',3,(#17432,#17433,#17434,#17435,#17436,
#17437,#17438,#17439,#17440,#17441,#17442,#17443,#17444,#17445,#17446,#17447,
#17448,#17449,#17450,#17451,#17452,#17453,#17454,#17455,#17456,#17457,#17458,
#17459,#17460,#17461,#17462,#17463,#17464,#17465,#17466,#17467,#17468,#17469,
#17470,#17471,#17472,#17473,#17474,#17475,#17476,#17477,#17478,#17479,#17480,
#17481,#17482,#17483,#17484,#17485,#17486),.UNSPECIFIED.,.F.,.F.,(4,3,3,
3,3,3,3,3,3,3,3,3,3,3,3,3,3,3,4),(-0.376940817211611,-0.351602437357937,
-0.332519414484987,-0.318228064219006,-0.288333486347302,-0.272718127906801,
-0.234505384447309,-0.21696214863526,-0.205493420723107,-0.180854828870948,
-0.153734168647042,-0.136642926650914,-0.126205451446247,-0.0954716908423004,
-0.0666266083256078,-0.0558556962658209,-0.0219613612575045,-0.00327040903046154,
0.),.UNSPECIFIED.);
#1952=B_SPLINE_CURVE_WITH_KNOTS('',3,(#17488,#17489,#17490,#17491,#17492,
#17493,#17494,#17495,#17496,#17497,#17498),.UNSPECIFIED.,.F.,.F.,(4,1,1,
1,1,1,1,1,4),(15.7079632679489,15.8518654961884,16.8494368691714,17.8470082421543,
18.8445796151372,19.8421509881202,20.8397223611031,21.837293734086,21.9911485751285),
 .UNSPECIFIED.);
#1953=B_SPLINE_CURVE_WITH_KNOTS('',3,(#17499,#17500,#17501,#17502,#17503,
#17504,#17505,#17506,#17507,#17508),.UNSPECIFIED.,.F.,.F.,(4,1,1,1,1,1,
1,4),(15.7079632679489,16.3932837587428,17.3908551317257,18.3884265047087,
19.3859978776916,20.3835692506745,21.3811406236575,21.9911485751285),
 .UNSPECIFIED.);
#1954=B_SPLINE_CURVE_WITH_KNOTS('',3,(#17853,#17854,#17855,#17856,#17857,
#17858,#17859,#17860,#17861,#17862,#17863,#17864,#17865,#17866,#17867,#17868,
#17869,#17870,#17871,#17872,#17873,#17874,#17875,#17876,#17877,#17878,#17879,
#17880,#17881,#17882,#17883,#17884,#17885,#17886,#17887,#17888,#17889,#17890,
#17891,#17892,#17893,#17894,#17895,#17896,#17897,#17898,#17899,#17900,#17901,
#17902,#17903,#17904),.UNSPECIFIED.,.F.,.F.,(4,3,3,3,3,3,3,3,3,3,3,3,3,
3,3,3,3,4),(0.,0.0336910719722371,0.0587346603191241,0.0734852357557152,
0.109792234187795,0.132864822139093,0.143632015204812,0.177205256270034,
0.195911998811098,0.207613973107216,0.244895181060382,0.269599327917347,
0.282507776228681,0.310158203547799,0.327758105582494,0.342580213444175,
0.372940760482282,0.376940817211633),.UNSPECIFIED.);
#1955=B_SPLINE_CURVE_WITH_KNOTS('',3,(#17905,#17906,#17907,#17908,#17909,
#17910,#17911,#17912,#17913,#17914,#17915,#17916,#17917,#17918,#17919,#17920,
#17921,#17922,#17923,#17924,#17925,#17926,#17927,#17928,#17929),
 .UNSPECIFIED.,.F.,.F.,(4,3,3,3,3,3,3,3,4),(-10.1295685708718,-9.97571372982935,
-8.97814235684641,-7.98057098386348,-6.98299961088054,-5.98542823789761,
-4.98785686491467,-3.99028549193174,-3.84638326369226),.UNSPECIFIED.);
#1956=B_SPLINE_CURVE_WITH_KNOTS('',3,(#18274,#18275,#18276,#18277,#18278,
#18279,#18280,#18281,#18282,#18283,#18284,#18285,#18286,#18287,#18288,#18289,
#18290,#18291,#18292,#18293,#18294,#18295),.UNSPECIFIED.,.F.,.F.,(4,3,3,
3,3,3,3,4),(7.59300756235157,7.98057098386348,8.97814235684641,9.97571372982935,
10.9732851028123,11.9708564757952,12.9684278487782,13.8761928695311),
 .UNSPECIFIED.);
#1957=B_SPLINE_CURVE_WITH_KNOTS('',3,(#18296,#18297,#18298,#18299,#18300,
#18301,#18302,#18303,#18304,#18305,#18306,#18307,#18308,#18309,#18310,#18311,
#18312,#18313,#18314,#18315,#18316,#18317,#18318,#18319,#18320,#18321,#18322,
#18323,#18324,#18325,#18326,#18327,#18328,#18329,#18330,#18331,#18332,#18333,
#18334,#18335,#18336,#18337,#18338,#18339,#18340,#18341,#18342,#18343,#18344,
#18345,#18346,#18347),.UNSPECIFIED.,.F.,.F.,(4,3,3,3,3,3,3,3,3,3,3,3,3,
3,3,3,3,4),(0.,0.0396791274481056,0.0597937021224953,0.0771976680457239,
0.0898303082602208,0.12849248988162,0.15352646947755,0.165101472375799,
0.197163594226428,0.224452133325792,0.23416053148377,0.269455200537544,
0.287578557392714,0.305421521052156,0.333081636597174,0.347224904045167,
0.375339207698866,0.378621596831432),.UNSPECIFIED.);
#1958=B_SPLINE_CURVE_WITH_KNOTS('',3,(#18350,#18351,#18352,#18353,#18354,
#18355,#18356,#18357,#18358,#18359,#18360,#18361,#18362,#18363,#18364,#18365,
#18366,#18367,#18368,#18369,#18370,#18371,#18372,#18373,#18374,#18375,#18376,
#18377,#18378,#18379,#18380,#18381,#18382,#18383,#18384,#18385,#18386,#18387,
#18388,#18389,#18390,#18391,#18392,#18393,#18394,#18395,#18396,#18397,#18398,
#18399,#18400,#18401,#18402,#18403,#18404),.UNSPECIFIED.,.F.,.F.,(4,3,3,
3,3,3,3,3,3,3,3,3,3,3,3,3,3,3,4),(-0.378621596831421,-0.353562246109156,
-0.3397267922352,-0.324795396410533,-0.299967947923947,-0.289118693566506,
-0.252370005353849,-0.234474253593686,-0.219335630122499,-0.200829495678059,
-0.174827348196324,-0.155847028127452,-0.144923863657138,-0.109697050694078,
-0.089670146324546,-0.0773387918294275,-0.0372142948109077,-0.00401661180489871,
0.),.UNSPECIFIED.);
#1959=B_SPLINE_CURVE_WITH_KNOTS('',3,(#18405,#18406,#18407,#18408,#18409,
#18410,#18411,#18412,#18413,#18414,#18415,#18416,#18417,#18418,#18419,#18420,
#18421,#18422,#18423,#18424,#18425,#18426,#18427,#18428,#18429,#18430,#18431,
#18432,#18433,#18434,#18435,#18436,#18437,#18438,#18439,#18440,#18441,#18442,
#18443,#18444,#18445,#18446,#18447,#18448,#18449,#18450,#18451,#18452,#18453,
#18454,#18455,#18456,#18457,#18458,#18459),.UNSPECIFIED.,.F.,.F.,(4,3,3,
3,3,3,3,3,3,3,3,3,3,3,3,3,3,3,4),(-0.376940817211661,-0.351602437644044,
-0.332519420023622,-0.318228069756221,-0.288333520013757,-0.272718137738777,
-0.234505390822111,-0.216962164313794,-0.205493431901863,-0.180854828870961,
-0.15373415812608,-0.13664282164838,-0.126205224016848,-0.0954715202702509,
-0.0666263326168646,-0.0558556424387309,-0.0219613030816618,-0.00327040903045922,
0.),.UNSPECIFIED.);
#1960=B_SPLINE_CURVE_WITH_KNOTS('',3,(#18461,#18462,#18463,#18464,#18465,
#18466,#18467,#18468,#18469,#18470,#18471),.UNSPECIFIED.,.F.,.F.,(4,1,1,
1,1,1,1,1,4),(15.7079632679489,15.8518654961884,16.8494368691713,17.8470082421543,
18.8445796151372,19.8421509881201,20.8397223611031,21.837293734086,21.9911485751285),
 .UNSPECIFIED.);
#1961=B_SPLINE_CURVE_WITH_KNOTS('',3,(#18472,#18473,#18474,#18475,#18476,
#18477,#18478,#18479,#18480,#18481),.UNSPECIFIED.,.F.,.F.,(4,1,1,1,1,1,
1,4),(15.7079632679489,16.3932837587428,17.3908551317257,18.3884265047087,
19.3859978776916,20.3835692506745,21.3811406236575,21.9911485751285),
 .UNSPECIFIED.);
#1962=B_SPLINE_CURVE_WITH_KNOTS('',3,(#18826,#18827,#18828,#18829,#18830,
#18831,#18832,#18833,#18834,#18835,#18836,#18837,#18838,#18839,#18840,#18841,
#18842,#18843,#18844,#18845,#18846,#18847,#18848,#18849,#18850,#18851,#18852,
#18853,#18854,#18855,#18856,#18857,#18858,#18859,#18860,#18861,#18862,#18863,
#18864,#18865,#18866,#18867,#18868,#18869,#18870,#18871,#18872,#18873,#18874,
#18875,#18876,#18877),.UNSPECIFIED.,.F.,.F.,(4,3,3,3,3,3,3,3,3,3,3,3,3,
3,3,3,3,4),(0.,0.0336910603093437,0.0587346556237836,0.0734852350726252,
0.109792229900142,0.132864814179886,0.143632001341265,0.177205256270027,
0.195912000411831,0.207613973950097,0.244895189457593,0.269599349217699,
0.282507794231336,0.310158230215905,0.327758387489592,0.342580257274108,
0.372940760482283,0.376940817211633),.UNSPECIFIED.);
#1963=B_SPLINE_CURVE_WITH_KNOTS('',3,(#18878,#18879,#18880,#18881,#18882,
#18883,#18884,#18885,#18886,#18887,#18888,#18889,#18890,#18891,#18892,#18893,
#18894,#18895,#18896,#18897,#18898,#18899,#18900,#18901,#18902),
 .UNSPECIFIED.,.F.,.F.,(4,3,3,3,3,3,3,3,4),(-10.1295685708718,-9.97571372982934,
-8.97814235684641,-7.98057098386347,-6.98299961088054,-5.9854282378976,
-4.98785686491467,-3.99028549193173,-3.84638326369226),.UNSPECIFIED.);
#1964=B_SPLINE_CURVE_WITH_KNOTS('',3,(#19247,#19248,#19249,#19250,#19251,
#19252,#19253,#19254,#19255,#19256,#19257,#19258,#19259,#19260,#19261,#19262,
#19263,#19264,#19265,#19266,#19267,#19268),.UNSPECIFIED.,.F.,.F.,(4,3,3,
3,3,3,3,4),(7.59300756235157,7.98057098386347,8.9781423568464,9.97571372982934,
10.9732851028123,11.9708564757952,12.9684278487781,13.8761928695311),
 .UNSPECIFIED.);
#1965=B_SPLINE_CURVE_WITH_KNOTS('',3,(#19269,#19270,#19271,#19272,#19273,
#19274,#19275,#19276,#19277,#19278,#19279,#19280,#19281,#19282,#19283,#19284,
#19285,#19286,#19287,#19288,#19289,#19290,#19291,#19292,#19293,#19294,#19295,
#19296,#19297,#19298,#19299,#19300,#19301,#19302,#19303,#19304,#19305,#19306,
#19307,#19308,#19309,#19310,#19311,#19312,#19313,#19314,#19315,#19316,#19317,
#19318,#19319,#19320),.UNSPECIFIED.,.F.,.F.,(4,3,3,3,3,3,3,3,3,3,3,3,3,
3,3,3,3,4),(0.,0.0396791507684394,0.0597938827984087,0.0771996525601983,
0.0898307615993676,0.128492920651297,0.153526877334627,0.165101563474246,
0.197163594226425,0.22445212238587,0.234160516714088,0.269455189460283,
0.287578726323234,0.30542148874616,0.333081540294033,0.34722488830939,0.375339207698871,
0.378621596831437),.UNSPECIFIED.);
#1966=B_SPLINE_CURVE_WITH_KNOTS('',3,(#19323,#19324,#19325,#19326,#19327,
#19328,#19329,#19330,#19331,#19332,#19333,#19334,#19335,#19336,#19337,#19338,
#19339,#19340,#19341,#19342,#19343,#19344,#19345,#19346,#19347,#19348,#19349,
#19350,#19351,#19352,#19353,#19354,#19355,#19356,#19357,#19358,#19359,#19360,
#19361,#19362,#19363,#19364,#19365,#19366,#19367,#19368,#19369,#19370,#19371,
#19372,#19373,#19374,#19375,#19376,#19377),.UNSPECIFIED.,.F.,.F.,(4,3,3,
3,3,3,3,3,3,3,3,3,3,3,3,3,3,3,4),(-0.378621596831421,-0.35356224610225,
-0.339726792605717,-0.324795397019123,-0.299967964935665,-0.289118709747788,
-0.252370025571504,-0.234474277842488,-0.219335629751949,-0.200829495678081,
-0.174827335946658,-0.155846980593001,-0.144923798098897,-0.109697001525397,
-0.0896700514919927,-0.0773387576028108,-0.0372142610763827,-0.00401661180489582,
0.),.UNSPECIFIED.);
#1967=B_SPLINE_CURVE_WITH_KNOTS('',3,(#19378,#19379,#19380,#19381,#19382,
#19383,#19384,#19385,#19386,#19387,#19388,#19389,#19390,#19391,#19392,#19393,
#19394,#19395,#19396,#19397,#19398,#19399,#19400,#19401,#19402,#19403,#19404,
#19405,#19406,#19407,#19408,#19409,#19410,#19411,#19412,#19413,#19414,#19415,
#19416,#19417,#19418,#19419,#19420,#19421,#19422,#19423,#19424,#19425,#19426,
#19427,#19428,#19429,#19430,#19431,#19432),.UNSPECIFIED.,.F.,.F.,(4,3,3,
3,3,3,3,3,3,3,3,3,3,3,3,3,3,3,4),(-0.376940817211658,-0.35160243790482,
-0.332519425088979,-0.318228074800829,-0.288333550643748,-0.272718146690274,
-0.234505396639293,-0.21696217861614,-0.205493442096022,-0.18085482887096,
-0.153734148588707,-0.136642726461199,-0.12620501784944,-0.095471365644694,
-0.0666260826793201,-0.0558555936353674,-0.021961250336811,-0.00327040903045685,
0.),.UNSPECIFIED.);
#1968=B_SPLINE_CURVE_WITH_KNOTS('',3,(#19434,#19435,#19436,#19437,#19438,
#19439,#19440,#19441,#19442,#19443,#19444),.UNSPECIFIED.,.F.,.F.,(4,1,1,
1,1,1,1,1,4),(15.7079632679489,15.8518654961884,16.8494368691713,17.8470082421543,
18.8445796151372,19.8421509881202,20.8397223611031,21.837293734086,21.9911485751285),
 .UNSPECIFIED.);
#1969=B_SPLINE_CURVE_WITH_KNOTS('',3,(#19445,#19446,#19447,#19448,#19449,
#19450,#19451,#19452,#19453,#19454),.UNSPECIFIED.,.F.,.F.,(4,1,1,1,1,1,
1,4),(15.7079632679489,16.3932837587428,17.3908551317257,18.3884265047087,
19.3859978776916,20.3835692506745,21.3811406236575,21.9911485751285),
 .UNSPECIFIED.);
#1970=B_SPLINE_CURVE_WITH_KNOTS('',3,(#19799,#19800,#19801,#19802,#19803,
#19804,#19805,#19806,#19807,#19808,#19809,#19810,#19811,#19812,#19813,#19814,
#19815,#19816,#19817,#19818,#19819,#19820,#19821,#19822,#19823,#19824,#19825,
#19826,#19827,#19828,#19829,#19830,#19831,#19832,#19833,#19834,#19835,#19836,
#19837,#19838,#19839,#19840,#19841,#19842,#19843,#19844,#19845,#19846,#19847,
#19848,#19849,#19850),.UNSPECIFIED.,.F.,.F.,(4,3,3,3,3,3,3,3,3,3,3,3,3,
3,3,3,3,4),(0.,0.0336910497355155,0.058734651365868,0.0734852344555961,
0.109792226014928,0.132864806965475,0.143631988775342,0.17720525627004,
0.1959120018626,0.20761397470913,0.244895197064516,0.269599368515367,0.282507810536056,
0.310158254371969,0.327758642889101,0.342580296989548,0.372940760482291,
0.376940817211643),.UNSPECIFIED.);
#1971=B_SPLINE_CURVE_WITH_KNOTS('',3,(#19851,#19852,#19853,#19854,#19855,
#19856,#19857,#19858,#19859,#19860,#19861,#19862,#19863,#19864,#19865,#19866,
#19867,#19868,#19869,#19870,#19871,#19872,#19873,#19874,#19875),
 .UNSPECIFIED.,.F.,.F.,(4,3,3,3,3,3,3,3,4),(-10.1295685708718,-9.97571372982934,
-8.97814235684641,-7.98057098386347,-6.98299961088054,-5.9854282378976,
-4.98785686491467,-3.99028549193173,-3.84638326369226),.UNSPECIFIED.);
#1972=B_SPLINE_CURVE_WITH_KNOTS('',3,(#20220,#20221,#20222,#20223,#20224,
#20225,#20226,#20227,#20228,#20229,#20230,#20231,#20232,#20233,#20234,#20235,
#20236,#20237,#20238,#20239,#20240,#20241),.UNSPECIFIED.,.F.,.F.,(4,3,3,
3,3,3,3,4),(7.59300756235157,7.98057098386347,8.9781423568464,9.97571372982934,
10.9732851028123,11.9708564757952,12.9684278487781,13.8761928695311),
 .UNSPECIFIED.);
#1973=B_SPLINE_CURVE_WITH_KNOTS('',3,(#20242,#20243,#20244,#20245,#20246,
#20247,#20248,#20249,#20250,#20251,#20252,#20253,#20254,#20255,#20256,#20257,
#20258,#20259,#20260,#20261,#20262,#20263,#20264,#20265,#20266,#20267,#20268,
#20269,#20270,#20271,#20272,#20273,#20274,#20275,#20276,#20277,#20278,#20279,
#20280,#20281,#20282,#20283,#20284,#20285,#20286,#20287,#20288,#20289,#20290,
#20291,#20292,#20293),.UNSPECIFIED.,.F.,.F.,(4,3,3,3,3,3,3,3,3,3,3,3,3,
3,3,3,3,4),(0.,0.0396791423592224,0.0597938176449427,0.0771989368507012,
0.0898305980572942,0.128492765250004,0.153526730198623,0.165101530608957,
0.197163594226419,0.224452126331546,0.234160522045081,0.269455193458526,
0.287578665402526,0.305421500398064,0.333081575029239,0.347224893982947,
0.375339207698863,0.378621596831429),.UNSPECIFIED.);
#1974=B_SPLINE_CURVE_WITH_KNOTS('',3,(#20484,#20485,#20486,#20487),
 .UNSPECIFIED.,.F.,.F.,(4,4),(51.5750455984138,52.2860549491936),
 .UNSPECIFIED.);
#1975=B_SPLINE_CURVE_WITH_KNOTS('',3,(#20490,#20491,#20492,#20493,#20494,
#20495,#20496,#20497,#20498,#20499),.UNSPECIFIED.,.F.,.F.,(4,3,3,4),(-50.2654824574367,
-49.3264669332015,-48.3399375945375,-47.8348991546268),.UNSPECIFIED.);
#1976=B_SPLINE_CURVE_WITH_KNOTS('',3,(#20504,#20505,#20506,#20507,#20508,
#20509,#20510,#20511,#20512,#20513,#20514,#20515,#20516,#20517,#20518,#20519,
#20520,#20521,#20522,#20523,#20524,#20525,#20526,#20527,#20528),
 .UNSPECIFIED.,.F.,.F.,(4,3,3,3,3,3,3,3,4),(45.2918602912342,45.3803495785454,
46.3668789172094,47.3534082558735,48.3399375945375,49.3264669332015,50.3129962718656,
51.2995256105296,51.5750455984138),.UNSPECIFIED.);
#1977=B_SPLINE_CURVE_WITH_KNOTS('',3,(#20529,#20530,#20531,#20532,#20533,
#20534,#20535,#20536,#20537,#20538,#20539,#20540,#20541,#20542,#20543,#20544,
#20545,#20546,#20547,#20548,#20549,#20550),.UNSPECIFIED.,.F.,.F.,(4,3,3,
3,3,3,3,4),(-47.8348991546268,-47.3534082558735,-46.3668789172095,-45.3803495785454,
-44.3938202398814,-43.4072909012174,-42.4207615625533,-41.5517138474472),
 .UNSPECIFIED.);
#1978=B_SPLINE_CURVE_WITH_KNOTS('',3,(#20555,#20556,#20557,#20558,#20559,
#20560,#20561,#20562,#20563,#20564,#20565,#20566,#20567,#20568,#20569,#20570,
#20571,#20572,#20573,#20574,#20575,#20576),.UNSPECIFIED.,.F.,.F.,(4,3,3,
3,3,3,3,4),(39.0086749840546,39.4611735465612,40.4477028852253,41.4342322238893,
42.4207615625533,43.4072909012174,44.3938202398814,45.2918602912342),
 .UNSPECIFIED.);
#1979=B_SPLINE_CURVE_WITH_KNOTS('',3,(#20577,#20578,#20579,#20580,#20581,
#20582,#20583,#20584,#20585,#20586,#20587,#20588,#20589,#20590,#20591,#20592,
#20593,#20594,#20595,#20596,#20597,#20598,#20599,#20600,#20601),
 .UNSPECIFIED.,.F.,.F.,(4,3,3,3,3,3,3,3,4),(-41.5517138474472,-41.4342322238893,
-40.4477028852253,-39.4611735465612,-38.4746442078972,-37.4881148692332,
-36.5015855305691,-35.5150561919051,-35.2685285402676),.UNSPECIFIED.);
#1980=B_SPLINE_CURVE_WITH_KNOTS('',3,(#20606,#20607,#20608,#20609,#20610,
#20611,#20612,#20613,#20614,#20615,#20616,#20617,#20618,#20619,#20620,#20621,
#20622,#20623,#20624,#20625,#20626,#20627),.UNSPECIFIED.,.F.,.F.,(4,3,3,
3,3,3,3,4),(32.725489676875,33.541997514577,34.5285268532411,35.5150561919051,
36.5015855305691,37.4881148692332,38.4746442078972,39.0086749840546),
 .UNSPECIFIED.);
#1981=B_SPLINE_CURVE_WITH_KNOTS('',3,(#20628,#20629,#20630,#20631,#20632,
#20633,#20634,#20635,#20636,#20637,#20638,#20639,#20640,#20641,#20642,#20643,
#20644,#20645,#20646,#20647,#20648,#20649),.UNSPECIFIED.,.F.,.F.,(4,3,3,
3,3,3,3,4),(-35.2685285402676,-34.5285268532411,-33.541997514577,-32.555468175913,
-31.568938837249,-30.582409498585,-29.5958801599209,-28.985343233088),
 .UNSPECIFIED.);
#1982=B_SPLINE_CURVE_WITH_KNOTS('',3,(#20654,#20655,#20656,#20657,#20658,
#20659,#20660,#20661,#20662,#20663,#20664,#20665,#20666,#20667,#20668,#20669,
#20670,#20671,#20672,#20673,#20674,#20675,#20676,#20677,#20678),
 .UNSPECIFIED.,.F.,.F.,(4,3,3,3,3,3,3,3,4),(26.4423043696954,26.6362921439288,
27.6228214825929,28.6093508212569,29.5958801599209,30.582409498585,31.568938837249,
32.555468175913,32.725489676875),.UNSPECIFIED.);
#1983=B_SPLINE_CURVE_WITH_KNOTS('',3,(#20679,#20680,#20681,#20682,#20683,
#20684,#20685,#20686,#20687,#20688,#20689,#20690,#20691,#20692,#20693,#20694,
#20695,#20696,#20697,#20698,#20699,#20700),.UNSPECIFIED.,.F.,.F.,(4,3,3,
3,3,3,3,4),(-28.985343233088,-28.6093508212569,-27.6228214825929,-26.6362921439288,
-25.6497628052648,-24.6632334666008,-23.6767041279367,-22.7021579259084),
 .UNSPECIFIED.);
#1984=B_SPLINE_CURVE_WITH_KNOTS('',3,(#20705,#20706,#20707,#20708,#20709,
#20710,#20711,#20712,#20713,#20714,#20715,#20716,#20717,#20718,#20719,#20720,
#20721,#20722,#20723,#20724,#20725,#20726),.UNSPECIFIED.,.F.,.F.,(4,3,3,
3,3,3,3,4),(20.1591190625159,20.7171161119446,21.7036454506087,22.6901747892727,
23.6767041279367,24.6632334666008,25.6497628052648,26.4423043696954),
 .UNSPECIFIED.);
#1985=B_SPLINE_CURVE_WITH_KNOTS('',3,(#20727,#20728,#20729,#20730,#20731,
#20732,#20733,#20734,#20735,#20736,#20737,#20738,#20739,#20740,#20741,#20742,
#20743,#20744,#20745,#20746,#20747,#20748,#20749,#20750,#20751),
 .UNSPECIFIED.,.F.,.F.,(4,3,3,3,3,3,3,3,4),(-22.7021579259084,-22.6901747892727,
-21.7036454506087,-20.7171161119446,-19.7305867732806,-18.7440574346166,
-17.7575280959526,-16.7709987572885,-16.4189726187288),.UNSPECIFIED.);
#1986=B_SPLINE_CURVE_WITH_KNOTS('',3,(#20756,#20757,#20758,#20759,#20760,
#20761,#20762,#20763,#20764,#20765,#20766,#20767,#20768,#20769,#20770,#20771,
#20772,#20773,#20774,#20775,#20776,#20777),.UNSPECIFIED.,.F.,.F.,(4,3,3,
3,3,3,3,4),(13.8759337553363,14.7979400799605,15.7844694186245,16.7709987572885,
17.7575280959526,18.7440574346166,19.7305867732806,20.1591190625159),
 .UNSPECIFIED.);
#1987=B_SPLINE_CURVE_WITH_KNOTS('',3,(#20778,#20779,#20780,#20781,#20782,
#20783,#20784,#20785,#20786,#20787,#20788,#20789,#20790,#20791,#20792,#20793,
#20794,#20795,#20796,#20797,#20798,#20799),.UNSPECIFIED.,.F.,.F.,(4,3,3,
3,3,3,3,4),(-16.4189726187288,-15.7844694186245,-14.7979400799605,-13.8114107412964,
-12.8248814026324,-11.8383520639684,-10.8518227253043,-10.1357873115492),
 .UNSPECIFIED.);
#1988=B_SPLINE_CURVE_WITH_KNOTS('',3,(#20805,#20806,#20807,#20808,#20809,
#20810,#20811,#20812,#20813,#20814,#20815,#20816,#20817),.UNSPECIFIED.,
 .F.,.F.,(4,3,3,3,4),(-3.85260200436966,-2.95958801599209,-1.97305867732806,
-0.986529338664031,0.),.UNSPECIFIED.);
#1989=B_SPLINE_CURVE_WITH_KNOTS('',3,(#20820,#20821,#20822,#20823,#20824,
#20825,#20826,#20827,#20828,#20829,#20830,#20831,#20832,#20833,#20834,#20835,
#20836,#20837,#20838),.UNSPECIFIED.,.F.,.F.,(4,3,3,3,3,3,4),(2.0205724917569,
2.95958801599209,3.94611735465613,4.93264669332016,5.91917603198418,6.90570537064821,
7.5927484481567),.UNSPECIFIED.);
#1990=B_SPLINE_CURVE_WITH_KNOTS('',3,(#20844,#20845,#20846,#20847),
 .UNSPECIFIED.,.F.,.F.,(4,4),(51.5750455984138,52.2860549491936),
 .UNSPECIFIED.);
#1991=B_SPLINE_CURVE_WITH_KNOTS('',3,(#20850,#20851,#20852,#20853,#20854,
#20855,#20856,#20857,#20858,#20859),.UNSPECIFIED.,.F.,.F.,(4,3,3,4),(-50.2654824574367,
-49.3264669332015,-48.3399375945375,-47.8348991546268),.UNSPECIFIED.);
#1992=B_SPLINE_CURVE_WITH_KNOTS('',3,(#20864,#20865,#20866,#20867,#20868,
#20869,#20870,#20871,#20872,#20873,#20874,#20875,#20876,#20877,#20878,#20879,
#20880,#20881,#20882,#20883,#20884,#20885,#20886,#20887,#20888),
 .UNSPECIFIED.,.F.,.F.,(4,3,3,3,3,3,3,3,4),(45.2918602912342,45.3803495785454,
46.3668789172094,47.3534082558735,48.3399375945375,49.3264669332015,50.3129962718656,
51.2995256105296,51.5750455984138),.UNSPECIFIED.);
#1993=B_SPLINE_CURVE_WITH_KNOTS('',3,(#20889,#20890,#20891,#20892,#20893,
#20894,#20895,#20896,#20897,#20898,#20899,#20900,#20901,#20902,#20903,#20904,
#20905,#20906,#20907,#20908,#20909,#20910),.UNSPECIFIED.,.F.,.F.,(4,3,3,
3,3,3,3,4),(-47.8348991546268,-47.3534082558735,-46.3668789172095,-45.3803495785454,
-44.3938202398814,-43.4072909012174,-42.4207615625533,-41.5517138474472),
 .UNSPECIFIED.);
#1994=B_SPLINE_CURVE_WITH_KNOTS('',3,(#20915,#20916,#20917,#20918,#20919,
#20920,#20921,#20922,#20923,#20924,#20925,#20926,#20927,#20928,#20929,#20930,
#20931,#20932,#20933,#20934,#20935,#20936),.UNSPECIFIED.,.F.,.F.,(4,3,3,
3,3,3,3,4),(39.0086749840546,39.4611735465612,40.4477028852253,41.4342322238893,
42.4207615625533,43.4072909012174,44.3938202398814,45.2918602912342),
 .UNSPECIFIED.);
#1995=B_SPLINE_CURVE_WITH_KNOTS('',3,(#20937,#20938,#20939,#20940,#20941,
#20942,#20943,#20944,#20945,#20946,#20947,#20948,#20949,#20950,#20951,#20952,
#20953,#20954,#20955,#20956,#20957,#20958,#20959,#20960,#20961),
 .UNSPECIFIED.,.F.,.F.,(4,3,3,3,3,3,3,3,4),(-41.5517138474472,-41.4342322238893,
-40.4477028852253,-39.4611735465612,-38.4746442078972,-37.4881148692332,
-36.5015855305691,-35.5150561919051,-35.2685285402676),.UNSPECIFIED.);
#1996=B_SPLINE_CURVE_WITH_KNOTS('',3,(#20966,#20967,#20968,#20969,#20970,
#20971,#20972,#20973,#20974,#20975,#20976,#20977,#20978,#20979,#20980,#20981,
#20982,#20983,#20984,#20985,#20986,#20987),.UNSPECIFIED.,.F.,.F.,(4,3,3,
3,3,3,3,4),(32.725489676875,33.541997514577,34.5285268532411,35.5150561919051,
36.5015855305691,37.4881148692332,38.4746442078972,39.0086749840546),
 .UNSPECIFIED.);
#1997=B_SPLINE_CURVE_WITH_KNOTS('',3,(#20988,#20989,#20990,#20991,#20992,
#20993,#20994,#20995,#20996,#20997,#20998,#20999,#21000,#21001,#21002,#21003,
#21004,#21005,#21006,#21007,#21008,#21009),.UNSPECIFIED.,.F.,.F.,(4,3,3,
3,3,3,3,4),(-35.2685285402676,-34.5285268532411,-33.541997514577,-32.555468175913,
-31.568938837249,-30.582409498585,-29.5958801599209,-28.985343233088),
 .UNSPECIFIED.);
#1998=B_SPLINE_CURVE_WITH_KNOTS('',3,(#21014,#21015,#21016,#21017,#21018,
#21019,#21020,#21021,#21022,#21023,#21024,#21025,#21026,#21027,#21028,#21029,
#21030,#21031,#21032,#21033,#21034,#21035,#21036,#21037,#21038),
 .UNSPECIFIED.,.F.,.F.,(4,3,3,3,3,3,3,3,4),(26.4423043696954,26.6362921439288,
27.6228214825929,28.6093508212569,29.5958801599209,30.582409498585,31.568938837249,
32.555468175913,32.725489676875),.UNSPECIFIED.);
#1999=B_SPLINE_CURVE_WITH_KNOTS('',3,(#21039,#21040,#21041,#21042,#21043,
#21044,#21045,#21046,#21047,#21048,#21049,#21050,#21051,#21052,#21053,#21054,
#21055,#21056,#21057,#21058,#21059,#21060),.UNSPECIFIED.,.F.,.F.,(4,3,3,
3,3,3,3,4),(-28.985343233088,-28.6093508212569,-27.6228214825929,-26.6362921439288,
-25.6497628052648,-24.6632334666008,-23.6767041279367,-22.7021579259084),
 .UNSPECIFIED.);
#2000=B_SPLINE_CURVE_WITH_KNOTS('',3,(#21065,#21066,#21067,#21068,#21069,
#21070,#21071,#21072,#21073,#21074,#21075,#21076,#21077,#21078,#21079,#21080,
#21081,#21082,#21083,#21084,#21085,#21086),.UNSPECIFIED.,.F.,.F.,(4,3,3,
3,3,3,3,4),(20.1591190625159,20.7171161119446,21.7036454506087,22.6901747892727,
23.6767041279367,24.6632334666008,25.6497628052648,26.4423043696954),
 .UNSPECIFIED.);
#2001=B_SPLINE_CURVE_WITH_KNOTS('',3,(#21087,#21088,#21089,#21090,#21091,
#21092,#21093,#21094,#21095,#21096,#21097,#21098,#21099,#21100,#21101,#21102,
#21103,#21104,#21105,#21106,#21107,#21108,#21109,#21110,#21111),
 .UNSPECIFIED.,.F.,.F.,(4,3,3,3,3,3,3,3,4),(-22.7021579259084,-22.6901747892727,
-21.7036454506087,-20.7171161119446,-19.7305867732806,-18.7440574346166,
-17.7575280959526,-16.7709987572885,-16.4189726187288),.UNSPECIFIED.);
#2002=B_SPLINE_CURVE_WITH_KNOTS('',3,(#21116,#21117,#21118,#21119,#21120,
#21121,#21122,#21123,#21124,#21125,#21126,#21127,#21128,#21129,#21130,#21131,
#21132,#21133,#21134,#21135,#21136,#21137),.UNSPECIFIED.,.F.,.F.,(4,3,3,
3,3,3,3,4),(13.8759337553363,14.7979400799605,15.7844694186245,16.7709987572885,
17.7575280959526,18.7440574346166,19.7305867732806,20.1591190625159),
 .UNSPECIFIED.);
#2003=B_SPLINE_CURVE_WITH_KNOTS('',3,(#21138,#21139,#21140,#21141,#21142,
#21143,#21144,#21145,#21146,#21147,#21148,#21149,#21150,#21151,#21152,#21153,
#21154,#21155,#21156,#21157,#21158,#21159),.UNSPECIFIED.,.F.,.F.,(4,3,3,
3,3,3,3,4),(-16.4189726187288,-15.7844694186245,-14.7979400799605,-13.8114107412964,
-12.8248814026324,-11.8383520639684,-10.8518227253043,-10.1357873115492),
 .UNSPECIFIED.);
#2004=B_SPLINE_CURVE_WITH_KNOTS('',3,(#21165,#21166,#21167,#21168,#21169,
#21170,#21171,#21172,#21173,#21174,#21175,#21176,#21177),.UNSPECIFIED.,
 .F.,.F.,(4,3,3,3,4),(-3.85260200436966,-2.95958801599209,-1.97305867732806,
-0.986529338664031,0.),.UNSPECIFIED.);
#2005=B_SPLINE_CURVE_WITH_KNOTS('',3,(#21180,#21181,#21182,#21183,#21184,
#21185,#21186,#21187,#21188,#21189,#21190,#21191,#21192,#21193,#21194,#21195,
#21196,#21197,#21198),.UNSPECIFIED.,.F.,.F.,(4,3,3,3,3,3,4),(2.0205724917569,
2.95958801599209,3.94611735465612,4.93264669332016,5.91917603198418,6.90570537064822,
7.5927484481567),.UNSPECIFIED.);
#2006=B_SPLINE_CURVE_WITH_KNOTS('',3,(#21204,#21205,#21206,#21207,#21208,
#21209,#21210,#21211),.UNSPECIFIED.,.F.,.F.,(4,1,1,1,1,4),(59.6902604182061,
60.1952988581168,61.1818281967808,62.1683575354449,63.1548868741089,64.1414162127729),
 .UNSPECIFIED.);
#2007=B_SPLINE_CURVE_WITH_KNOTS('',3,(#21214,#21215,#21216,#21217,#21218,
#21219,#21220,#21221,#21222),.UNSPECIFIED.,.F.,.F.,(4,1,1,1,1,1,4),(59.6902604182061,
59.7787497055172,60.7652790441813,61.7518083828453,62.7383377215093,63.7248670601734,
64.6638825844086),.UNSPECIFIED.);
#2008=B_SPLINE_CURVE_WITH_KNOTS('',3,(#21227,#21228,#21229,#21230,#21231,
#21232,#21233,#21234,#21235,#21236),.UNSPECIFIED.,.F.,.F.,(4,1,1,1,1,1,
1,4),(53.4070751110265,54.2761228261326,55.2626521647967,56.2491815034607,
57.2357108421247,58.2222401807888,59.2087695194528,59.6902604182061),
 .UNSPECIFIED.);
#2009=B_SPLINE_CURVE_WITH_KNOTS('',3,(#21237,#21238,#21239,#21240,#21241,
#21242,#21243,#21244,#21245,#21246),.UNSPECIFIED.,.F.,.F.,(4,1,1,1,1,1,
1,4),(53.4070751110265,53.8595736735331,54.8461030121971,55.8326323508611,
56.8191616895251,57.8056910281892,58.7922203668532,59.6902604182061),
 .UNSPECIFIED.);
#2010=B_SPLINE_CURVE_WITH_KNOTS('',3,(#21251,#21252,#21253,#21254,#21255,
#21256,#21257,#21258,#21259,#21260,#21261),.UNSPECIFIED.,.F.,.F.,(4,1,1,
1,1,1,1,1,4),(47.1238898038469,47.3704174554844,48.3569467941484,49.3434761328125,
50.3300054714765,51.3165348101405,52.3030641488046,53.2895934874686,53.4070751110265),
 .UNSPECIFIED.);
#2011=B_SPLINE_CURVE_WITH_KNOTS('',3,(#21262,#21263,#21264,#21265,#21266,
#21267,#21268,#21269,#21270,#21271),.UNSPECIFIED.,.F.,.F.,(4,1,1,1,1,1,
1,4),(47.1238898038469,47.9403976415489,48.9269269802129,49.9134563188769,
50.899985657541,51.886514996205,52.873044334869,53.4070751110265),
 .UNSPECIFIED.);
#2012=B_SPLINE_CURVE_WITH_KNOTS('',3,(#21276,#21277,#21278,#21279,#21280,
#21281,#21282,#21283,#21284,#21285),.UNSPECIFIED.,.F.,.F.,(4,1,1,1,1,1,
1,4),(40.8407044966673,41.4512414235002,42.4377707621643,43.4243001008283,
44.4108294394923,45.3973587781563,46.3838881168204,47.1238898038469),
 .UNSPECIFIED.);
#2013=B_SPLINE_CURVE_WITH_KNOTS('',3,(#21286,#21287,#21288,#21289,#21290,
#21291,#21292,#21293,#21294,#21295,#21296),.UNSPECIFIED.,.F.,.F.,(4,1,1,
1,1,1,1,1,4),(40.8407044966673,41.0346922709007,42.0212216095647,43.0077509482287,
43.9942802868928,44.9808096255568,45.9673389642208,46.9538683028848,47.1238898038469),
 .UNSPECIFIED.);
#2014=B_SPLINE_CURVE_WITH_KNOTS('',3,(#21301,#21302,#21303,#21304,#21305,
#21306,#21307,#21308,#21309,#21310),.UNSPECIFIED.,.F.,.F.,(4,1,1,1,1,1,
1,4),(34.5575191894877,35.532065391516,36.5185947301801,37.5051240688441,
38.4916534075081,39.4781827461722,40.4647120848362,40.8407044966673),
 .UNSPECIFIED.);
#2015=B_SPLINE_CURVE_WITH_KNOTS('',3,(#21311,#21312,#21313,#21314,#21315,
#21316,#21317,#21318,#21319,#21320),.UNSPECIFIED.,.F.,.F.,(4,1,1,1,1,1,
1,4),(34.5575191894877,35.1155162389165,36.1020455775805,37.0885749162445,
38.0751042549086,39.0616335935726,40.0481629322366,40.8407044966673),
 .UNSPECIFIED.);
#2016=B_SPLINE_CURVE_WITH_KNOTS('',3,(#21325,#21326,#21327,#21328,#21329,
#21330,#21331,#21332,#21333,#21334,#21335),.UNSPECIFIED.,.F.,.F.,(4,1,1,
1,1,1,1,1,4),(28.2743338823081,28.6263600208678,29.6128893595319,30.5994186981959,
31.5859480368599,32.5724773755239,33.559006714188,34.545536052852,34.5575191894877),
 .UNSPECIFIED.);
#2017=B_SPLINE_CURVE_WITH_KNOTS('',3,(#21336,#21337,#21338,#21339,#21340,
#21341,#21342,#21343,#21344,#21345),.UNSPECIFIED.,.F.,.F.,(4,1,1,1,1,1,
1,4),(28.2743338823081,29.1963402069323,30.1828695455963,31.1693988842604,
32.1559282229244,33.1424575615884,34.1289869002524,34.5575191894877),
 .UNSPECIFIED.);
#2018=B_SPLINE_CURVE_WITH_KNOTS('',3,(#21350,#21351,#21352,#21353,#21354,
#21355,#21356,#21357,#21358,#21359),.UNSPECIFIED.,.F.,.F.,(4,1,1,1,1,1,
1,4),(21.9911485751285,22.7071839888836,23.6937133275477,24.6802426662117,
25.6667720048757,26.6533013435398,27.6398306822038,28.2743338823081),
 .UNSPECIFIED.);
#2019=B_SPLINE_CURVE_WITH_KNOTS('',3,(#21360,#21361,#21362,#21363,#21364,
#21365,#21366,#21367,#21368,#21369,#21370),.UNSPECIFIED.,.F.,.F.,(4,1,1,
1,1,1,1,1,4),(21.9911485751285,22.2906348362841,23.2771641749481,24.2636935136121,
25.2502228522762,26.2367521909402,27.2232815296042,28.2098108682683,28.2743338823081),
 .UNSPECIFIED.);
#2020=B_SPLINE_CURVE_WITH_KNOTS('',3,(#21376,#21377,#21378,#21379,#21380),
 .UNSPECIFIED.,.F.,.F.,(4,1,4),(14.3984001269718,15.3849294656359,15.707963267949),
 .UNSPECIFIED.);
#2021=B_SPLINE_CURVE_WITH_KNOTS('',3,(#21383,#21384,#21385,#21386,#21387),
 .UNSPECIFIED.,.F.,.F.,(4,1,4),(13.8759337553362,14.8149492795714,15.7079632679489),
 .UNSPECIFIED.);
#2022=B_SPLINE_CURVE_WITH_KNOTS('',3,(#21393,#21394,#21395,#21396,#21397,
#21398,#21399,#21400),.UNSPECIFIED.,.F.,.F.,(4,1,1,1,1,4),(59.6902604182061,
60.1952988581168,61.1818281967808,62.1683575354449,63.1548868741089,64.1414162127729),
 .UNSPECIFIED.);
#2023=B_SPLINE_CURVE_WITH_KNOTS('',3,(#21403,#21404,#21405,#21406,#21407,
#21408,#21409,#21410,#21411),.UNSPECIFIED.,.F.,.F.,(4,1,1,1,1,1,4),(59.6902604182061,
59.7787497055172,60.7652790441813,61.7518083828453,62.7383377215093,63.7248670601734,
64.6638825844086),.UNSPECIFIED.);
#2024=B_SPLINE_CURVE_WITH_KNOTS('',3,(#21416,#21417,#21418,#21419,#21420,
#21421,#21422,#21423,#21424,#21425),.UNSPECIFIED.,.F.,.F.,(4,1,1,1,1,1,
1,4),(53.4070751110265,54.2761228261326,55.2626521647967,56.2491815034607,
57.2357108421247,58.2222401807888,59.2087695194528,59.6902604182061),
 .UNSPECIFIED.);
#2025=B_SPLINE_CURVE_WITH_KNOTS('',3,(#21426,#21427,#21428,#21429,#21430,
#21431,#21432,#21433,#21434,#21435),.UNSPECIFIED.,.F.,.F.,(4,1,1,1,1,1,
1,4),(53.4070751110265,53.8595736735331,54.8461030121971,55.8326323508611,
56.8191616895251,57.8056910281892,58.7922203668532,59.6902604182061),
 .UNSPECIFIED.);
#2026=B_SPLINE_CURVE_WITH_KNOTS('',3,(#21440,#21441,#21442,#21443,#21444,
#21445,#21446,#21447,#21448,#21449,#21450),.UNSPECIFIED.,.F.,.F.,(4,1,1,
1,1,1,1,1,4),(47.1238898038469,47.3704174554844,48.3569467941484,49.3434761328125,
50.3300054714765,51.3165348101405,52.3030641488046,53.2895934874686,53.4070751110265),
 .UNSPECIFIED.);
#2027=B_SPLINE_CURVE_WITH_KNOTS('',3,(#21451,#21452,#21453,#21454,#21455,
#21456,#21457,#21458,#21459,#21460),.UNSPECIFIED.,.F.,.F.,(4,1,1,1,1,1,
1,4),(47.1238898038469,47.9403976415489,48.9269269802129,49.9134563188769,
50.899985657541,51.886514996205,52.873044334869,53.4070751110265),
 .UNSPECIFIED.);
#2028=B_SPLINE_CURVE_WITH_KNOTS('',3,(#21465,#21466,#21467,#21468,#21469,
#21470,#21471,#21472,#21473,#21474),.UNSPECIFIED.,.F.,.F.,(4,1,1,1,1,1,
1,4),(40.8407044966673,41.4512414235002,42.4377707621643,43.4243001008283,
44.4108294394923,45.3973587781563,46.3838881168204,47.1238898038469),
 .UNSPECIFIED.);
#2029=B_SPLINE_CURVE_WITH_KNOTS('',3,(#21475,#21476,#21477,#21478,#21479,
#21480,#21481,#21482,#21483,#21484,#21485),.UNSPECIFIED.,.F.,.F.,(4,1,1,
1,1,1,1,1,4),(40.8407044966673,41.0346922709007,42.0212216095647,43.0077509482287,
43.9942802868928,44.9808096255568,45.9673389642208,46.9538683028848,47.1238898038469),
 .UNSPECIFIED.);
#2030=B_SPLINE_CURVE_WITH_KNOTS('',3,(#21490,#21491,#21492,#21493,#21494,
#21495,#21496,#21497,#21498,#21499),.UNSPECIFIED.,.F.,.F.,(4,1,1,1,1,1,
1,4),(34.5575191894877,35.532065391516,36.5185947301801,37.5051240688441,
38.4916534075081,39.4781827461722,40.4647120848362,40.8407044966673),
 .UNSPECIFIED.);
#2031=B_SPLINE_CURVE_WITH_KNOTS('',3,(#21500,#21501,#21502,#21503,#21504,
#21505,#21506,#21507,#21508,#21509),.UNSPECIFIED.,.F.,.F.,(4,1,1,1,1,1,
1,4),(34.5575191894877,35.1155162389165,36.1020455775805,37.0885749162445,
38.0751042549086,39.0616335935726,40.0481629322366,40.8407044966673),
 .UNSPECIFIED.);
#2032=B_SPLINE_CURVE_WITH_KNOTS('',3,(#21514,#21515,#21516,#21517,#21518,
#21519,#21520,#21521,#21522,#21523,#21524),.UNSPECIFIED.,.F.,.F.,(4,1,1,
1,1,1,1,1,4),(28.2743338823081,28.6263600208678,29.6128893595319,30.5994186981959,
31.5859480368599,32.5724773755239,33.559006714188,34.545536052852,34.5575191894877),
 .UNSPECIFIED.);
#2033=B_SPLINE_CURVE_WITH_KNOTS('',3,(#21525,#21526,#21527,#21528,#21529,
#21530,#21531,#21532,#21533,#21534),.UNSPECIFIED.,.F.,.F.,(4,1,1,1,1,1,
1,4),(28.2743338823081,29.1963402069323,30.1828695455963,31.1693988842604,
32.1559282229244,33.1424575615884,34.1289869002524,34.5575191894877),
 .UNSPECIFIED.);
#2034=B_SPLINE_CURVE_WITH_KNOTS('',3,(#21539,#21540,#21541,#21542,#21543,
#21544,#21545,#21546,#21547,#21548),.UNSPECIFIED.,.F.,.F.,(4,1,1,1,1,1,
1,4),(21.9911485751285,22.7071839888836,23.6937133275477,24.6802426662117,
25.6667720048757,26.6533013435398,27.6398306822038,28.2743338823081),
 .UNSPECIFIED.);
#2035=B_SPLINE_CURVE_WITH_KNOTS('',3,(#21549,#21550,#21551,#21552,#21553,
#21554,#21555,#21556,#21557,#21558,#21559),.UNSPECIFIED.,.F.,.F.,(4,1,1,
1,1,1,1,1,4),(21.9911485751285,22.2906348362841,23.2771641749481,24.2636935136121,
25.2502228522762,26.2367521909402,27.2232815296042,28.2098108682683,28.2743338823081),
 .UNSPECIFIED.);
#2036=B_SPLINE_CURVE_WITH_KNOTS('',3,(#21565,#21566,#21567,#21568,#21569),
 .UNSPECIFIED.,.F.,.F.,(4,1,4),(14.3984001269718,15.3849294656359,15.707963267949),
 .UNSPECIFIED.);
#2037=B_SPLINE_CURVE_WITH_KNOTS('',3,(#21572,#21573,#21574,#21575,#21576),
 .UNSPECIFIED.,.F.,.F.,(4,1,4),(13.8759337553362,14.8149492795714,15.7079632679489),
 .UNSPECIFIED.);
#2038=B_SPLINE_CURVE_WITH_KNOTS('',3,(#21578,#21579,#21580,#21581,#21582,
#21583,#21584,#21585,#21586,#21587,#21588),.UNSPECIFIED.,.F.,.F.,(4,1,1,
1,1,1,1,1,4),(15.7079632679489,15.8014786182354,16.7880079568995,17.7745372955635,
18.7610666342275,19.7475959728915,20.7341253115556,21.7206546502196,21.9911485751285),
 .UNSPECIFIED.);
#2039=B_SPLINE_CURVE_WITH_KNOTS('',3,(#21589,#21590,#21591,#21592,#21593,
#21594,#21595,#21596,#21597,#21598),.UNSPECIFIED.,.F.,.F.,(4,1,1,1,1,1,
1,4),(15.707963267949,16.3714588042999,17.3579881429639,18.344517481628,
19.331046820292,20.317576158956,21.30410549762,21.9911485751285),
 .UNSPECIFIED.);
#2040=B_SPLINE_CURVE_WITH_KNOTS('',3,(#21823,#21824,#21825,#21826,#21827,
#21828,#21829,#21830,#21831,#21832,#21833,#21834,#21835,#21836,#21837,#21838,
#21839,#21840,#21841,#21842,#21843,#21844,#21845,#21846,#21847,#21848,#21849,
#21850,#21851,#21852,#21853,#21854,#21855,#21856,#21857,#21858,#21859,#21860,
#21861,#21862,#21863,#21864,#21865,#21866,#21867,#21868,#21869,#21870,#21871,
#21872,#21873,#21874),.UNSPECIFIED.,.F.,.F.,(4,3,3,3,3,3,3,3,3,3,3,3,3,
3,3,3,3,4),(0.,0.0320331684328983,0.047982254793735,0.0587463569853809,
0.068374331906695,0.0996455206564278,0.112637667143497,0.122453511831961,
0.146764141737192,0.169126652772842,0.178509832567225,0.203948034872107,
0.222826517887668,0.233934300135679,0.251364503567911,0.26339901807632,
0.280262641786753,0.286347380332264),.UNSPECIFIED.);
#2041=B_SPLINE_CURVE_WITH_KNOTS('',3,(#21875,#21876,#21877,#21878,#21879,
#21880,#21881,#21882,#21883,#21884,#21885,#21886,#21887,#21888,#21889,#21890,
#21891,#21892,#21893,#21894,#21895,#21896,#21897,#21898,#21899,#21900,#21901,
#21902,#21903,#21904,#21905,#21906,#21907,#21908,#21909,#21910,#21911,#21912,
#21913,#21914,#21915,#21916,#21917,#21918,#21919,#21920,#21921,#21922,#21923),
 .UNSPECIFIED.,.F.,.F.,(4,3,3,3,3,3,3,3,3,3,3,3,3,3,3,3,4),(0.,0.0274255978447832,
0.048809316595412,0.0580010326491972,0.0875347374149519,0.101224292480011,
0.111280556216297,0.132431451325231,0.155780476821444,0.165670961223459,
0.193708256295631,0.208717590629974,0.219760914288732,0.239138299607853,
0.257256761910142,0.277820141512149,0.28514280399518),.UNSPECIFIED.);
#2042=B_SPLINE_CURVE_WITH_KNOTS('',3,(#21924,#21925,#21926,#21927,#21928,
#21929,#21930,#21931,#21932,#21933,#21934,#21935,#21936,#21937,#21938,#21939,
#21940,#21941,#21942,#21943,#21944,#21945,#21946,#21947,#21948),
 .UNSPECIFIED.,.F.,.F.,(4,3,3,3,3,3,3,3,4),(-10.1357873115492,-9.8652933866403,
-8.87876404797627,-7.89223470931224,-6.90570537064821,-5.91917603198418,
-4.93264669332015,-3.94611735465612,-3.85260200436966),.UNSPECIFIED.);
#2043=B_SPLINE_CURVE_WITH_KNOTS('',3,(#22173,#22174,#22175,#22176,#22177,
#22178,#22179,#22180,#22181,#22182,#22183,#22184,#22185,#22186,#22187,#22188,
#22189,#22190,#22191,#22192,#22193,#22194,#22195,#22196,#22197,#22198,#22199,
#22200,#22201,#22202,#22203,#22204,#22205,#22206,#22207,#22208,#22209,#22210,
#22211,#22212,#22213,#22214,#22215,#22216,#22217,#22218,#22219,#22220,#22221),
 .UNSPECIFIED.,.F.,.F.,(4,3,3,3,3,3,3,3,3,3,3,3,3,3,3,3,4),(0.,0.0274255913653339,
0.0488093131133246,0.0580010269694127,0.0875347308595416,0.101224269152377,
0.111280553657591,0.132431451325227,0.155780477659062,0.165670961808075,
0.193708256734092,0.208717605217266,0.21976091765614,0.239138308570995,
0.257256762582239,0.277820141512144,0.28514280399514),.UNSPECIFIED.);
#2044=B_SPLINE_CURVE_WITH_KNOTS('',3,(#22222,#22223,#22224,#22225,#22226,
#22227,#22228,#22229,#22230,#22231,#22232,#22233,#22234,#22235,#22236,#22237,
#22238,#22239,#22240,#22241,#22242,#22243,#22244,#22245,#22246),
 .UNSPECIFIED.,.F.,.F.,(4,3,3,3,3,3,3,3,4),(7.5927484481567,7.89223470931224,
8.87876404797628,9.86529338664031,10.8518227253043,11.8383520639684,12.8248814026324,
13.8114107412964,13.8759337553363),.UNSPECIFIED.);
#2045=B_SPLINE_CURVE_WITH_KNOTS('',3,(#22247,#22248,#22249,#22250,#22251,
#22252,#22253,#22254,#22255,#22256,#22257,#22258,#22259,#22260,#22261,#22262,
#22263,#22264,#22265,#22266,#22267,#22268,#22269,#22270,#22271,#22272,#22273,
#22274,#22275,#22276,#22277,#22278,#22279,#22280,#22281,#22282,#22283,#22284,
#22285,#22286,#22287,#22288,#22289,#22290,#22291,#22292,#22293,#22294,#22295,
#22296,#22297,#22298),.UNSPECIFIED.,.F.,.F.,(4,3,3,3,3,3,3,3,3,3,3,3,3,
3,3,3,3,4),(0.,0.0320331645440323,0.0479822944538874,0.0587463983360561,
0.0683743388328265,0.0996455292883743,0.112637688108393,0.122453518454582,
0.146764141737195,0.169126651893336,0.178509831787203,0.20394803428708,
0.222826505940554,0.233934299906464,0.251364515046202,0.263399023832158,
0.280262641786714,0.28634738033223),.UNSPECIFIED.);
#2046=B_SPLINE_CURVE_WITH_KNOTS('',3,(#22312,#22313,#22314,#22315,#22316,
#22317,#22318,#22319,#22320,#22321,#22322,#22323,#22324,#22325,#22326,#22327,
#22328,#22329,#22330,#22331,#22332,#22333,#22334,#22335,#22336,#22337,#22338,
#22339,#22340,#22341,#22342,#22343,#22344,#22345,#22346,#22347,#22348,#22349,
#22350,#22351,#22352,#22353,#22354,#22355,#22356,#22357,#22358,#22359,#22360),
 .UNSPECIFIED.,.F.,.F.,(4,3,3,3,3,3,3,3,3,3,3,3,3,3,3,3,4),(0.,0.0274256070877454,
0.0488093215641943,0.0580010407627361,0.0875347467776894,0.101224325795315,
0.111280559869577,0.132431451325226,0.155780475624762,0.165670960389251,
0.193708255669975,0.208717569845021,0.219760909477782,0.239138286790648,
0.257256760954527,0.277820141512144,0.285142803995137),.UNSPECIFIED.);
#2047=B_SPLINE_CURVE_WITH_KNOTS('',3,(#22361,#22362,#22363,#22364,#22365,
#22366,#22367,#22368,#22369,#22370,#22371,#22372,#22373,#22374,#22375,#22376,
#22377,#22378,#22379,#22380,#22381,#22382,#22383,#22384,#22385,#22386,#22387,
#22388,#22389,#22390,#22391,#22392,#22393,#22394,#22395,#22396,#22397,#22398,
#22399,#22400,#22401,#22402,#22403,#22404,#22405,#22406,#22407,#22408,#22409,
#22410,#22411,#22412),.UNSPECIFIED.,.F.,.F.,(4,3,3,3,3,3,3,3,3,3,3,3,3,
3,3,3,3,4),(0.,0.032033144059138,0.0479825033685422,0.058746616231457,0.068374375333449,
0.0996455747709087,0.112637798572108,0.122453553351573,0.146764141737196,
0.169126647261903,0.17850982771232,0.203948031230928,0.22282644299279,0.233934298697096,
0.251364575521066,0.263399054117863,0.280262641786752,0.286347380332261),
 .UNSPECIFIED.);
#2048=B_SPLINE_CURVE_WITH_KNOTS('',3,(#22414,#22415,#22416,#22417,#22418,
#22419,#22420,#22421,#22422,#22423,#22424),.UNSPECIFIED.,.F.,.F.,(4,1,1,
1,1,1,1,1,4),(15.7079632679489,15.8014786182354,16.7880079568995,17.7745372955635,
18.7610666342275,19.7475959728915,20.7341253115556,21.7206546502196,21.9911485751285),
 .UNSPECIFIED.);
#2049=B_SPLINE_CURVE_WITH_KNOTS('',3,(#22425,#22426,#22427,#22428,#22429,
#22430,#22431,#22432,#22433,#22434),.UNSPECIFIED.,.F.,.F.,(4,1,1,1,1,1,
1,4),(15.707963267949,16.3714588042999,17.3579881429639,18.344517481628,
19.331046820292,20.317576158956,21.30410549762,21.9911485751285),
 .UNSPECIFIED.);
#2050=B_SPLINE_CURVE_WITH_KNOTS('',3,(#22659,#22660,#22661,#22662,#22663,
#22664,#22665,#22666,#22667,#22668,#22669,#22670,#22671,#22672,#22673,#22674,
#22675,#22676,#22677,#22678,#22679,#22680,#22681,#22682,#22683,#22684,#22685,
#22686,#22687,#22688,#22689,#22690,#22691,#22692,#22693,#22694,#22695,#22696,
#22697,#22698,#22699,#22700,#22701,#22702,#22703,#22704,#22705,#22706,#22707),
 .UNSPECIFIED.,.F.,.F.,(4,3,3,3,3,3,3,3,3,3,3,3,3,3,3,3,4),(0.,0.0274255572386018,
0.0488092947703195,0.0580009970300377,0.0875346963040298,0.101224146180659,
0.111280540172636,0.132431451325231,0.155780482071967,0.165670964883965,
0.19370825904101,0.208717681926172,0.219760935414438,0.239138355867989,
0.257256766122231,0.277820141512143,0.285142803995174),.UNSPECIFIED.);
#2051=B_SPLINE_CURVE_WITH_KNOTS('',3,(#22708,#22709,#22710,#22711,#22712,
#22713,#22714,#22715,#22716,#22717,#22718,#22719,#22720,#22721,#22722,#22723,
#22724,#22725,#22726,#22727,#22728,#22729,#22730,#22731,#22732),
 .UNSPECIFIED.,.F.,.F.,(4,3,3,3,3,3,3,3,4),(-10.1357873115492,-9.8652933866403,
-8.87876404797628,-7.89223470931224,-6.90570537064821,-5.91917603198418,
-4.93264669332015,-3.94611735465612,-3.85260200436966),.UNSPECIFIED.);
#2052=B_SPLINE_CURVE_WITH_KNOTS('',3,(#22957,#22958,#22959,#22960,#22961,
#22962,#22963,#22964,#22965,#22966,#22967,#22968,#22969,#22970,#22971,#22972,
#22973,#22974,#22975,#22976,#22977,#22978,#22979,#22980,#22981),
 .UNSPECIFIED.,.F.,.F.,(4,3,3,3,3,3,3,3,4),(7.5927484481567,7.89223470931225,
8.87876404797628,9.86529338664031,10.8518227253043,11.8383520639684,12.8248814026324,
13.8114107412964,13.8759337553363),.UNSPECIFIED.);
#2053=B_SPLINE_CURVE_WITH_KNOTS('',3,(#22982,#22983,#22984,#22985,#22986,
#22987,#22988,#22989,#22990,#22991,#22992,#22993,#22994,#22995,#22996,#22997,
#22998,#22999,#23000,#23001,#23002,#23003,#23004,#23005,#23006,#23007,#23008,
#23009,#23010,#23011,#23012,#23013,#23014,#23015,#23016,#23017,#23018,#23019,
#23020,#23021,#23022,#23023,#23024,#23025,#23026,#23027,#23028,#23029,#23030,
#23031,#23032,#23033),.UNSPECIFIED.,.F.,.F.,(4,3,3,3,3,3,3,3,3,3,3,3,3,
3,3,3,3,4),(0.,0.0320331739806594,0.047982198208099,0.0587462979950865,
0.0683743220264688,0.0996455083427913,0.112637637236076,0.122453502382791,
0.146764141737189,0.169126654027335,0.178509833663637,0.203948035694404,
0.222826534951851,0.233934300464251,0.251364487179106,0.263399009878289,
0.280262641786705,0.286347380332219),.UNSPECIFIED.);
#2054=B_SPLINE_CURVE_WITH_KNOTS('',3,(#23212,#23213,#23214,#23215,#23216,
#23217,#23218,#23219,#23220,#23221,#23222,#23223,#23224,#23225,#23226,#23227,
#23228,#23229,#23230,#23231,#23232,#23233),.UNSPECIFIED.,.F.,.F.,(4,3,3,
3,3,3,3,4),(76.7080459413271,76.8129957196858,77.8105670926688,78.8081384656517,
79.8057098386346,80.8032812116176,81.8008525846005,82.7984239575834),
 .UNSPECIFIED.);
#2055=B_SPLINE_CURVE_WITH_KNOTS('',3,(#23237,#23238,#23239,#23240,#23241,
#23242,#23243),.UNSPECIFIED.,.F.,.F.,(4,3,4),(-80.783811092309,-79.8057098386346,
-79.2446069498474),.UNSPECIFIED.);
#2056=B_SPLINE_CURVE_WITH_KNOTS('',3,(#23247,#23248,#23249,#23250,#23251,
#23252,#23253,#23254,#23255,#23256,#23257,#23258,#23259,#23260,#23261,#23262,
#23263,#23264,#23265,#23266,#23267,#23268),.UNSPECIFIED.,.F.,.F.,(4,3,3,
3,3,3,3,4),(-79.2446069498474,-78.8081384656517,-77.8105670926688,-76.8129957196858,
-75.8154243467029,-74.81785297372,-73.820281600737,-72.9614216426678),
 .UNSPECIFIED.);
#2057=B_SPLINE_CURVE_WITH_KNOTS('',3,(#23273,#23274,#23275,#23276,#23277,
#23278,#23279,#23280,#23281,#23282,#23283,#23284,#23285,#23286,#23287,#23288,
#23289,#23290,#23291,#23292,#23293,#23294),.UNSPECIFIED.,.F.,.F.,(4,3,3,
3,3,3,3,4),(70.4248606341475,70.8275674817882,71.8251388547712,72.8227102277541,
73.820281600737,74.81785297372,75.8154243467029,76.7080459413271),
 .UNSPECIFIED.);
#2058=B_SPLINE_CURVE_WITH_KNOTS('',3,(#23295,#23296,#23297,#23298,#23299,
#23300,#23301,#23302,#23303,#23304,#23305,#23306,#23307,#23308,#23309,#23310,
#23311,#23312,#23313,#23314,#23315,#23316,#23317,#23318,#23319),
 .UNSPECIFIED.,.F.,.F.,(4,3,3,3,3,3,3,3,4),(-72.9614216426678,-72.8227102277541,
-71.8251388547712,-70.8275674817882,-69.8299961088053,-68.8324247358224,
-67.8348533628394,-66.8372819898565,-66.6782363354882),.UNSPECIFIED.);
#2059=B_SPLINE_CURVE_WITH_KNOTS('',3,(#23324,#23325,#23326,#23327,#23328,
#23329,#23330,#23331,#23332,#23333,#23334,#23335,#23336,#23337,#23338,#23339,
#23340,#23341,#23342,#23343,#23344,#23345),.UNSPECIFIED.,.F.,.F.,(4,3,3,
3,3,3,3,4),(64.1416753269679,64.8421392438906,65.8397106168736,66.8372819898565,
67.8348533628394,68.8324247358224,69.8299961088053,70.4248606341475),
 .UNSPECIFIED.);
#2060=B_SPLINE_CURVE_WITH_KNOTS('',3,(#23346,#23347,#23348,#23349,#23350,
#23351,#23352,#23353,#23354,#23355,#23356,#23357,#23358,#23359,#23360,#23361,
#23362,#23363,#23364,#23365,#23366,#23367),.UNSPECIFIED.,.F.,.F.,(4,3,3,
3,3,3,3,4),(-66.6782363354882,-65.8397106168736,-64.8421392438907,-63.8445678709077,
-62.8469964979248,-61.8494251249419,-60.8518537519589,-60.3950510283086),
 .UNSPECIFIED.);
#2061=B_SPLINE_CURVE_WITH_KNOTS('',3,(#23372,#23373,#23374,#23375,#23376,
#23377,#23378,#23379,#23380,#23381,#23382,#23383,#23384,#23385,#23386,#23387,
#23388,#23389,#23390,#23391,#23392,#23393),.UNSPECIFIED.,.F.,.F.,(4,3,3,
3,3,3,3,4),(57.8584900197883,58.856711005993,59.854282378976,60.8518537519589,
61.8494251249418,62.8469964979247,63.8445678709077,64.1416753269679),
 .UNSPECIFIED.);
#2062=B_SPLINE_CURVE_WITH_KNOTS('',3,(#23394,#23395,#23396,#23397,#23398,
#23399,#23400,#23401,#23402,#23403,#23404,#23405,#23406,#23407,#23408,#23409,
#23410,#23411,#23412,#23413,#23414,#23415),.UNSPECIFIED.,.F.,.F.,(4,3,3,
3,3,3,3,4),(-60.3950510283086,-59.854282378976,-58.856711005993,-57.8591396330101,
-56.8615682600272,-55.8639968870442,-54.8664255140613,-54.111865721129),
 .UNSPECIFIED.);
#2063=B_SPLINE_CURVE_WITH_KNOTS('',3,(#23420,#23421,#23422,#23423,#23424,
#23425,#23426,#23427,#23428,#23429,#23430,#23431,#23432,#23433,#23434,#23435,
#23436,#23437,#23438,#23439,#23440,#23441),.UNSPECIFIED.,.F.,.F.,(4,3,3,
3,3,3,3,4),(51.5753047126087,51.8737113951125,52.8712827680954,53.8688541410784,
54.8664255140613,55.8639968870442,56.8615682600272,57.8584900197883),
 .UNSPECIFIED.);
#2064=B_SPLINE_CURVE_WITH_KNOTS('',3,(#23442,#23443,#23444,#23445,#23446,
#23447,#23448,#23449,#23450,#23451,#23452,#23453,#23454,#23455,#23456,#23457,
#23458,#23459,#23460,#23461,#23462,#23463,#23464,#23465,#23466),
 .UNSPECIFIED.,.F.,.F.,(4,3,3,3,3,3,3,3,4),(-54.111865721129,-53.8688541410784,
-52.8712827680954,-51.8737113951125,-50.8761400221296,-49.8785686491466,
-48.8809972761637,-47.8834259031808,-47.8286804139494),.UNSPECIFIED.);
#2065=B_SPLINE_CURVE_WITH_KNOTS('',3,(#23471,#23472,#23473,#23474,#23475,
#23476,#23477,#23478,#23479,#23480,#23481,#23482,#23483,#23484,#23485,#23486,
#23487,#23488,#23489,#23490,#23491,#23492),.UNSPECIFIED.,.F.,.F.,(4,3,3,
3,3,3,3,4),(45.2921194054291,45.8882831572149,46.8858545301978,47.8834259031808,
48.8809972761637,49.8785686491466,50.8761400221296,51.5753047126087),
 .UNSPECIFIED.);
#2066=B_SPLINE_CURVE_WITH_KNOTS('',3,(#23493,#23494,#23495,#23496,#23497,
#23498,#23499,#23500,#23501,#23502,#23503,#23504,#23505,#23506,#23507,#23508,
#23509,#23510,#23511,#23512,#23513,#23514),.UNSPECIFIED.,.F.,.F.,(4,3,3,
3,3,3,3,4),(-47.8286804139494,-46.8858545301979,-45.8882831572149,-44.890711784232,
-43.893140411249,-42.8955690382661,-41.8979976652832,-41.5454951067698),
 .UNSPECIFIED.);
#2067=B_SPLINE_CURVE_WITH_KNOTS('',3,(#23519,#23520,#23521,#23522,#23523,
#23524,#23525,#23526,#23527,#23528,#23529,#23530,#23531,#23532,#23533,#23534,
#23535,#23536,#23537,#23538,#23539,#23540),.UNSPECIFIED.,.F.,.F.,(4,3,3,
3,3,3,3,4),(39.0089340982495,39.9028549193173,40.9004262923002,41.8979976652832,
42.8955690382661,43.893140411249,44.890711784232,45.2921194054291),
 .UNSPECIFIED.);
#2068=B_SPLINE_CURVE_WITH_KNOTS('',3,(#23541,#23542,#23543,#23544,#23545,
#23546,#23547,#23548,#23549,#23550,#23551,#23552,#23553,#23554,#23555,#23556,
#23557,#23558,#23559,#23560,#23561,#23562),.UNSPECIFIED.,.F.,.F.,(4,3,3,
3,3,3,3,4),(-41.5454951067698,-40.9004262923003,-39.9028549193173,-38.9052835463344,
-37.9077121733515,-36.9101408003685,-35.9125694273856,-35.2623097995902),
 .UNSPECIFIED.);
#2069=B_SPLINE_CURVE_WITH_KNOTS('',3,(#23567,#23568,#23569,#23570,#23571,
#23572,#23573,#23574,#23575,#23576,#23577,#23578,#23579,#23580,#23581,#23582,
#23583,#23584,#23585,#23586,#23587,#23588,#23589,#23590,#23591),
 .UNSPECIFIED.,.F.,.F.,(4,3,3,3,3,3,3,3,4),(32.7257487910699,32.9198553084368,
33.9174266814197,34.9149980544027,35.9125694273856,36.9101408003685,37.9077121733514,
38.9052835463344,39.0089340982495),.UNSPECIFIED.);
#2070=B_SPLINE_CURVE_WITH_KNOTS('',3,(#23592,#23593,#23594,#23595,#23596,
#23597,#23598,#23599,#23600,#23601,#23602,#23603,#23604,#23605,#23606,#23607,
#23608,#23609,#23610,#23611,#23612,#23613),.UNSPECIFIED.,.F.,.F.,(4,3,3,
3,3,3,3,4),(-35.2623097995902,-34.9149980544027,-33.9174266814197,-32.9198553084368,
-31.9222839354538,-30.9247125624709,-29.927141189488,-28.9791244924106),
 .UNSPECIFIED.);
#2071=B_SPLINE_CURVE_WITH_KNOTS('',3,(#23618,#23619,#23620,#23621,#23622,
#23623,#23624,#23625,#23626,#23627,#23628,#23629,#23630,#23631,#23632,#23633,
#23634,#23635,#23636,#23637,#23638,#23639),.UNSPECIFIED.,.F.,.F.,(4,3,3,
3,3,3,3,4),(26.4425634838903,26.9344270705392,27.9319984435221,28.929569816505,
29.927141189488,30.9247125624709,31.9222839354538,32.7257487910699),
 .UNSPECIFIED.);
#2072=B_SPLINE_CURVE_WITH_KNOTS('',3,(#23640,#23641,#23642,#23643,#23644,
#23645,#23646,#23647,#23648,#23649,#23650,#23651,#23652,#23653,#23654,#23655,
#23656,#23657,#23658,#23659,#23660,#23661,#23662,#23663,#23664),
 .UNSPECIFIED.,.F.,.F.,(4,3,3,3,3,3,3,3,4),(-28.9791244924106,-28.929569816505,
-27.9319984435221,-26.9344270705392,-25.9368556975562,-24.9392843245733,
-23.9417129515904,-22.9441415786075,-22.695939185231),.UNSPECIFIED.);
#2073=B_SPLINE_CURVE_WITH_KNOTS('',3,(#23669,#23670,#23671,#23672,#23673,
#23674,#23675,#23676,#23677,#23678,#23679,#23680,#23681,#23682,#23683,#23684,
#23685,#23686,#23687,#23688,#23689,#23690),.UNSPECIFIED.,.F.,.F.,(4,3,3,
3,3,3,3,4),(20.1593781767107,20.9489988326416,21.9465702056245,22.9441415786074,
23.9417129515904,24.9392843245733,25.9368556975562,26.4425634838903),
 .UNSPECIFIED.);
#2074=B_SPLINE_CURVE_WITH_KNOTS('',3,(#23691,#23692,#23693,#23694,#23695,
#23696,#23697,#23698,#23699,#23700,#23701,#23702,#23703,#23704,#23705,#23706,
#23707,#23708,#23709,#23710,#23711,#23712),.UNSPECIFIED.,.F.,.F.,(4,3,3,
3,3,3,3,4),(-22.695939185231,-21.9465702056245,-20.9489988326416,-19.9514274596586,
-18.9538560866757,-17.9562847136928,-16.9587133407099,-16.4127538780514),
 .UNSPECIFIED.);
#2075=B_SPLINE_CURVE_WITH_KNOTS('',3,(#23717,#23718,#23719,#23720,#23721,
#23722,#23723,#23724,#23725,#23726,#23727,#23728,#23729,#23730,#23731,#23732,
#23733,#23734,#23735,#23736,#23737,#23738,#23739,#23740,#23741),
 .UNSPECIFIED.,.F.,.F.,(4,3,3,3,3,3,3,3,4),(13.8761928695311,13.9659992217611,
14.963570594744,15.9611419677269,16.9587133407099,17.9562847136928,18.9538560866757,
19.9514274596586,20.1593781767107),.UNSPECIFIED.);
#2076=B_SPLINE_CURVE_WITH_KNOTS('',3,(#23742,#23743,#23744,#23745,#23746,
#23747,#23748,#23749,#23750,#23751,#23752,#23753,#23754,#23755,#23756,#23757,
#23758,#23759,#23760,#23761,#23762,#23763),.UNSPECIFIED.,.F.,.F.,(4,3,3,
3,3,3,3,4),(-16.4127538780514,-15.9611419677269,-14.963570594744,-13.9659992217611,
-12.9684278487781,-11.9708564757952,-10.9732851028123,-10.1295685708718),
 .UNSPECIFIED.);
#2077=B_SPLINE_CURVE_WITH_KNOTS('',3,(#23769,#23770,#23771,#23772,#23773,
#23774,#23775,#23776,#23777,#23778,#23779,#23780,#23781),.UNSPECIFIED.,
 .F.,.F.,(4,3,3,3,4),(-3.84638326369226,-2.9927141189488,-1.99514274596587,
-0.997571372982931,0.),.UNSPECIFIED.);
#2078=B_SPLINE_CURVE_WITH_KNOTS('',3,(#23784,#23785,#23786,#23787,#23788,
#23789,#23790,#23791,#23792,#23793,#23794,#23795,#23796,#23797,#23798,#23799,
#23800,#23801,#23802),.UNSPECIFIED.,.F.,.F.,(4,3,3,3,3,3,4),(2.01461286527445,
2.9927141189488,3.99028549193173,4.98785686491467,5.9854282378976,6.98299961088053,
7.59300756235155),.UNSPECIFIED.);
#2079=B_SPLINE_CURVE_WITH_KNOTS('',3,(#23808,#23809,#23810,#23811,#23812,
#23813,#23814),.UNSPECIFIED.,.F.,.F.,(4,1,1,1,4),(91.106186954104,91.6672898428913,
92.6648612158742,93.6624325888571,94.6600039618401),.UNSPECIFIED.);
#2080=B_SPLINE_CURVE_WITH_KNOTS('',3,(#23817,#23818,#23819,#23820,#23821,
#23822,#23823,#23824),.UNSPECIFIED.,.F.,.F.,(4,1,1,1,1,4),(91.106186954104,
91.2111367324627,92.2087081054457,93.2062794784286,94.2038508514115,95.1819521050859),
 .UNSPECIFIED.);
#2081=B_SPLINE_CURVE_WITH_KNOTS('',3,(#23829,#23830,#23831,#23832,#23833,
#23834,#23835,#23836,#23837,#23838),.UNSPECIFIED.,.F.,.F.,(4,1,1,1,1,1,
1,4),(84.8230016469244,85.6818616049937,86.6794329779766,87.6770043509595,
88.6745757239425,89.6721470969254,90.6697184699083,91.106186954104),
 .UNSPECIFIED.);
#2082=B_SPLINE_CURVE_WITH_KNOTS('',3,(#23839,#23840,#23841,#23842,#23843,
#23844,#23845,#23846,#23847,#23848),.UNSPECIFIED.,.F.,.F.,(4,1,1,1,1,1,
1,4),(84.8230016469244,85.2257084945651,86.2232798675481,87.220851240531,
88.2184226135139,89.2159939864969,90.2135653594798,91.106186954104),
 .UNSPECIFIED.);
#2083=B_SPLINE_CURVE_WITH_KNOTS('',3,(#23853,#23854,#23855,#23856,#23857,
#23858,#23859,#23860,#23861,#23862,#23863),.UNSPECIFIED.,.F.,.F.,(4,1,1,
1,1,1,1,1,4),(78.5398163397448,78.6988619941132,79.6964333670961,80.694004740079,
81.691576113062,82.6891474860449,83.6867188590278,84.6842902320108,84.8230016469244),
 .UNSPECIFIED.);
#2084=B_SPLINE_CURVE_WITH_KNOTS('',3,(#23864,#23865,#23866,#23867,#23868,
#23869,#23870,#23871,#23872,#23873),.UNSPECIFIED.,.F.,.F.,(4,1,1,1,1,1,
1,4),(78.5398163397448,79.2402802566675,80.2378516296505,81.2354230026334,
82.2329943756163,83.2305657485993,84.2281371215822,84.8230016469244),
 .UNSPECIFIED.);
#2085=B_SPLINE_CURVE_WITH_KNOTS('',3,(#23878,#23879,#23880,#23881,#23882,
#23883,#23884,#23885,#23886,#23887),.UNSPECIFIED.,.F.,.F.,(4,1,1,1,1,1,
1,4),(72.2566310325652,72.7134337562156,73.7110051291985,74.7085765021814,
75.7061478751643,76.7037192481473,77.7012906211302,78.5398163397448),
 .UNSPECIFIED.);
#2086=B_SPLINE_CURVE_WITH_KNOTS('',3,(#23888,#23889,#23890,#23891,#23892,
#23893,#23894,#23895,#23896,#23897,#23898),.UNSPECIFIED.,.F.,.F.,(4,1,1,
1,1,1,1,1,4),(72.2566310325652,72.257280645787,73.2548520187699,74.2524233917529,
75.2499947647358,76.2475661377187,77.2451375107017,78.2427088836846,78.5398163397448),
 .UNSPECIFIED.);
#2087=B_SPLINE_CURVE_WITH_KNOTS('',3,(#23903,#23904,#23905,#23906,#23907,
#23908,#23909,#23910,#23911,#23912),.UNSPECIFIED.,.F.,.F.,(4,1,1,1,1,1,
1,4),(65.9734457253856,66.728005518318,67.7255768913009,68.7231482642838,
69.7207196372668,70.7182910102497,71.7158623832326,72.2566310325652),
 .UNSPECIFIED.);
#2088=B_SPLINE_CURVE_WITH_KNOTS('',3,(#23913,#23914,#23915,#23916,#23917,
#23918,#23919,#23920,#23921,#23922),.UNSPECIFIED.,.F.,.F.,(4,1,1,1,1,1,
1,4),(65.9734457253856,66.2718524078894,67.2694237808723,68.2669951538553,
69.2645665268382,70.2621378998211,71.2597092728041,72.2566310325652),
 .UNSPECIFIED.);
#2089=B_SPLINE_CURVE_WITH_KNOTS('',3,(#23927,#23928,#23929,#23930,#23931,
#23932,#23933,#23934,#23935,#23936,#23937),.UNSPECIFIED.,.F.,.F.,(4,1,1,
1,1,1,1,1,4),(59.690260418206,59.7450059074374,60.7425772804204,61.7401486534033,
62.7377200263862,63.7352913993692,64.7328627723521,65.730434145335,65.9734457253856),
 .UNSPECIFIED.);
#2090=B_SPLINE_CURVE_WITH_KNOTS('',3,(#23938,#23939,#23940,#23941,#23942,
#23943,#23944,#23945,#23946,#23947),.UNSPECIFIED.,.F.,.F.,(4,1,1,1,1,1,
1,4),(59.690260418206,60.2864241699918,61.2839955429747,62.2815669159577,
63.2791382889406,64.2767096619235,65.2742810349065,65.9734457253856),
 .UNSPECIFIED.);
#2091=B_SPLINE_CURVE_WITH_KNOTS('',3,(#23952,#23953,#23954,#23955,#23956,
#23957,#23958,#23959,#23960,#23961),.UNSPECIFIED.,.F.,.F.,(4,1,1,1,1,1,
1,4),(53.4070751110264,53.7595776695398,54.7571490425228,55.7547204155057,
56.7522917884886,57.7498631614716,58.7474345344545,59.690260418206),
 .UNSPECIFIED.);
#2092=B_SPLINE_CURVE_WITH_KNOTS('',3,(#23962,#23963,#23964,#23965,#23966,
#23967,#23968,#23969,#23970,#23971),.UNSPECIFIED.,.F.,.F.,(4,1,1,1,1,1,
1,4),(53.4070751110264,54.3009959320942,55.2985673050771,56.2961386780601,
57.293710051043,58.2912814240259,59.2888527970089,59.690260418206),
 .UNSPECIFIED.);
#2093=B_SPLINE_CURVE_WITH_KNOTS('',3,(#23976,#23977,#23978,#23979,#23980,
#23981,#23982,#23983,#23984,#23985),.UNSPECIFIED.,.F.,.F.,(4,1,1,1,1,1,
1,4),(47.1238898038468,47.7741494316422,48.7717208046252,49.7692921776081,
50.766863550591,51.764434923574,52.7620062965569,53.4070751110264),
 .UNSPECIFIED.);
#2094=B_SPLINE_CURVE_WITH_KNOTS('',3,(#23986,#23987,#23988,#23989,#23990,
#23991,#23992,#23993,#23994,#23995,#23996),.UNSPECIFIED.,.F.,.F.,(4,1,1,
1,1,1,1,1,4),(47.1238898038468,47.3179963212137,48.3155676941966,49.3131390671795,
50.3107104401625,51.3082818131454,52.3058531861283,53.3034245591113,53.4070751110264),
 .UNSPECIFIED.);
#2095=B_SPLINE_CURVE_WITH_KNOTS('',3,(#24001,#24002,#24003,#24004,#24005,
#24006,#24007,#24008,#24009,#24010),.UNSPECIFIED.,.F.,.F.,(4,1,1,1,1,1,
1,4),(40.8407044966673,41.7887211937446,42.7862925667276,43.7838639397105,
44.7814353126934,45.7790066856764,46.7765780586593,47.1238898038468),
 .UNSPECIFIED.);
#2096=B_SPLINE_CURVE_WITH_KNOTS('',3,(#24011,#24012,#24013,#24014,#24015,
#24016,#24017,#24018,#24019,#24020),.UNSPECIFIED.,.F.,.F.,(4,1,1,1,1,1,
1,4),(40.8407044966673,41.3325680833161,42.330139456299,43.3277108292819,
44.3252822022649,45.3228535752478,46.3204249482307,47.1238898038468),
 .UNSPECIFIED.);
#2097=B_SPLINE_CURVE_WITH_KNOTS('',3,(#24025,#24026,#24027,#24028,#24029,
#24030,#24031,#24032,#24033,#24034,#24035),.UNSPECIFIED.,.F.,.F.,(4,1,1,
1,1,1,1,1,4),(34.5575191894876,34.8057215828641,35.803292955847,36.80086432883,
37.7984357018129,38.7960070747958,39.7935784477788,40.7911498207617,40.8407044966673),
 .UNSPECIFIED.);
#2098=B_SPLINE_CURVE_WITH_KNOTS('',3,(#24036,#24037,#24038,#24039,#24040,
#24041,#24042,#24043,#24044,#24045),.UNSPECIFIED.,.F.,.F.,(4,1,1,1,1,1,
1,4),(34.5575191894876,35.3471398454185,36.3447112184014,37.3422825913843,
38.3398539643673,39.3374253373502,40.3349967103331,40.8407044966673),
 .UNSPECIFIED.);
#2099=B_SPLINE_CURVE_WITH_KNOTS('',3,(#24050,#24051,#24052,#24053,#24054,
#24055,#24056,#24057,#24058,#24059),.UNSPECIFIED.,.F.,.F.,(4,1,1,1,1,1,
1,4),(28.2743338823081,28.8202933449665,29.8178647179494,30.8154360909324,
31.8130074639153,32.8105788368982,33.8081502098812,34.5575191894876),
 .UNSPECIFIED.);
#2100=B_SPLINE_CURVE_WITH_KNOTS('',3,(#24060,#24061,#24062,#24063,#24064,
#24065,#24066,#24067,#24068,#24069,#24070),.UNSPECIFIED.,.F.,.F.,(4,1,1,
1,1,1,1,1,4),(28.2743338823081,28.364140234538,29.3617116075209,30.3592829805038,
31.3568543534868,32.3544257264697,33.3519970994526,34.3495684724355,34.5575191894876),
 .UNSPECIFIED.);
#2101=B_SPLINE_CURVE_WITH_KNOTS('',3,(#24075,#24076,#24077,#24078,#24079,
#24080,#24081,#24082,#24083,#24084),.UNSPECIFIED.,.F.,.F.,(4,1,1,1,1,1,
1,4),(21.9911485751285,22.8348651070689,23.8324364800518,24.8300078530348,
25.8275792260177,26.8251505990006,27.8227219719836,28.2743338823081),
 .UNSPECIFIED.);
#2102=B_SPLINE_CURVE_WITH_KNOTS('',3,(#24085,#24086,#24087,#24088,#24089,
#24090,#24091,#24092,#24093,#24094),.UNSPECIFIED.,.F.,.F.,(4,1,1,1,1,1,
1,4),(21.9911485751285,22.3787119966404,23.3762833696233,24.3738547426062,
25.3714261155892,26.3689974885721,27.366568861555,28.2743338823081),
 .UNSPECIFIED.);
#2103=B_SPLINE_CURVE_WITH_KNOTS('',3,(#24100,#24101,#24102,#24103,#24104),
 .UNSPECIFIED.,.F.,.F.,(4,1,4),(14.3981410127769,15.3957123857598,15.7079632679489),
 .UNSPECIFIED.);
#2104=B_SPLINE_CURVE_WITH_KNOTS('',3,(#24107,#24108,#24109,#24110,#24111),
 .UNSPECIFIED.,.F.,.F.,(4,1,4),(13.8761928695311,14.8542941232054,15.7079632679489),
 .UNSPECIFIED.);
#2105=B_SPLINE_CURVE_WITH_KNOTS('',3,(#24117,#24118,#24119,#24120),
 .UNSPECIFIED.,.F.,.F.,(4,4),(114.40689867021,115.117908020989),
 .UNSPECIFIED.);
#2106=B_SPLINE_CURVE_WITH_KNOTS('',3,(#24128,#24129,#24130,#24131,#24132,
#24133,#24134,#24135,#24136,#24137),.UNSPECIFIED.,.F.,.F.,(4,3,3,4),(-113.097335529232,
-112.140720744584,-111.148324985783,-110.666752226423),.UNSPECIFIED.);
#2107=B_SPLINE_CURVE_WITH_KNOTS('',3,(#24142,#24143,#24144,#24145,#24146,
#24147,#24148,#24149,#24150,#24151,#24152,#24153,#24154,#24155,#24156,#24157,
#24158,#24159,#24160,#24161,#24162,#24163,#24164,#24165,#24166),
 .UNSPECIFIED.,.F.,.F.,(4,3,3,3,3,3,3,3,4),(108.12371336303,108.171137709378,
109.16353346818,110.155929226981,111.148324985783,112.140720744584,113.133116503386,
114.125512262188,114.40689867021),.UNSPECIFIED.);
#2108=B_SPLINE_CURVE_WITH_KNOTS('',3,(#24167,#24168,#24169,#24170,#24171,
#24172,#24173,#24174,#24175,#24176,#24177,#24178,#24179,#24180,#24181,#24182,
#24183,#24184,#24185,#24186,#24187,#24188),.UNSPECIFIED.,.F.,.F.,(4,3,3,
3,3,3,3,4),(-110.666752226423,-110.155929226981,-109.16353346818,-108.171137709378,
-107.178741950576,-106.186346191775,-105.193950432973,-104.383566919243),
 .UNSPECIFIED.);
#2109=B_SPLINE_CURVE_WITH_KNOTS('',3,(#24193,#24194,#24195,#24196,#24197,
#24198,#24199,#24200,#24201,#24202,#24203,#24204,#24205,#24206,#24207,#24208,
#24209,#24210,#24211,#24212,#24213,#24214),.UNSPECIFIED.,.F.,.F.,(4,3,3,
3,3,3,3,4),(101.84052805585,102.216763156568,103.20915891537,104.201554674171,
105.193950432973,106.186346191775,107.178741950576,108.12371336303),
 .UNSPECIFIED.);
#2110=B_SPLINE_CURVE_WITH_KNOTS('',3,(#24215,#24216,#24217,#24218,#24219,
#24220,#24221,#24222,#24223,#24224,#24225,#24226,#24227,#24228,#24229,#24230,
#24231,#24232,#24233,#24234,#24235,#24236,#24237,#24238,#24239),
 .UNSPECIFIED.,.F.,.F.,(4,3,3,3,3,3,3,3,4),(-104.383566919243,-104.201554674171,
-103.20915891537,-102.216763156568,-101.224367397767,-100.231971638965,
-99.2395758801633,-98.2471801213616,-98.1003816120635),.UNSPECIFIED.);
#2111=B_SPLINE_CURVE_WITH_KNOTS('',3,(#24244,#24245,#24246,#24247,#24248,
#24249,#24250,#24251,#24252,#24253,#24254,#24255,#24256,#24257,#24258,#24259,
#24260,#24261,#24262,#24263,#24264,#24265),.UNSPECIFIED.,.F.,.F.,(4,3,3,
3,3,3,3,4),(95.5573427486709,96.2623886037584,97.25478436256,98.2471801213616,
99.2395758801633,100.231971638965,101.224367397767,101.84052805585),
 .UNSPECIFIED.);
#2112=B_SPLINE_CURVE_WITH_KNOTS('',3,(#24266,#24267,#24268,#24269,#24270,
#24271,#24272,#24273,#24274,#24275,#24276,#24277,#24278,#24279,#24280,#24281,
#24282,#24283,#24284,#24285,#24286,#24287),.UNSPECIFIED.,.F.,.F.,(4,3,3,
3,3,3,3,4),(-98.1003816120635,-97.25478436256,-96.2623886037584,-95.2699928449567,
-94.2775970861551,-93.2852013273535,-92.2928055685519,-91.8171963048839),
 .UNSPECIFIED.);
#2113=B_SPLINE_CURVE_WITH_KNOTS('',3,(#24292,#24293,#24294,#24295,#24296,
#24297,#24298,#24299,#24300,#24301,#24302,#24303,#24304,#24305,#24306,#24307,
#24308,#24309,#24310,#24311,#24312,#24313,#24314,#24315,#24316),
 .UNSPECIFIED.,.F.,.F.,(4,3,3,3,3,3,3,3,4),(89.2741574414912,89.3156182921469,
90.3080140509486,91.3004098097502,92.2928055685518,93.2852013273535,94.2775970861551,
95.2699928449567,95.5573427486709),.UNSPECIFIED.);
#2114=B_SPLINE_CURVE_WITH_KNOTS('',3,(#24317,#24318,#24319,#24320,#24321,
#24322,#24323,#24324,#24325,#24326,#24327,#24328,#24329,#24330,#24331,#24332,
#24333,#24334,#24335,#24336,#24337,#24338),.UNSPECIFIED.,.F.,.F.,(4,3,3,
3,3,3,3,4),(-91.8171963048839,-91.3004098097502,-90.3080140509486,-89.315618292147,
-88.3232225333453,-87.3308267745437,-86.338431015742,-85.5340109977043),
 .UNSPECIFIED.);
#2115=B_SPLINE_CURVE_WITH_KNOTS('',3,(#24343,#24344,#24345,#24346,#24347,
#24348,#24349,#24350,#24351,#24352,#24353,#24354,#24355,#24356,#24357,#24358,
#24359,#24360,#24361,#24362,#24363,#24364),.UNSPECIFIED.,.F.,.F.,(4,3,3,
3,3,3,3,4),(82.9909721343117,83.3612437393372,84.3536394981388,85.3460352569404,
86.338431015742,87.3308267745437,88.3232225333453,89.2741574414912),
 .UNSPECIFIED.);
#2116=B_SPLINE_CURVE_WITH_KNOTS('',3,(#24365,#24366,#24367,#24368,#24369,
#24370,#24371,#24372,#24373,#24374,#24375,#24376,#24377,#24378,#24379,#24380,
#24381,#24382,#24383,#24384,#24385,#24386,#24387,#24388,#24389),
 .UNSPECIFIED.,.F.,.F.,(4,3,3,3,3,3,3,3,4),(-85.5340109977043,-85.3460352569404,
-84.3536394981388,-83.3612437393372,-82.3688479805355,-81.3764522217339,
-80.3840564629323,-79.3916607041306,-79.2508256905247),.UNSPECIFIED.);
#2117=B_SPLINE_CURVE_WITH_KNOTS('',3,(#24394,#24395,#24396,#24397,#24398,
#24399,#24400,#24401,#24402,#24403,#24404,#24405,#24406,#24407,#24408,#24409,
#24410,#24411,#24412,#24413,#24414,#24415),.UNSPECIFIED.,.F.,.F.,(4,3,3,
3,3,3,3,4),(76.7077868271321,77.4068691865273,78.399264945329,79.3916607041306,
80.3840564629322,81.3764522217339,82.3688479805355,82.9909721343117),
 .UNSPECIFIED.);
#2118=B_SPLINE_CURVE_WITH_KNOTS('',3,(#24416,#24417,#24418,#24419,#24420,
#24421,#24422,#24423,#24424,#24425,#24426,#24427,#24428,#24429,#24430,#24431,
#24432,#24433,#24434,#24435,#24436,#24437),.UNSPECIFIED.,.F.,.F.,(4,3,3,
3,3,3,3,4),(-79.2508256905247,-78.399264945329,-77.4068691865274,-76.4144734277257,
-75.4220776689241,-74.4296819101224,-73.4372861513208,-72.9676403833451),
 .UNSPECIFIED.);
#2119=B_SPLINE_CURVE_WITH_KNOTS('',3,(#24442,#24443,#24444,#24445,#24446,
#24447,#24448,#24449,#24450,#24451,#24452,#24453,#24454,#24455,#24456,#24457,
#24458,#24459,#24460,#24461,#24462,#24463,#24464,#24465,#24466),
 .UNSPECIFIED.,.F.,.F.,(4,3,3,3,3,3,3,3,4),(70.4246015199525,70.4600988749159,
71.4524946337175,72.4448903925192,73.4372861513208,74.4296819101224,75.4220776689241,
76.4144734277257,76.7077868271321),.UNSPECIFIED.);
#2120=B_SPLINE_CURVE_WITH_KNOTS('',3,(#24467,#24468,#24469,#24470,#24471,
#24472,#24473,#24474,#24475,#24476,#24477,#24478,#24479,#24480,#24481,#24482,
#24483,#24484,#24485,#24486,#24487,#24488),.UNSPECIFIED.,.F.,.F.,(4,3,3,
3,3,3,3,4),(-72.9676403833451,-72.4448903925192,-71.4524946337175,-70.4600988749159,
-69.4677031161143,-68.4753073573127,-67.482911598511,-66.6844550761655),
 .UNSPECIFIED.);
#2121=B_SPLINE_CURVE_WITH_KNOTS('',3,(#24493,#24494,#24495,#24496,#24497,
#24498,#24499,#24500,#24501,#24502,#24503,#24504,#24505,#24506,#24507,#24508,
#24509,#24510,#24511,#24512,#24513,#24514),.UNSPECIFIED.,.F.,.F.,(4,3,3,
3,3,3,3,4),(64.1414162127729,64.5057243221061,65.4981200809078,66.4905158397094,
67.482911598511,68.4753073573126,69.4677031161143,70.4246015199525),
 .UNSPECIFIED.);
#2122=B_SPLINE_CURVE_WITH_KNOTS('',3,(#24515,#24516,#24517,#24518,#24519,
#24520,#24521,#24522,#24523,#24524,#24525,#24526,#24527,#24528,#24529,#24530,
#24531,#24532,#24533,#24534,#24535,#24536,#24537,#24538,#24539),
 .UNSPECIFIED.,.F.,.F.,(4,3,3,3,3,3,3,3,4),(-66.6844550761655,-66.4905158397094,
-65.4981200809078,-64.5057243221061,-63.5133285633045,-62.5209328045029,
-61.5285370457012,-60.5361412868996,-60.4012697689859),.UNSPECIFIED.);
#2123=B_SPLINE_CURVE_WITH_KNOTS('',3,(#24544,#24545,#24546,#24547,#24548,
#24549,#24550,#24551,#24552,#24553,#24554,#24555,#24556,#24557,#24558,#24559,
#24560,#24561,#24562,#24563,#24564,#24565),.UNSPECIFIED.,.F.,.F.,(4,3,3,
3,3,3,3,4),(57.8582309055933,58.5513497692963,59.543745528098,60.5361412868996,
61.5285370457012,62.5209328045029,63.5133285633045,64.1414162127729),
 .UNSPECIFIED.);
#2124=B_SPLINE_CURVE_WITH_KNOTS('',3,(#24566,#24567,#24568,#24569,#24570,
#24571,#24572,#24573,#24574,#24575,#24576,#24577,#24578,#24579,#24580,#24581,
#24582,#24583,#24584,#24585,#24586,#24587),.UNSPECIFIED.,.F.,.F.,(4,3,3,
3,3,3,3,4),(-60.4012697689859,-59.543745528098,-58.5513497692964,-57.5589540104947,
-56.5665582516931,-55.5741624928914,-54.5817667340898,-54.1180844618063),
 .UNSPECIFIED.);
#2125=B_SPLINE_CURVE_WITH_KNOTS('',3,(#24592,#24593,#24594,#24595,#24596,
#24597,#24598,#24599,#24600,#24601,#24602,#24603,#24604,#24605,#24606,#24607,
#24608,#24609,#24610,#24611,#24612,#24613,#24614,#24615,#24616),
 .UNSPECIFIED.,.F.,.F.,(4,3,3,3,3,3,3,3,4),(51.5750455984137,51.6045794576849,
52.5969752164865,53.5893709752882,54.5817667340898,55.5741624928914,56.5665582516931,
57.5589540104947,57.8582309055933),.UNSPECIFIED.);
#2126=B_SPLINE_CURVE_WITH_KNOTS('',3,(#24617,#24618,#24619,#24620,#24621,
#24622,#24623,#24624,#24625,#24626,#24627,#24628,#24629,#24630,#24631,#24632,
#24633,#24634,#24635,#24636,#24637,#24638),.UNSPECIFIED.,.F.,.F.,(4,3,3,
3,3,3,3,4),(-54.1180844618063,-53.5893709752882,-52.5969752164865,-51.6045794576849,
-50.6121836988833,-49.6197879400816,-48.62739218128,-47.8348991546267),
 .UNSPECIFIED.);
#2127=B_SPLINE_CURVE_WITH_KNOTS('',3,(#24643,#24644,#24645,#24646,#24647,
#24648,#24649,#24650,#24651,#24652,#24653,#24654,#24655,#24656,#24657,#24658,
#24659,#24660,#24661,#24662,#24663,#24664),.UNSPECIFIED.,.F.,.F.,(4,3,3,
3,3,3,3,4),(45.2918602912341,45.6502049048751,46.6426006636767,47.6349964224784,
48.62739218128,49.6197879400816,50.6121836988833,51.5750455984137),
 .UNSPECIFIED.);
#2128=B_SPLINE_CURVE_WITH_KNOTS('',3,(#24665,#24666,#24667,#24668,#24669,
#24670,#24671,#24672,#24673,#24674,#24675,#24676,#24677,#24678,#24679,#24680,
#24681,#24682,#24683,#24684,#24685,#24686,#24687,#24688,#24689),
 .UNSPECIFIED.,.F.,.F.,(4,3,3,3,3,3,3,3,4),(-47.8348991546267,-47.6349964224784,
-46.6426006636767,-45.6502049048751,-44.6578091460735,-43.6654133872718,
-42.6730176284702,-41.6806218696686,-41.5517138474472),.UNSPECIFIED.);
#2129=B_SPLINE_CURVE_WITH_KNOTS('',3,(#24694,#24695,#24696,#24697,#24698,
#24699,#24700,#24701,#24702,#24703,#24704,#24705,#24706,#24707,#24708,#24709,
#24710,#24711,#24712,#24713,#24714,#24715),.UNSPECIFIED.,.F.,.F.,(4,3,3,
3,3,3,3,4),(39.0086749840545,39.6958303520653,40.6882261108669,41.6806218696686,
42.6730176284702,43.6654133872718,44.6578091460735,45.2918602912341),
 .UNSPECIFIED.);
#2130=B_SPLINE_CURVE_WITH_KNOTS('',3,(#24716,#24717,#24718,#24719,#24720,
#24721,#24722,#24723,#24724,#24725,#24726,#24727,#24728,#24729,#24730,#24731,
#24732,#24733,#24734,#24735,#24736,#24737),.UNSPECIFIED.,.F.,.F.,(4,3,3,
3,3,3,3,4),(-41.5517138474472,-40.6882261108669,-39.6958303520653,-38.7034345932637,
-37.711038834462,-36.7186430756604,-35.7262473168588,-35.2685285402675),
 .UNSPECIFIED.);
#2131=B_SPLINE_CURVE_WITH_KNOTS('',3,(#24742,#24743,#24744,#24745,#24746,
#24747,#24748,#24749,#24750,#24751,#24752,#24753,#24754,#24755,#24756,#24757,
#24758,#24759,#24760,#24761,#24762,#24763,#24764,#24765,#24766),
 .UNSPECIFIED.,.F.,.F.,(4,3,3,3,3,3,3,3,4),(32.725489676875,32.7490600404539,
33.7414557992555,34.7338515580571,35.7262473168588,36.7186430756604,37.711038834462,
38.7034345932637,39.0086749840545),.UNSPECIFIED.);
#2132=B_SPLINE_CURVE_WITH_KNOTS('',3,(#24767,#24768,#24769,#24770,#24771,
#24772,#24773,#24774,#24775,#24776,#24777,#24778,#24779,#24780,#24781,#24782,
#24783,#24784,#24785,#24786,#24787,#24788),.UNSPECIFIED.,.F.,.F.,(4,3,3,
3,3,3,3,4),(-35.2685285402675,-34.7338515580572,-33.7414557992555,-32.7490600404539,
-31.7566642816523,-30.7642685228506,-29.771872764049,-28.985343233088),
 .UNSPECIFIED.);
#2133=B_SPLINE_CURVE_WITH_KNOTS('',3,(#24793,#24794,#24795,#24796,#24797,
#24798,#24799,#24800,#24801,#24802,#24803,#24804,#24805,#24806,#24807,#24808,
#24809,#24810,#24811,#24812,#24813,#24814),.UNSPECIFIED.,.F.,.F.,(4,3,3,
3,3,3,3,4),(26.4423043696953,26.7946854876441,27.7870812464457,28.7794770052473,
29.771872764049,30.7642685228506,31.7566642816522,32.725489676875),
 .UNSPECIFIED.);
#2134=B_SPLINE_CURVE_WITH_KNOTS('',3,(#24815,#24816,#24817,#24818,#24819,
#24820,#24821,#24822,#24823,#24824,#24825,#24826,#24827,#24828,#24829,#24830,
#24831,#24832,#24833,#24834,#24835,#24836,#24837,#24838,#24839),
 .UNSPECIFIED.,.F.,.F.,(4,3,3,3,3,3,3,3,4),(-28.985343233088,-28.7794770052474,
-27.7870812464457,-26.7946854876441,-25.8022897288425,-24.8098939700408,
-23.8174982112392,-22.8251024524376,-22.7021579259084),.UNSPECIFIED.);
#2135=B_SPLINE_CURVE_WITH_KNOTS('',3,(#24844,#24845,#24846,#24847,#24848,
#24849,#24850,#24851,#24852,#24853,#24854,#24855,#24856,#24857,#24858,#24859,
#24860,#24861,#24862,#24863,#24864,#24865),.UNSPECIFIED.,.F.,.F.,(4,3,3,
3,3,3,3,4),(20.1591190625158,20.8403109348343,21.8327066936359,22.8251024524376,
23.8174982112392,24.8098939700408,25.8022897288424,26.4423043696953),
 .UNSPECIFIED.);
#2136=B_SPLINE_CURVE_WITH_KNOTS('',3,(#24866,#24867,#24868,#24869,#24870,
#24871,#24872,#24873,#24874,#24875,#24876,#24877,#24878,#24879,#24880,#24881,
#24882,#24883,#24884,#24885,#24886,#24887),.UNSPECIFIED.,.F.,.F.,(4,3,3,
3,3,3,3,4),(-22.7021579259084,-21.8327066936359,-20.8403109348343,-19.8479151760327,
-18.855519417231,-17.8631236584294,-16.8707278996278,-16.4189726187288),
 .UNSPECIFIED.);
#2137=B_SPLINE_CURVE_WITH_KNOTS('',3,(#24892,#24893,#24894,#24895,#24896,
#24897,#24898,#24899,#24900,#24901,#24902,#24903,#24904,#24905,#24906,#24907,
#24908,#24909,#24910,#24911,#24912,#24913,#24914,#24915,#24916),
 .UNSPECIFIED.,.F.,.F.,(4,3,3,3,3,3,3,3,4),(13.8759337553361,13.8935406232229,
14.8859363820245,15.8783321408261,16.8707278996278,17.8631236584294,18.855519417231,
19.8479151760327,20.1591190625158),.UNSPECIFIED.);
#2138=B_SPLINE_CURVE_WITH_KNOTS('',3,(#24917,#24918,#24919,#24920,#24921,
#24922,#24923,#24924,#24925,#24926,#24927,#24928,#24929,#24930,#24931,#24932,
#24933,#24934,#24935,#24936,#24937,#24938),.UNSPECIFIED.,.F.,.F.,(4,3,3,
3,3,3,3,4),(-16.4189726187288,-15.8783321408261,-14.8859363820245,-13.8935406232229,
-12.9011448644212,-11.9087491056196,-10.916353346818,-10.1357873115492),
 .UNSPECIFIED.);
#2139=B_SPLINE_CURVE_WITH_KNOTS('',3,(#24944,#24945,#24946,#24947,#24948,
#24949,#24950,#24951,#24952,#24953,#24954,#24955,#24956),.UNSPECIFIED.,
 .F.,.F.,(4,3,3,3,4),(-3.85260200436961,-2.9771872764049,-1.98479151760327,
-0.992395758801633,0.),.UNSPECIFIED.);
#2140=B_SPLINE_CURVE_WITH_KNOTS('',3,(#24959,#24960,#24961,#24962,#24963,
#24964,#24965,#24966,#24967,#24968,#24969,#24970,#24971,#24972,#24973,#24974,
#24975,#24976,#24977),.UNSPECIFIED.,.F.,.F.,(4,3,3,3,3,3,4),(2.0205724917569,
2.9771872764049,3.96958303520653,4.96197879400816,5.9543745528098,6.94677031161143,
7.59274844815659),.UNSPECIFIED.);
#2141=B_SPLINE_CURVE_WITH_KNOTS('',3,(#24983,#24984,#24985,#24986,#24987,
#24988,#24989,#24990),.UNSPECIFIED.,.F.,.F.,(4,1,1,1,1,4),(122.522113490002,
123.003686249362,123.996082008164,124.988477766965,125.980873525767,126.973269284569),
 .UNSPECIFIED.);
#2142=B_SPLINE_CURVE_WITH_KNOTS('',3,(#24993,#24994,#24995,#24996,#24997,
#24998,#24999,#25000,#25001),.UNSPECIFIED.,.F.,.F.,(4,1,1,1,1,1,4),(122.522113490002,
122.56953783635,123.561933595151,124.554329353953,125.546725112755,126.539120871556,
127.495735656204),.UNSPECIFIED.);
#2143=B_SPLINE_CURVE_WITH_KNOTS('',3,(#25006,#25007,#25008,#25009,#25010,
#25011,#25012,#25013,#25014,#25015),.UNSPECIFIED.,.F.,.F.,(4,1,1,1,1,1,
1,4),(116.238928182822,117.049311696552,118.041707455354,119.034103214156,
120.026498972957,121.018894731759,122.01129049056,122.522113490002),
 .UNSPECIFIED.);
#2144=B_SPLINE_CURVE_WITH_KNOTS('',3,(#25016,#25017,#25018,#25019,#25020,
#25021,#25022,#25023,#25024,#25025),.UNSPECIFIED.,.F.,.F.,(4,1,1,1,1,1,
1,4),(116.238928182822,116.61516328354,117.607559042342,118.599954801143,
119.592350559945,120.584746318746,121.577142077548,122.522113490002),
 .UNSPECIFIED.);
#2145=B_SPLINE_CURVE_WITH_KNOTS('',3,(#25030,#25031,#25032,#25033,#25034,
#25035,#25036,#25037,#25038,#25039,#25040),.UNSPECIFIED.,.F.,.F.,(4,1,1,
1,1,1,1,1,4),(109.955742875643,110.102541384941,111.094937143743,112.087332902544,
113.079728661346,114.072124420147,115.064520178949,116.056915937751,116.238928182822),
 .UNSPECIFIED.);
#2146=B_SPLINE_CURVE_WITH_KNOTS('',3,(#25041,#25042,#25043,#25044,#25045,
#25046,#25047,#25048,#25049,#25050),.UNSPECIFIED.,.F.,.F.,(4,1,1,1,1,1,
1,4),(109.955742875643,110.66078873073,111.653184489532,112.645580248333,
113.637976007135,114.630371765937,115.622767524738,116.238928182822),
 .UNSPECIFIED.);
#2147=B_SPLINE_CURVE_WITH_KNOTS('',3,(#25055,#25056,#25057,#25058,#25059,
#25060,#25061,#25062,#25063,#25064),.UNSPECIFIED.,.F.,.F.,(4,1,1,1,1,1,
1,4),(103.672557568463,104.148166832131,105.140562590933,106.132958349734,
107.125354108536,108.117749867338,109.110145626139,109.955742875643),
 .UNSPECIFIED.);
#2148=B_SPLINE_CURVE_WITH_KNOTS('',3,(#25065,#25066,#25067,#25068,#25069,
#25070,#25071,#25072,#25073,#25074,#25075),.UNSPECIFIED.,.F.,.F.,(4,1,1,
1,1,1,1,1,4),(103.672557568463,103.714018419119,104.70641417792,105.698809936722,
106.691205695524,107.683601454325,108.675997213127,109.668392971929,109.955742875643),
 .UNSPECIFIED.);
#2149=B_SPLINE_CURVE_WITH_KNOTS('',3,(#25080,#25081,#25082,#25083,#25084,
#25085,#25086,#25087,#25088,#25089),.UNSPECIFIED.,.F.,.F.,(4,1,1,1,1,1,
1,4),(97.3893722612835,98.1937922793213,99.1861880381229,100.178583796925,
101.170979555726,102.163375314528,103.155771073329,103.672557568463),
 .UNSPECIFIED.);
#2150=B_SPLINE_CURVE_WITH_KNOTS('',3,(#25090,#25091,#25092,#25093,#25094,
#25095,#25096,#25097,#25098,#25099),.UNSPECIFIED.,.F.,.F.,(4,1,1,1,1,1,
1,4),(97.3893722612835,97.7596438663089,98.7520396251105,99.7444353839122,
100.736831142714,101.729226901515,102.721622660317,103.672557568463),
 .UNSPECIFIED.);
#2151=B_SPLINE_CURVE_WITH_KNOTS('',3,(#25104,#25105,#25106,#25107,#25108,
#25109,#25110,#25111,#25112,#25113,#25114),.UNSPECIFIED.,.F.,.F.,(4,1,1,
1,1,1,1,1,4),(91.106186954104,91.2470219677099,92.2394177265115,93.2318134853131,
94.2242092441148,95.2166050029164,96.209000761718,97.2013965205197,97.3893722612835),
 .UNSPECIFIED.);
#2152=B_SPLINE_CURVE_WITH_KNOTS('',3,(#25115,#25116,#25117,#25118,#25119,
#25120,#25121,#25122,#25123,#25124),.UNSPECIFIED.,.F.,.F.,(4,1,1,1,1,1,
1,4),(91.106186954104,91.8052693134991,92.7976650723007,93.7900608311024,
94.782456589904,95.7748523487057,96.7672481075073,97.3893722612835),
 .UNSPECIFIED.);
#2153=B_SPLINE_CURVE_WITH_KNOTS('',3,(#25129,#25130,#25131,#25132,#25133,
#25134,#25135,#25136,#25137,#25138),.UNSPECIFIED.,.F.,.F.,(4,1,1,1,1,1,
1,4),(84.8230016469243,85.2926474149001,86.2850431737017,87.2774389325033,
88.269834691305,89.2622304501066,90.2546262089082,91.106186954104),
 .UNSPECIFIED.);
#2154=B_SPLINE_CURVE_WITH_KNOTS('',3,(#25139,#25140,#25141,#25142,#25143,
#25144,#25145,#25146,#25147,#25148,#25149),.UNSPECIFIED.,.F.,.F.,(4,1,1,
1,1,1,1,1,4),(84.8230016469243,84.8584990018877,85.8508947606893,86.8432905194909,
87.8356862782926,88.8280820370942,89.8204777958959,90.8128735546975,91.106186954104),
 .UNSPECIFIED.);
#2155=B_SPLINE_CURVE_WITH_KNOTS('',3,(#25154,#25155,#25156,#25157,#25158,
#25159,#25160,#25161,#25162,#25163),.UNSPECIFIED.,.F.,.F.,(4,1,1,1,1,1,
1,4),(78.5398163397448,79.3382728620903,80.3306686208919,81.3230643796935,
82.3154601384952,83.3078558972968,84.3002516560985,84.8230016469243),
 .UNSPECIFIED.);
#2156=B_SPLINE_CURVE_WITH_KNOTS('',3,(#25164,#25165,#25166,#25167,#25168,
#25169,#25170,#25171,#25172,#25173),.UNSPECIFIED.,.F.,.F.,(4,1,1,1,1,1,
1,4),(78.5398163397448,78.9041244490779,79.8965202078795,80.8889159666812,
81.8813117254828,82.8737074842844,83.8661032430861,84.8230016469243),
 .UNSPECIFIED.);
#2157=B_SPLINE_CURVE_WITH_KNOTS('',3,(#25178,#25179,#25180,#25181,#25182,
#25183,#25184,#25185,#25186,#25187,#25188),.UNSPECIFIED.,.F.,.F.,(4,1,1,
1,1,1,1,1,4),(72.2566310325651,72.3915025504788,73.3838983092805,74.3762940680821,
75.3686898268838,76.3610855856854,77.353481344487,78.3458771032886,78.5398163397448),
 .UNSPECIFIED.);
#2158=B_SPLINE_CURVE_WITH_KNOTS('',3,(#25189,#25190,#25191,#25192,#25193,
#25194,#25195,#25196,#25197,#25198),.UNSPECIFIED.,.F.,.F.,(4,1,1,1,1,1,
1,4),(72.2566310325651,72.9497498962681,73.9421456550697,74.9345414138714,
75.926937172673,76.9193329314746,77.9117286902763,78.5398163397448),
 .UNSPECIFIED.);
#2159=B_SPLINE_CURVE_WITH_KNOTS('',3,(#25203,#25204,#25205,#25206,#25207,
#25208,#25209,#25210,#25211,#25212),.UNSPECIFIED.,.F.,.F.,(4,1,1,1,1,1,
1,4),(65.9734457253856,66.4371279976691,67.4295237564707,68.4219195152723,
69.4143152740739,70.4067110328756,71.3991067916772,72.2566310325651),
 .UNSPECIFIED.);
#2160=B_SPLINE_CURVE_WITH_KNOTS('',3,(#25213,#25214,#25215,#25216,#25217,
#25218,#25219,#25220,#25221,#25222,#25223),.UNSPECIFIED.,.F.,.F.,(4,1,1,
1,1,1,1,1,4),(65.9734457253856,66.0029795846567,66.9953753434583,67.9877711022599,
68.9801668610616,69.9725626198632,70.9649583786648,71.9573541374665,72.2566310325651),
 .UNSPECIFIED.);
#2161=B_SPLINE_CURVE_WITH_KNOTS('',3,(#25228,#25229,#25230,#25231,#25232,
#25233,#25234,#25235,#25236,#25237),.UNSPECIFIED.,.F.,.F.,(4,1,1,1,1,1,
1,4),(59.690260418206,60.4827534448593,61.4751492036609,62.4675449624625,
63.4599407212642,64.4523364800658,65.4447322388674,65.9734457253856),
 .UNSPECIFIED.);
#2162=B_SPLINE_CURVE_WITH_KNOTS('',3,(#25238,#25239,#25240,#25241,#25242,
#25243,#25244,#25245,#25246,#25247),.UNSPECIFIED.,.F.,.F.,(4,1,1,1,1,1,
1,4),(59.690260418206,60.0486050318469,61.0410007906485,62.0333965494501,
63.0257923082518,64.0181880670534,65.010583825855,65.9734457253856),
 .UNSPECIFIED.);
#2163=B_SPLINE_CURVE_WITH_KNOTS('',3,(#25252,#25253,#25254,#25255,#25256,
#25257,#25258,#25259,#25260,#25261,#25262),.UNSPECIFIED.,.F.,.F.,(4,1,1,
1,1,1,1,1,4),(53.4070751110264,53.5359831332478,54.5283788920495,55.5207746508511,
56.5131704096527,57.5055661684544,58.497961927256,59.4903576860576,59.690260418206),
 .UNSPECIFIED.);
#2164=B_SPLINE_CURVE_WITH_KNOTS('',3,(#25263,#25264,#25265,#25266,#25267,
#25268,#25269,#25270,#25271,#25272),.UNSPECIFIED.,.F.,.F.,(4,1,1,1,1,1,
1,4),(53.4070751110264,54.0942304790371,55.0866262378387,56.0790219966403,
57.071417755442,58.0638135142436,59.0562092730452,59.690260418206),
 .UNSPECIFIED.);
#2165=B_SPLINE_CURVE_WITH_KNOTS('',3,(#25277,#25278,#25279,#25280,#25281,
#25282,#25283,#25284,#25285,#25286),.UNSPECIFIED.,.F.,.F.,(4,1,1,1,1,1,
1,4),(47.1238898038468,47.581608580438,48.5740043392397,49.5664000980413,
50.5587958568429,51.5511916156446,52.5435873744462,53.4070751110264),
 .UNSPECIFIED.);
#2166=B_SPLINE_CURVE_WITH_KNOTS('',3,(#25287,#25288,#25289,#25290,#25291,
#25292,#25293,#25294,#25295,#25296,#25297),.UNSPECIFIED.,.F.,.F.,(4,1,1,
1,1,1,1,1,4),(47.1238898038468,47.1474601674257,48.1398559262273,49.1322516850289,
50.1246474438306,51.1170432026322,52.1094389614338,53.1018347202355,53.4070751110264),
 .UNSPECIFIED.);
#2167=B_SPLINE_CURVE_WITH_KNOTS('',3,(#25302,#25303,#25304,#25305,#25306,
#25307,#25308,#25309,#25310,#25311),.UNSPECIFIED.,.F.,.F.,(4,1,1,1,1,1,
1,4),(40.8407044966672,41.6272340276282,42.6196297864299,43.6120255452315,
44.6044213040331,45.5968170628348,46.5892128216364,47.1238898038468),
 .UNSPECIFIED.);
#2168=B_SPLINE_CURVE_WITH_KNOTS('',3,(#25312,#25313,#25314,#25315,#25316,
#25317,#25318,#25319,#25320,#25321),.UNSPECIFIED.,.F.,.F.,(4,1,1,1,1,1,
1,4),(40.8407044966672,41.1930856146159,42.1854813734175,43.1778771322191,
44.1702728910208,45.1626686498224,46.155064408624,47.1238898038468),
 .UNSPECIFIED.);
#2169=B_SPLINE_CURVE_WITH_KNOTS('',3,(#25326,#25327,#25328,#25329,#25330,
#25331,#25332,#25333,#25334,#25335,#25336),.UNSPECIFIED.,.F.,.F.,(4,1,1,
1,1,1,1,1,4),(34.5575191894876,34.6804637160168,35.6728594748184,36.6652552336201,
37.6576509924217,38.6500467512233,39.642442510025,40.6348382688266,40.8407044966672),
 .UNSPECIFIED.);
#2170=B_SPLINE_CURVE_WITH_KNOTS('',3,(#25337,#25338,#25339,#25340,#25341,
#25342,#25343,#25344,#25345,#25346),.UNSPECIFIED.,.F.,.F.,(4,1,1,1,1,1,
1,4),(34.5575191894876,35.2387110618061,36.2311068206077,37.2235025794093,
38.215898338211,39.2082940970126,40.2006898558142,40.8407044966672),
 .UNSPECIFIED.);
#2171=B_SPLINE_CURVE_WITH_KNOTS('',3,(#25351,#25352,#25353,#25354,#25355,
#25356,#25357,#25358,#25359,#25360),.UNSPECIFIED.,.F.,.F.,(4,1,1,1,1,1,
1,4),(28.274333882308,28.726089163207,29.7184849220086,30.7108806808103,
31.7032764396119,32.6956721984135,33.6880679572152,34.5575191894876),
 .UNSPECIFIED.);
#2172=B_SPLINE_CURVE_WITH_KNOTS('',3,(#25361,#25362,#25363,#25364,#25365,
#25366,#25367,#25368,#25369,#25370,#25371),.UNSPECIFIED.,.F.,.F.,(4,1,1,
1,1,1,1,1,4),(28.274333882308,28.2919407501946,29.2843365089963,30.2767322677979,
31.2691280265995,32.2615237854012,33.2539195442028,34.2463153030044,34.5575191894876),
 .UNSPECIFIED.);
#2173=B_SPLINE_CURVE_WITH_KNOTS('',3,(#25376,#25377,#25378,#25379,#25380,
#25381,#25382,#25383,#25384,#25385),.UNSPECIFIED.,.F.,.F.,(4,1,1,1,1,1,
1,4),(21.9911485751284,22.7717146103972,23.7641103691988,24.7565061280005,
25.7489018868021,26.7412976456037,27.7336934044054,28.274333882308),
 .UNSPECIFIED.);
#2174=B_SPLINE_CURVE_WITH_KNOTS('',3,(#25386,#25387,#25388,#25389,#25390,
#25391,#25392,#25393,#25394,#25395),.UNSPECIFIED.,.F.,.F.,(4,1,1,1,1,1,
1,4),(21.9911485751284,22.3375661973848,23.3299619561865,24.3223577149881,
25.3147534737897,26.3071492325914,27.299544991393,28.274333882308),
 .UNSPECIFIED.);
#2175=B_SPLINE_CURVE_WITH_KNOTS('',3,(#25401,#25402,#25403,#25404,#25405),
 .UNSPECIFIED.,.F.,.F.,(4,1,4),(14.3984001269718,15.3907958857734,15.7079632679489),
 .UNSPECIFIED.);
#2176=B_SPLINE_CURVE_WITH_KNOTS('',3,(#25408,#25409,#25410,#25411,#25412),
 .UNSPECIFIED.,.F.,.F.,(4,1,4),(13.8759337553361,14.8325485399841,15.7079632679489),
 .UNSPECIFIED.);
#2177=B_SPLINE_CURVE_WITH_KNOTS('',3,(#25414,#25415,#25416,#25417,#25418,
#25419,#25420,#25421,#25422,#25423,#25424,#25425,#25426,#25427,#25428,#25429,
#25430,#25431,#25432,#25433,#25434,#25435,#25436,#25437,#25438,#25439,#25440,
#25441,#25442,#25443,#25444,#25445,#25446,#25447,#25448,#25449,#25450,#25451,
#25452,#25453,#25454,#25455,#25456,#25457,#25458,#25459,#25460,#25461,#25462,
#25463,#25464,#25465),.UNSPECIFIED.,.F.,.F.,(4,3,3,3,3,3,3,3,3,3,3,3,3,
3,3,3,3,4),(-0.286347380332279,-0.266347789416864,-0.254098115456061,-0.230501751705225,
-0.216536610693349,-0.18668269284242,-0.173443188538191,-0.164130900566406,
-0.152678732927651,-0.129952909210668,-0.116365164485228,-0.106745630798174,
-0.0814440134366876,-0.0640046809373957,-0.0520446962100768,-0.0197039455308333,
-0.00553916135222766,0.),.UNSPECIFIED.);
#2178=B_SPLINE_CURVE_WITH_KNOTS('',3,(#25466,#25467,#25468,#25469,#25470,
#25471,#25472,#25473,#25474,#25475,#25476,#25477,#25478,#25479,#25480,#25481,
#25482,#25483,#25484,#25485,#25486,#25487,#25488,#25489,#25490,#25491,#25492,
#25493,#25494,#25495,#25496,#25497,#25498,#25499,#25500,#25501,#25502,#25503,
#25504,#25505,#25506,#25507,#25508,#25509,#25510,#25511,#25512,#25513,#25514,
#25515,#25516,#25517,#25518,#25519,#25520),.UNSPECIFIED.,.F.,.F.,(4,3,3,
3,3,3,3,3,3,3,3,3,3,3,3,3,3,3,4),(-0.2851428039951,-0.264876660632172,-0.2498967274825,
-0.236025660645345,-0.214587312757531,-0.204671023974553,-0.173775777047669,
-0.160111619860766,-0.150128525406277,-0.138317788758425,-0.118237251615849,
-0.10321155298755,-0.092840846421164,-0.0707715126256338,-0.0558839316601653,
-0.043797399607841,-0.0161434201156718,-0.00456351123904309,0.),
 .UNSPECIFIED.);
#2179=B_SPLINE_CURVE_WITH_KNOTS('',3,(#25522,#25523,#25524,#25525,#25526,
#25527,#25528,#25529,#25530,#25531,#25532),.UNSPECIFIED.,.F.,.F.,(4,1,1,
1,1,1,1,1,4),(15.7079632679489,15.8249442987858,16.8173400575874,17.809735816389,
18.8021315751907,19.7945273339923,20.7869230927939,21.7793188515956,21.9911485751284),
 .UNSPECIFIED.);
#2180=B_SPLINE_CURVE_WITH_KNOTS('',3,(#25533,#25534,#25535,#25536,#25537,
#25538,#25539,#25540,#25541,#25542),.UNSPECIFIED.,.F.,.F.,(4,1,1,1,1,1,
1,4),(15.7079632679489,16.383191644575,17.3755874033767,18.3679831621783,
19.3603789209799,20.3527746797816,21.3451704385832,21.9911485751284),
 .UNSPECIFIED.);
#2181=B_SPLINE_CURVE_WITH_KNOTS('',3,(#26019,#26020,#26021,#26022,#26023,
#26024,#26025,#26026,#26027,#26028,#26029,#26030,#26031,#26032,#26033,#26034,
#26035,#26036,#26037,#26038,#26039,#26040,#26041,#26042,#26043,#26044,#26045,
#26046,#26047,#26048,#26049,#26050,#26051,#26052,#26053,#26054,#26055,#26056,
#26057,#26058,#26059,#26060,#26061,#26062,#26063,#26064,#26065,#26066,#26067),
 .UNSPECIFIED.,.F.,.F.,(4,3,3,3,3,3,3,3,3,3,3,3,3,3,3,3,4),(0.,0.027427935344833,
0.0485975213880563,0.057338544085104,0.0868715743464506,0.0993492225585254,
0.10874754786483,0.133259321258805,0.148225404936155,0.157073224224447,
0.187711488807199,0.203788900709552,0.214227532674886,0.239511221647469,
0.25730153039039,0.279626282555456,0.285142803995123),.UNSPECIFIED.);
#2182=B_SPLINE_CURVE_WITH_KNOTS('',3,(#26068,#26069,#26070,#26071,#26072,
#26073,#26074,#26075,#26076,#26077,#26078,#26079,#26080,#26081,#26082,#26083,
#26084,#26085,#26086,#26087,#26088,#26089,#26090,#26091,#26092),
 .UNSPECIFIED.,.F.,.F.,(4,3,3,3,3,3,3,3,4),(-10.1357873115492,-9.92395758801633,
-8.9315618292147,-7.93916607041306,-6.94677031161143,-5.9543745528098,-4.96197879400816,
-3.96958303520653,-3.85260200436961),.UNSPECIFIED.);
#2183=B_SPLINE_CURVE_WITH_KNOTS('',3,(#26569,#26570,#26571,#26572,#26573,
#26574,#26575,#26576,#26577,#26578,#26579,#26580,#26581,#26582,#26583,#26584,
#26585,#26586,#26587,#26588,#26589,#26590),.UNSPECIFIED.,.F.,.F.,(4,3,3,
3,3,3,3,4),(7.59274844815659,7.93916607041306,8.9315618292147,9.92395758801632,
10.916353346818,11.9087491056196,12.9011448644212,13.8759337553361),
 .UNSPECIFIED.);
#2184=B_SPLINE_CURVE_WITH_KNOTS('',3,(#26591,#26592,#26593,#26594,#26595,
#26596,#26597,#26598,#26599,#26600,#26601,#26602,#26603,#26604,#26605,#26606,
#26607,#26608,#26609,#26610,#26611,#26612,#26613,#26614,#26615,#26616,#26617,
#26618,#26619,#26620,#26621,#26622,#26623,#26624,#26625,#26626,#26627,#26628,
#26629,#26630,#26631,#26632,#26633,#26634,#26635,#26636,#26637,#26638,#26639),
 .UNSPECIFIED.,.F.,.F.,(4,3,3,3,3,3,3,3,3,3,3,3,3,3,3,3,4),(0.,0.0320359961493654,
0.0578351282991586,0.0686833515155324,0.0999463544758613,0.113502099149543,
0.123023834848469,0.14759884188358,0.169881710030997,0.180117784856696,
0.205530503004595,0.220530951880297,0.231030371326071,0.247789211594336,
0.263619336128737,0.281768657448294,0.286347380332258),.UNSPECIFIED.);
#2185=B_SPLINE_CURVE_WITH_KNOTS('',3,(#26643,#26644,#26645,#26646,#26647,
#26648,#26649,#26650,#26651,#26652,#26653,#26654,#26655,#26656,#26657,#26658,
#26659,#26660,#26661,#26662,#26663,#26664,#26665,#26666,#26667,#26668,#26669,
#26670,#26671,#26672,#26673,#26674,#26675,#26676,#26677,#26678,#26679,#26680,
#26681,#26682,#26683,#26684,#26685,#26686,#26687,#26688,#26689,#26690,#26691,
#26692,#26693,#26694,#26695,#26696,#26697),.UNSPECIFIED.,.F.,.F.,(4,3,3,
3,3,3,3,3,3,3,3,3,3,3,3,3,3,3,4),(-0.378621596831434,-0.353562249903933,
-0.339726595154467,-0.324795073175994,-0.299958563910779,-0.289109739323556,
-0.25235894447449,-0.234461207277299,-0.219335840287605,-0.20082949567809,
-0.174834335133969,-0.155874235881852,-0.144961055903939,-0.109724944879178,
-0.089723852283725,-0.0773553386782937,-0.0372306048514265,-0.00401661180489575,
0.),.UNSPECIFIED.);
#2186=B_SPLINE_CURVE_WITH_KNOTS('',3,(#26698,#26699,#26700,#26701,#26702,
#26703,#26704,#26705,#26706,#26707,#26708,#26709,#26710,#26711,#26712,#26713,
#26714,#26715,#26716,#26717,#26718,#26719,#26720,#26721,#26722,#26723,#26724,
#26725,#26726,#26727,#26728,#26729,#26730,#26731,#26732,#26733,#26734,#26735,
#26736,#26737,#26738,#26739,#26740,#26741,#26742,#26743,#26744,#26745,#26746,
#26747,#26748,#26749,#26750,#26751,#26752),.UNSPECIFIED.,.F.,.F.,(4,3,3,
3,3,3,3,3,3,3,3,3,3,3,3,3,3,3,4),(-0.376940817211603,-0.35160224691684,
-0.332515709335319,-0.31822436103578,-0.288310916204436,-0.272711478712379,
-0.234501138719602,-0.216951876329547,-0.20548608487052,-0.180854828870935,
-0.153741722238776,-0.136717958714649,-0.126362699189128,-0.0955896266494597,
-0.0668165609022854,-0.0558907541314208,-0.0219997397314357,-0.00327040903045418,
0.),.UNSPECIFIED.);
#2187=B_SPLINE_CURVE_WITH_KNOTS('',3,(#26754,#26755,#26756,#26757,#26758,
#26759,#26760,#26761,#26762,#26763,#26764),.UNSPECIFIED.,.F.,.F.,(4,1,1,
1,1,1,1,1,4),(15.7079632679489,15.8518654961884,16.8494368691713,17.8470082421542,
18.8445796151372,19.8421509881201,20.839722361103,21.837293734086,21.9911485751285),
 .UNSPECIFIED.);
#2188=B_SPLINE_CURVE_WITH_KNOTS('',3,(#26765,#26766,#26767,#26768,#26769,
#26770,#26771,#26772,#26773,#26774),.UNSPECIFIED.,.F.,.F.,(4,1,1,1,1,1,
1,4),(15.7079632679489,16.3932837587428,17.3908551317257,18.3884265047086,
19.3859978776916,20.3835692506745,21.3811406236574,21.9911485751285),
 .UNSPECIFIED.);
#2189=B_SPLINE_CURVE_WITH_KNOTS('',3,(#27119,#27120,#27121,#27122,#27123,
#27124,#27125,#27126,#27127,#27128,#27129,#27130,#27131,#27132,#27133,#27134,
#27135,#27136,#27137,#27138,#27139,#27140,#27141,#27142,#27143,#27144,#27145,
#27146,#27147,#27148,#27149,#27150,#27151,#27152,#27153,#27154,#27155,#27156,
#27157,#27158,#27159,#27160,#27161,#27162,#27163,#27164,#27165,#27166,#27167,
#27168,#27169,#27170),.UNSPECIFIED.,.F.,.F.,(4,3,3,3,3,3,3,3,3,3,3,3,3,
3,3,3,3,4),(0.,0.0336989330766502,0.058737806914676,0.0734856897216009,
0.109795026944167,0.13287001176372,0.143641059388719,0.177205256270034,
0.195910789941764,0.207613330853891,0.24488927972035,0.269584354829063,
0.282495236861346,0.310139624218381,0.327566593080831,0.34255192583909,
0.372940760482297,0.376940817211641),.UNSPECIFIED.);
#2190=B_SPLINE_CURVE_WITH_KNOTS('',3,(#27171,#27172,#27173,#27174,#27175,
#27176,#27177,#27178,#27179,#27180,#27181,#27182,#27183,#27184,#27185,#27186,
#27187,#27188,#27189,#27190,#27191,#27192,#27193,#27194,#27195),
 .UNSPECIFIED.,.F.,.F.,(4,3,3,3,3,3,3,3,4),(-10.1295685708718,-9.97571372982933,
-8.9781423568464,-7.98057098386346,-6.98299961088053,-5.9854282378976,-4.98785686491466,
-3.99028549193173,-3.84638326369226),.UNSPECIFIED.);
#2191=B_SPLINE_CURVE_WITH_KNOTS('',3,(#27540,#27541,#27542,#27543,#27544,
#27545,#27546,#27547,#27548,#27549,#27550,#27551,#27552,#27553,#27554,#27555,
#27556,#27557,#27558,#27559,#27560,#27561),.UNSPECIFIED.,.F.,.F.,(4,3,3,
3,3,3,3,4),(7.59300756235155,7.98057098386346,8.9781423568464,9.97571372982933,
10.9732851028123,11.9708564757952,12.9684278487781,13.8761928695311),
 .UNSPECIFIED.);
#2192=B_SPLINE_CURVE_WITH_KNOTS('',3,(#27562,#27563,#27564,#27565,#27566,
#27567,#27568,#27569,#27570,#27571,#27572,#27573,#27574,#27575,#27576,#27577,
#27578,#27579,#27580,#27581,#27582,#27583,#27584,#27585,#27586,#27587,#27588,
#27589,#27590,#27591,#27592,#27593,#27594,#27595,#27596,#27597,#27598,#27599,
#27600,#27601,#27602,#27603,#27604,#27605,#27606,#27607,#27608,#27609,#27610,
#27611,#27612,#27613),.UNSPECIFIED.,.F.,.F.,(4,3,3,3,3,3,3,3,3,3,3,3,3,
3,3,3,3,4),(0.,0.0396836996751474,0.0598295377036724,0.0776045542344442,
0.089287041955902,0.127960856426141,0.1530367876033,0.165008599097631,0.197163594226426,
0.224449840232547,0.234157399588655,0.269452851616206,0.2876129966593,0.30541494242687,
0.333061769489462,0.34722178230466,0.375339207698859,0.378621596831421),
 .UNSPECIFIED.);
#2193=B_SPLINE_CURVE_WITH_KNOTS('',3,(#27648,#27649,#27650,#27651),
 .UNSPECIFIED.,.F.,.F.,(4,4),(64.1414162127729,64.8524255635527),
 .UNSPECIFIED.);
#2194=B_SPLINE_CURVE_WITH_KNOTS('',3,(#27659,#27660,#27661,#27662,#27663,
#27664,#27665,#27666,#27667,#27668),.UNSPECIFIED.,.F.,.F.,(4,3,3,4),(-62.8318530717959,
-61.8592366913888,-60.8615070673342,-60.401269768986),.UNSPECIFIED.);
#2195=B_SPLINE_CURVE_WITH_KNOTS('',3,(#27673,#27674,#27675,#27676,#27677,
#27678,#27679,#27680,#27681,#27682,#27683,#27684,#27685,#27686,#27687,#27688,
#27689,#27690,#27691,#27692,#27693,#27694,#27695,#27696,#27697),
 .UNSPECIFIED.,.F.,.F.,(4,3,3,3,3,3,3,3,4),(57.8582309055934,57.8683181951701,
58.8660478192247,59.8637774432794,60.861507067334,61.8592366913887,62.8569663154434,
63.854695939498,64.1414162127729),.UNSPECIFIED.);
#2196=B_SPLINE_CURVE_WITH_KNOTS('',3,(#27698,#27699,#27700,#27701,#27702,
#27703,#27704,#27705,#27706,#27707,#27708,#27709,#27710,#27711,#27712,#27713,
#27714,#27715,#27716,#27717,#27718,#27719),.UNSPECIFIED.,.F.,.F.,(4,3,3,
3,3,3,3,4),(-60.401269768986,-59.8637774432795,-58.8660478192248,-57.8683181951702,
-56.8705885711155,-55.8728589470609,-54.8751293230062,-54.1180844618064),
 .UNSPECIFIED.);
#2197=B_SPLINE_CURVE_WITH_KNOTS('',3,(#27724,#27725,#27726,#27727,#27728,
#27729,#27730,#27731,#27732,#27733,#27734,#27735,#27736,#27737,#27738,#27739,
#27740,#27741,#27742,#27743,#27744,#27745),.UNSPECIFIED.,.F.,.F.,(4,3,3,
3,3,3,3,4),(51.5750455984138,51.8819404508421,52.8796700748968,53.8773996989514,
54.8751293230061,55.8728589470608,56.8705885711154,57.8582309055934),
 .UNSPECIFIED.);
#2198=B_SPLINE_CURVE_WITH_KNOTS('',3,(#27746,#27747,#27748,#27749,#27750,
#27751,#27752,#27753,#27754,#27755,#27756,#27757,#27758,#27759,#27760,#27761,
#27762,#27763,#27764,#27765,#27766,#27767,#27768,#27769,#27770),
 .UNSPECIFIED.,.F.,.F.,(4,3,3,3,3,3,3,3,4),(-54.1180844618064,-53.8773996989516,
-52.8796700748969,-51.8819404508422,-50.8842108267876,-49.8864812027329,
-48.8887515786783,-47.8910219546236,-47.8348991546268),.UNSPECIFIED.);
#2199=B_SPLINE_CURVE_WITH_KNOTS('',3,(#27775,#27776,#27777,#27778,#27779,
#27780,#27781,#27782,#27783,#27784,#27785,#27786,#27787,#27788,#27789,#27790,
#27791,#27792,#27793,#27794,#27795,#27796),.UNSPECIFIED.,.F.,.F.,(4,3,3,
3,3,3,3,4),(45.2918602912342,45.8955627065142,46.8932923305688,47.8910219546235,
48.8887515786782,49.8864812027328,50.8842108267875,51.5750455984138),
 .UNSPECIFIED.);
#2200=B_SPLINE_CURVE_WITH_KNOTS('',3,(#27797,#27798,#27799,#27800,#27801,
#27802,#27803,#27804,#27805,#27806,#27807,#27808,#27809,#27810,#27811,#27812,
#27813,#27814,#27815,#27816,#27817,#27818),.UNSPECIFIED.,.F.,.F.,(4,3,3,
3,3,3,3,4),(-47.8348991546268,-46.8932923305689,-45.8955627065143,-44.8978330824596,
-43.900103458405,-42.9023738343503,-41.9046442102957,-41.5517138474472),
 .UNSPECIFIED.);
#2201=B_SPLINE_CURVE_WITH_KNOTS('',3,(#27823,#27824,#27825,#27826,#27827,
#27828,#27829,#27830,#27831,#27832,#27833,#27834,#27835,#27836,#27837,#27838,
#27839,#27840,#27841,#27842,#27843,#27844),.UNSPECIFIED.,.F.,.F.,(4,3,3,
3,3,3,3,4),(39.0086749840546,39.9091849621863,40.9069145862409,41.9046442102956,
42.9023738343502,43.9001034584049,44.8978330824595,45.2918602912342),
 .UNSPECIFIED.);
#2202=B_SPLINE_CURVE_WITH_KNOTS('',3,(#27845,#27846,#27847,#27848,#27849,
#27850,#27851,#27852,#27853,#27854,#27855,#27856,#27857,#27858,#27859,#27860,
#27861,#27862,#27863,#27864,#27865,#27866),.UNSPECIFIED.,.F.,.F.,(4,3,3,
3,3,3,3,4),(-41.5517138474472,-40.906914586241,-39.9091849621863,-38.9114553381317,
-37.913725714077,-36.9159960900224,-35.9182664659677,-35.2685285402676),
 .UNSPECIFIED.);
#2203=B_SPLINE_CURVE_WITH_KNOTS('',3,(#27871,#27872,#27873,#27874,#27875,
#27876,#27877,#27878,#27879,#27880,#27881,#27882,#27883,#27884,#27885,#27886,
#27887,#27888,#27889,#27890,#27891,#27892,#27893,#27894,#27895),
 .UNSPECIFIED.,.F.,.F.,(4,3,3,3,3,3,3,3,4),(32.725489676875,32.9250775938037,
33.9228072178583,34.920536841913,35.9182664659676,36.9159960900223,37.9137257140769,
38.9114553381316,39.0086749840546),.UNSPECIFIED.);
#2204=B_SPLINE_CURVE_WITH_KNOTS('',3,(#27896,#27897,#27898,#27899,#27900,
#27901,#27902,#27903,#27904,#27905,#27906,#27907,#27908,#27909,#27910,#27911,
#27912,#27913,#27914,#27915,#27916,#27917),.UNSPECIFIED.,.F.,.F.,(4,3,3,
3,3,3,3,4),(-35.2685285402676,-34.920536841913,-33.9228072178584,-32.9250775938037,
-31.9273479697491,-30.9296183456944,-29.9318887216397,-28.985343233088),
 .UNSPECIFIED.);
#2205=B_SPLINE_CURVE_WITH_KNOTS('',3,(#27922,#27923,#27924,#27925,#27926,
#27927,#27928,#27929,#27930,#27931,#27932,#27933,#27934,#27935,#27936,#27937,
#27938,#27939,#27940,#27941,#27942,#27943),.UNSPECIFIED.,.F.,.F.,(4,3,3,
3,3,3,3,4),(26.4423043696954,26.9386998494757,27.9364294735304,28.934159097585,
29.9318887216397,30.9296183456943,31.927347969749,32.725489676875),
 .UNSPECIFIED.);
#2206=B_SPLINE_CURVE_WITH_KNOTS('',3,(#27944,#27945,#27946,#27947,#27948,
#27949,#27950,#27951,#27952,#27953,#27954,#27955,#27956,#27957,#27958,#27959,
#27960,#27961,#27962,#27963,#27964,#27965,#27966,#27967,#27968),
 .UNSPECIFIED.,.F.,.F.,(4,3,3,3,3,3,3,3,4),(-28.985343233088,-28.9341590975851,
-27.9364294735304,-26.9386998494758,-25.9409702254211,-24.9432406013665,
-23.9455109773118,-22.9477813532571,-22.7021579259084),.UNSPECIFIED.);
#2207=B_SPLINE_CURVE_WITH_KNOTS('',3,(#27973,#27974,#27975,#27976,#27977,
#27978,#27979,#27980,#27981,#27982,#27983,#27984,#27985,#27986,#27987,#27988,
#27989,#27990,#27991,#27992,#27993,#27994),.UNSPECIFIED.,.F.,.F.,(4,3,3,
3,3,3,3,4),(20.1591190625158,20.9523221051478,21.9500517292024,22.9477813532571,
23.9455109773117,24.9432406013664,25.9409702254211,26.4423043696954),
 .UNSPECIFIED.);
#2208=B_SPLINE_CURVE_WITH_KNOTS('',3,(#27995,#27996,#27997,#27998,#27999,
#28000,#28001,#28002,#28003,#28004,#28005,#28006,#28007,#28008,#28009,#28010,
#28011,#28012,#28013,#28014,#28015,#28016),.UNSPECIFIED.,.F.,.F.,(4,3,3,
3,3,3,3,4),(-22.7021579259084,-21.9500517292025,-20.9523221051478,-19.9545924810932,
-18.9568628570385,-17.9591332329838,-16.9614036089292,-16.4189726187288),
 .UNSPECIFIED.);
#2209=B_SPLINE_CURVE_WITH_KNOTS('',3,(#28021,#28022,#28023,#28024,#28025,
#28026,#28027,#28028,#28029,#28030,#28031,#28032,#28033,#28034,#28035,#28036,
#28037,#28038,#28039,#28040,#28041,#28042,#28043,#28044,#28045),
 .UNSPECIFIED.,.F.,.F.,(4,3,3,3,3,3,3,3,4),(13.8759337553362,13.9682147367652,
14.9659443608198,15.9636739848745,16.9614036089292,17.9591332329838,18.9568628570385,
19.9545924810931,20.1591190625158),.UNSPECIFIED.);
#2210=B_SPLINE_CURVE_WITH_KNOTS('',3,(#28046,#28047,#28048,#28049,#28050,
#28051,#28052,#28053,#28054,#28055,#28056,#28057,#28058,#28059,#28060,#28061,
#28062,#28063,#28064,#28065,#28066,#28067),.UNSPECIFIED.,.F.,.F.,(4,3,3,
3,3,3,3,4),(-16.4189726187288,-15.9636739848745,-14.9659443608199,-13.9682147367652,
-12.9704851127106,-11.9727554886559,-10.9750258646012,-10.1357873115493),
 .UNSPECIFIED.);
#2211=B_SPLINE_CURVE_WITH_KNOTS('',3,(#28073,#28074,#28075,#28076,#28077,
#28078,#28079,#28080,#28081,#28082,#28083,#28084,#28085),.UNSPECIFIED.,
 .F.,.F.,(4,3,3,3,4),(-3.85260200436966,-2.99318887216398,-1.99545924810932,
-0.997729624054659,0.),.UNSPECIFIED.);
#2212=B_SPLINE_CURVE_WITH_KNOTS('',3,(#28088,#28089,#28090,#28091,#28092,
#28093,#28094,#28095,#28096,#28097,#28098,#28099,#28100,#28101,#28102,#28103,
#28104,#28105,#28106),.UNSPECIFIED.,.F.,.F.,(4,3,3,3,3,3,4),(2.02057249175679,
2.99318887216397,3.99091849621862,4.98864812027328,5.98637774432793,6.98410736838259,
7.59274844815664),.UNSPECIFIED.);
#2213=B_SPLINE_CURVE_WITH_KNOTS('',3,(#28112,#28113,#28114,#28115,#28116,
#28117,#28118,#28119),.UNSPECIFIED.,.F.,.F.,(4,1,1,1,1,4),(72.2566310325653,
72.7168683309134,73.7145979549681,74.7123275790227,75.7100572030774,76.707786827132),
 .UNSPECIFIED.);
#2214=B_SPLINE_CURVE_WITH_KNOTS('',3,(#28122,#28123,#28124,#28125,#28126,
#28127,#28128,#28129,#28130),.UNSPECIFIED.,.F.,.F.,(4,1,1,1,1,1,4),(72.2566310325653,
72.2667183221419,73.2644479461966,74.2621775702512,75.2599071943059,76.2576368183605,
77.2302531987677),.UNSPECIFIED.);
#2215=B_SPLINE_CURVE_WITH_KNOTS('',3,(#28135,#28136,#28137,#28138,#28139,
#28140,#28141,#28142,#28143,#28144),.UNSPECIFIED.,.F.,.F.,(4,1,1,1,1,1,
1,4),(65.9734457253856,66.7304905865854,67.7282202106401,68.7259498346948,
69.7236794587494,70.7214090828041,71.7191387068587,72.2566310325653),
 .UNSPECIFIED.);
#2216=B_SPLINE_CURVE_WITH_KNOTS('',3,(#28145,#28146,#28147,#28148,#28149,
#28150,#28151,#28152,#28153,#28154),.UNSPECIFIED.,.F.,.F.,(4,1,1,1,1,1,
1,4),(65.9734457253856,66.280340577814,67.2780702018686,68.2757998259233,
69.2735294499779,70.2712590740326,71.2689886980872,72.2566310325653),
 .UNSPECIFIED.);
#2217=B_SPLINE_CURVE_WITH_KNOTS('',3,(#28159,#28160,#28161,#28162,#28163,
#28164,#28165,#28166,#28167,#28168,#28169),.UNSPECIFIED.,.F.,.F.,(4,1,1,
1,1,1,1,1,4),(59.690260418206,59.7463832182028,60.7441128422575,61.7418424663121,
62.7395720903668,63.7373017144215,64.7350313384761,65.7327609625308,65.9734457253856),
 .UNSPECIFIED.);
#2218=B_SPLINE_CURVE_WITH_KNOTS('',3,(#28170,#28171,#28172,#28173,#28174,
#28175,#28176,#28177,#28178,#28179),.UNSPECIFIED.,.F.,.F.,(4,1,1,1,1,1,
1,4),(59.690260418206,60.293962833486,61.2916924575407,62.2894220815953,
63.28715170565,64.2848813297046,65.2826109537593,65.9734457253856),
 .UNSPECIFIED.);
#2219=B_SPLINE_CURVE_WITH_KNOTS('',3,(#28184,#28185,#28186,#28187,#28188,
#28189,#28190,#28191,#28192,#28193),.UNSPECIFIED.,.F.,.F.,(4,1,1,1,1,1,
1,4),(53.4070751110265,53.7600054738749,54.7577350979295,55.7554647219842,
56.7531943460389,57.7509239700935,58.7486535941482,59.690260418206),
 .UNSPECIFIED.);
#2220=B_SPLINE_CURVE_WITH_KNOTS('',3,(#28194,#28195,#28196,#28197,#28198,
#28199,#28200,#28201,#28202,#28203),.UNSPECIFIED.,.F.,.F.,(4,1,1,1,1,1,
1,4),(53.4070751110265,54.3075850891581,55.3053147132127,56.3030443372674,
57.3007739613221,58.2985035853767,59.2962332094314,59.690260418206),
 .UNSPECIFIED.);
#2221=B_SPLINE_CURVE_WITH_KNOTS('',3,(#28208,#28209,#28210,#28211,#28212,
#28213,#28214,#28215,#28216,#28217),.UNSPECIFIED.,.F.,.F.,(4,1,1,1,1,1,
1,4),(47.1238898038468,47.7736277295469,48.7713573536016,49.7690869776563,
50.7668166017109,51.7645462257656,52.7622758498202,53.4070751110265),
 .UNSPECIFIED.);
#2222=B_SPLINE_CURVE_WITH_KNOTS('',3,(#28218,#28219,#28220,#28221,#28222,
#28223,#28224,#28225,#28226,#28227,#28228),.UNSPECIFIED.,.F.,.F.,(4,1,1,
1,1,1,1,1,4),(47.1238898038468,47.3234777207755,48.3212073448301,49.3189369688848,
50.3166665929395,51.3143962169941,52.3121258410488,53.3098554651034,53.4070751110265),
 .UNSPECIFIED.);
#2223=B_SPLINE_CURVE_WITH_KNOTS('',3,(#28233,#28234,#28235,#28236,#28237,
#28238,#28239,#28240,#28241,#28242),.UNSPECIFIED.,.F.,.F.,(4,1,1,1,1,1,
1,4),(40.8407044966673,41.787249985219,42.7849796092736,43.7827092333283,
44.780438857383,45.7781684814376,46.7758981054923,47.1238898038468),
 .UNSPECIFIED.);
#2224=B_SPLINE_CURVE_WITH_KNOTS('',3,(#28243,#28244,#28245,#28246,#28247,
#28248,#28249,#28250,#28251,#28252),.UNSPECIFIED.,.F.,.F.,(4,1,1,1,1,1,
1,4),(40.8407044966673,41.3370999764475,42.3348296005022,43.3325592245569,
44.3302888486115,45.3280184726662,46.3257480967208,47.1238898038468),
 .UNSPECIFIED.);
#2225=B_SPLINE_CURVE_WITH_KNOTS('',3,(#28257,#28258,#28259,#28260,#28261,
#28262,#28263,#28264,#28265,#28266,#28267),.UNSPECIFIED.,.F.,.F.,(4,1,1,
1,1,1,1,1,4),(34.5575191894877,34.8031426168364,35.800872240891,36.7986018649457,
37.7963314890004,38.794061113055,39.7917907371097,40.7895203611643,40.8407044966673),
 .UNSPECIFIED.);
#2226=B_SPLINE_CURVE_WITH_KNOTS('',3,(#28268,#28269,#28270,#28271,#28272,
#28273,#28274,#28275,#28276,#28277),.UNSPECIFIED.,.F.,.F.,(4,1,1,1,1,1,
1,4),(34.5575191894877,35.3507222321196,36.3484518561743,37.3461814802289,
38.3439111042836,39.3416407283382,40.3393703523929,40.8407044966673),
 .UNSPECIFIED.);
#2227=B_SPLINE_CURVE_WITH_KNOTS('',3,(#28282,#28283,#28284,#28285,#28286,
#28287,#28288,#28289,#28290,#28291),.UNSPECIFIED.,.F.,.F.,(4,1,1,1,1,1,
1,4),(28.2743338823081,28.8167648725084,29.8144944965631,30.8122241206177,
31.8099537446724,32.8076833687271,33.8054129927817,34.5575191894877),
 .UNSPECIFIED.);
#2228=B_SPLINE_CURVE_WITH_KNOTS('',3,(#28292,#28293,#28294,#28295,#28296,
#28297,#28298,#28299,#28300,#28301,#28302),.UNSPECIFIED.,.F.,.F.,(4,1,1,
1,1,1,1,1,4),(28.2743338823081,28.366614863737,29.3643444877917,30.3620741118463,
31.359803735901,32.3575333599556,33.3552629840103,34.352992608065,34.5575191894877),
 .UNSPECIFIED.);
#2229=B_SPLINE_CURVE_WITH_KNOTS('',3,(#28307,#28308,#28309,#28310,#28311,
#28312,#28313,#28314,#28315,#28316),.UNSPECIFIED.,.F.,.F.,(4,1,1,1,1,1,
1,4),(21.9911485751285,22.8303871281805,23.8281167522351,24.8258463762898,
25.8235760003445,26.8213056243991,27.8190352484538,28.2743338823081),
 .UNSPECIFIED.);
#2230=B_SPLINE_CURVE_WITH_KNOTS('',3,(#28317,#28318,#28319,#28320,#28321,
#28322,#28323,#28324,#28325,#28326),.UNSPECIFIED.,.F.,.F.,(4,1,1,1,1,1,
1,4),(21.9911485751285,22.3802371194091,23.3779667434637,24.3756963675184,
25.3734259915731,26.3711556156277,27.3688852396824,28.2743338823081),
 .UNSPECIFIED.);
#2231=B_SPLINE_CURVE_WITH_KNOTS('',3,(#28332,#28333,#28334,#28335,#28336),
 .UNSPECIFIED.,.F.,.F.,(4,1,4),(14.3984001269718,15.3961297510265,15.7079632679489),
 .UNSPECIFIED.);
#2232=B_SPLINE_CURVE_WITH_KNOTS('',3,(#28339,#28340,#28341,#28342,#28343),
 .UNSPECIFIED.,.F.,.F.,(4,1,4),(13.8759337553361,14.8485501357432,15.7079632679489),
 .UNSPECIFIED.);
#2233=B_SPLINE_CURVE_WITH_KNOTS('',3,(#28345,#28346,#28347,#28348,#28349,
#28350,#28351,#28352,#28353,#28354,#28355,#28356,#28357,#28358,#28359,#28360,
#28361,#28362,#28363,#28364,#28365,#28366,#28367,#28368,#28369,#28370,#28371,
#28372,#28373,#28374,#28375,#28376,#28377,#28378,#28379,#28380,#28381,#28382,
#28383,#28384,#28385,#28386,#28387,#28388,#28389,#28390,#28391,#28392,#28393,
#28394,#28395,#28396),.UNSPECIFIED.,.F.,.F.,(4,3,3,3,3,3,3,3,3,3,3,3,3,
3,3,3,3,4),(-0.286347380332243,-0.266225517657927,-0.253989633145399,-0.224118418951897,
-0.213637228539926,-0.18277997814213,-0.1712802294816,-0.161583702204544,
-0.151922727744335,-0.129977880386141,-0.117970426661857,-0.109303558462843,
-0.0829498108000933,-0.0663205445941391,-0.0521986510922473,-0.0198616494821571,
-0.00388856781184301,0.),.UNSPECIFIED.);
#2234=B_SPLINE_CURVE_WITH_KNOTS('',3,(#28397,#28398,#28399,#28400,#28401,
#28402,#28403,#28404,#28405,#28406,#28407,#28408,#28409,#28410,#28411,#28412,
#28413,#28414,#28415,#28416,#28417,#28418,#28419,#28420,#28421,#28422,#28423,
#28424,#28425,#28426,#28427,#28428,#28429,#28430,#28431,#28432,#28433,#28434,
#28435,#28436,#28437,#28438,#28439,#28440,#28441,#28442,#28443,#28444,#28445,
#28446,#28447,#28448,#28449,#28450,#28451),.UNSPECIFIED.,.F.,.F.,(4,3,3,
3,3,3,3,3,3,3,3,3,3,3,3,3,3,3,4),(-0.285142803995136,-0.264771978453909,
-0.248971203111392,-0.236527824899921,-0.214293390992849,-0.2038268270722,
-0.17295400685889,-0.159192875564253,-0.149652609754856,-0.137562774558619,
-0.11631964633286,-0.104925727456541,-0.0956925453293139,-0.0725695145406395,
-0.0586514835868502,-0.0490375298028169,-0.0212486353032901,-0.00320042217461625,
0.),.UNSPECIFIED.);
#2235=B_SPLINE_CURVE_WITH_KNOTS('',3,(#28453,#28454,#28455,#28456,#28457,
#28458,#28459,#28460,#28461,#28462,#28463),.UNSPECIFIED.,.F.,.F.,(4,1,1,
1,1,1,1,1,4),(15.7079632679489,15.8462797597979,16.8440093838525,17.8417390079072,
18.8394686319618,19.8371982560165,20.8349278800712,21.8326575041258,21.9911485751285),
 .UNSPECIFIED.);
#2236=B_SPLINE_CURVE_WITH_KNOTS('',3,(#28464,#28465,#28466,#28467,#28468,
#28469,#28470,#28471,#28472,#28473),.UNSPECIFIED.,.F.,.F.,(4,1,1,1,1,1,
1,4),(15.7079632679489,16.3938593750811,17.3915889991358,18.3893186231905,
19.3870482472451,20.3847778712998,21.3825074953544,21.9911485751285),
 .UNSPECIFIED.);
#2237=B_SPLINE_CURVE_WITH_KNOTS('',3,(#28746,#28747,#28748,#28749,#28750,
#28751,#28752,#28753,#28754,#28755,#28756,#28757,#28758,#28759,#28760,#28761,
#28762,#28763,#28764,#28765,#28766,#28767,#28768,#28769,#28770,#28771,#28772,
#28773,#28774,#28775,#28776,#28777,#28778,#28779,#28780,#28781,#28782,#28783,
#28784,#28785,#28786,#28787,#28788,#28789,#28790,#28791,#28792,#28793,#28794),
 .UNSPECIFIED.,.F.,.F.,(4,3,3,3,3,3,3,3,3,3,3,3,3,3,3,3,4),(0.,0.0274255371814078,
0.0484189866654049,0.0576777559231281,0.0872193790463039,0.100313119697051,
0.108749799500732,0.134012411342703,0.149997937188314,0.163168454336766,
0.192693763100972,0.210037636696566,0.220559059471184,0.247872294074534,
0.26049857837061,0.281269689393589,0.285142803995142),.UNSPECIFIED.);
#2238=B_SPLINE_CURVE_WITH_KNOTS('',3,(#28795,#28796,#28797,#28798,#28799,
#28800,#28801,#28802,#28803,#28804,#28805,#28806,#28807,#28808,#28809,#28810,
#28811,#28812,#28813,#28814,#28815,#28816,#28817,#28818,#28819),
 .UNSPECIFIED.,.F.,.F.,(4,3,3,3,3,3,3,3,4),(-10.1357873115493,-9.97729624054658,
-8.97956661649192,-7.98183699243727,-6.98410736838261,-5.98637774432795,
-4.98864812027329,-3.99091849621863,-3.85260200436966),.UNSPECIFIED.);
#2239=B_SPLINE_CURVE_WITH_KNOTS('',3,(#29092,#29093,#29094,#29095,#29096,
#29097,#29098,#29099,#29100,#29101,#29102,#29103,#29104,#29105,#29106,#29107,
#29108,#29109,#29110,#29111,#29112,#29113),.UNSPECIFIED.,.F.,.F.,(4,3,3,
3,3,3,3,4),(7.59274844815664,7.98183699243725,8.9795666164919,9.97729624054656,
10.9750258646012,11.9727554886559,12.9704851127105,13.8759337553362),
 .UNSPECIFIED.);
#2240=B_SPLINE_CURVE_WITH_KNOTS('',3,(#29114,#29115,#29116,#29117,#29118,
#29119,#29120,#29121,#29122,#29123,#29124,#29125,#29126,#29127,#29128,#29129,
#29130,#29131,#29132,#29133,#29134,#29135,#29136,#29137,#29138,#29139,#29140,
#29141,#29142,#29143,#29144,#29145,#29146,#29147,#29148,#29149,#29150,#29151,
#29152,#29153,#29154,#29155,#29156,#29157,#29158,#29159,#29160,#29161,#29162),
 .UNSPECIFIED.,.F.,.F.,(4,3,3,3,3,3,3,3,3,3,3,3,3,3,3,3,4),(0.,0.0320358644790656,
0.0566025392350713,0.0661929095230273,0.097524509655756,0.113218578765797,
0.122777613428698,0.148357330195644,0.170686258066526,0.180239221440332,
0.205963417559621,0.220473935588774,0.231002296372473,0.247562418687567,
0.263621625608468,0.283136005917488,0.286347380332233),.UNSPECIFIED.);
#2241=B_SPLINE_CURVE_WITH_KNOTS('',3,(#29608,#29609,#29610,#29611,#29612,
#29613,#29614,#29615,#29616,#29617,#29618,#29619,#29620,#29621,#29622,#29623,
#29624,#29625,#29626,#29627,#29628,#29629,#29630,#29631,#29632,#29633,#29634,
#29635,#29636),.UNSPECIFIED.,.F.,.F.,(4,1,1,1,1,1,1,1,1,1,1,1,1,1,1,1,1,
1,1,1,1,1,1,1,1,1,4),(0.,0.483321946706122,0.966643893412244,1.44996584011837,
1.93328778682449,2.41660973353061,2.89993168023673,3.38325362694285,3.86657557364898,
4.3498975203551,4.83321946706122,5.31654141376734,5.79986336047346,6.28318530717959,
6.76650725388571,7.24982920059183,7.73315114729795,8.21647309400407,8.6997950407102,
9.18311698741632,9.66643893412244,10.1497608808286,10.6330828275347,11.1164047742408,
11.5997267209469,12.083048667653,12.5663706143592),.UNSPECIFIED.);
#2242=B_SPLINE_CURVE_WITH_KNOTS('',3,(#29661,#29662,#29663,#29664,#29665,
#29666,#29667,#29668,#29669,#29670),.UNSPECIFIED.,.F.,.F.,(4,3,3,4),(-4.09254174883833,
-3.98934337020898,-2.99200752765673,-2.06514013327813),.UNSPECIFIED.);
#2243=B_SPLINE_CURVE_WITH_KNOTS('',3,(#29673,#29674,#29675,#29676,#29677,
#29678,#29679),.UNSPECIFIED.,.F.,.F.,(4,3,4),(0.,0.998006970630082,1.11419103802948),
 .UNSPECIFIED.);
#2244=B_SPLINE_CURVE_WITH_KNOTS('',3,(#29684,#29685,#29686,#29687,#29688,
#29689,#29690,#29691,#29692,#29693,#29694,#29695,#29696,#29697,#29698,#29699,
#29700,#29701,#29702,#29703,#29704,#29705),.UNSPECIFIED.,.F.,.F.,(4,3,3,
3,3,3,3,4),(-10.3757270560179,-9.97335842552244,-8.9760225829702,-7.97868674041795,
-6.9813508978657,-5.98401505531347,-4.98667921276122,-4.09254174883833),
 .UNSPECIFIED.);
#2245=B_SPLINE_CURVE_WITH_KNOTS('',3,(#29706,#29707,#29708,#29709,#29710,
#29711,#29712,#29713,#29714,#29715,#29716,#29717,#29718,#29719,#29720,#29721,
#29722,#29723,#29724,#29725,#29726,#29727),.UNSPECIFIED.,.F.,.F.,(4,3,3,
3,3,3,3,4),(1.11419103802948,1.99601394126018,2.99402091189026,3.99202788252035,
4.99003485315045,5.98804182378054,6.98604879441062,7.39737634520907),
 .UNSPECIFIED.);
#2246=B_SPLINE_CURVE_WITH_KNOTS('',3,(#29732,#29733,#29734,#29735,#29736,
#29737,#29738,#29739,#29740,#29741,#29742,#29743,#29744,#29745,#29746,#29747,
#29748,#29749,#29750,#29751,#29752,#29753),.UNSPECIFIED.,.F.,.F.,(4,3,3,
3,3,3,3,4),(-16.6589123631975,-15.9573734808359,-14.9600376382837,-13.9627017957314,
-12.9653659531792,-11.9680301106269,-10.9706942680747,-10.3757270560179),
 .UNSPECIFIED.);
#2247=B_SPLINE_CURVE_WITH_KNOTS('',3,(#29754,#29755,#29756,#29757,#29758,
#29759,#29760,#29761,#29762,#29763,#29764,#29765,#29766,#29767,#29768,#29769,
#29770,#29771,#29772,#29773,#29774,#29775),.UNSPECIFIED.,.F.,.F.,(4,3,3,
3,3,3,3,4),(7.39737634520907,7.98405576504071,8.9820627356708,9.98006970630089,
10.978076676931,11.9760836475611,12.9740906181912,13.6805616523887),
 .UNSPECIFIED.);
#2248=B_SPLINE_CURVE_WITH_KNOTS('',3,(#29780,#29781,#29782,#29783,#29784,
#29785,#29786,#29787,#29788,#29789,#29790,#29791,#29792,#29793,#29794,#29795,
#29796,#29797,#29798,#29799,#29800,#29801),.UNSPECIFIED.,.F.,.F.,(4,3,3,
3,3,3,3,4),(-22.9420976703771,-21.9413885361494,-20.9440526935971,-19.9467168510449,
-18.9493810084926,-17.9520451659404,-16.9547093233881,-16.6589123631975),
 .UNSPECIFIED.);
#2249=B_SPLINE_CURVE_WITH_KNOTS('',3,(#29802,#29803,#29804,#29805,#29806,
#29807,#29808,#29809,#29810,#29811,#29812,#29813,#29814,#29815,#29816,#29817,
#29818,#29819,#29820,#29821,#29822,#29823),.UNSPECIFIED.,.F.,.F.,(4,3,3,
3,3,3,3,4),(13.6805616523887,13.9720975888212,14.9701045594513,15.9681115300814,
16.9661185007115,17.9641254713416,18.9621324419717,19.9637469595682),
 .UNSPECIFIED.);
#2250=B_SPLINE_CURVE_WITH_KNOTS('',3,(#29828,#29829,#29830,#29831,#29832,
#29833,#29834,#29835,#29836,#29837,#29838,#29839,#29840,#29841,#29842,#29843,
#29844,#29845,#29846,#29847,#29848,#29849),.UNSPECIFIED.,.F.,.F.,(4,3,3,
3,3,3,3,4),(-29.2252829775567,-28.9227394340151,-27.9254035914628,-26.9280677489106,
-25.9307319063583,-24.9333960638061,-23.9360602212539,-22.9420976703771),
 .UNSPECIFIED.);
#2251=B_SPLINE_CURVE_WITH_KNOTS('',3,(#29850,#29851,#29852,#29853,#29854,
#29855,#29856,#29857,#29858,#29859,#29860,#29861,#29862,#29863,#29864,#29865,
#29866,#29867,#29868,#29869,#29870,#29871),.UNSPECIFIED.,.F.,.F.,(4,3,3,
3,3,3,3,4),(19.9637469595682,20.9581463832319,21.956153353862,22.954160324492,
23.9521672951221,24.9501742657522,25.9481812363823,26.2469322667478),
 .UNSPECIFIED.);
#2252=B_SPLINE_CURVE_WITH_KNOTS('',3,(#29876,#29877,#29878,#29879,#29880,
#29881,#29882,#29883,#29884,#29885,#29886,#29887,#29888,#29889,#29890,#29891,
#29892,#29893,#29894,#29895,#29896,#29897),.UNSPECIFIED.,.F.,.F.,(4,3,3,
3,3,3,3,4),(-35.5084682847363,-34.9067544893285,-33.9094186467763,-32.9120828042241,
-31.9147469616718,-30.9174111191196,-29.9200752765673,-29.2252829775567),
 .UNSPECIFIED.);
#2253=B_SPLINE_CURVE_WITH_KNOTS('',3,(#29898,#29899,#29900,#29901,#29902,
#29903,#29904,#29905,#29906,#29907,#29908,#29909,#29910,#29911,#29912,#29913,
#29914,#29915,#29916,#29917,#29918,#29919),.UNSPECIFIED.,.F.,.F.,(4,3,3,
3,3,3,3,4),(26.2469322667478,26.9461882070124,27.9441951776425,28.9422021482726,
29.9402091189027,30.9382160895327,31.9362230601628,32.5301175739274),
 .UNSPECIFIED.);
#2254=B_SPLINE_CURVE_WITH_KNOTS('',3,(#29924,#29925,#29926,#29927,#29928,
#29929,#29930,#29931,#29932,#29933,#29934,#29935,#29936,#29937,#29938,#29939,
#29940,#29941,#29942,#29943,#29944,#29945),.UNSPECIFIED.,.F.,.F.,(4,3,3,
3,3,3,3,4),(-41.7916535919159,-40.890769544642,-39.8934337020898,-38.8960978595375,
-37.8987620169853,-36.901426174433,-35.9040903318808,-35.5084682847363),
 .UNSPECIFIED.);
#2255=B_SPLINE_CURVE_WITH_KNOTS('',3,(#29946,#29947,#29948,#29949,#29950,
#29951,#29952,#29953,#29954,#29955,#29956,#29957,#29958,#29959,#29960,#29961,
#29962,#29963,#29964,#29965,#29966,#29967),.UNSPECIFIED.,.F.,.F.,(4,3,3,
3,3,3,3,4),(32.5301175739274,32.9342300307929,33.932237001423,34.9302439720531,
35.9282509426832,36.9262579133133,37.9242648839434,38.813302881107),
 .UNSPECIFIED.);
#2256=B_SPLINE_CURVE_WITH_KNOTS('',3,(#29972,#29973,#29974,#29975,#29976,
#29977,#29978,#29979,#29980,#29981,#29982,#29983,#29984,#29985,#29986,#29987,
#29988,#29989,#29990,#29991,#29992,#29993,#29994,#29995,#29996),
 .UNSPECIFIED.,.F.,.F.,(4,3,3,3,3,3,3,3,4),(-48.0748388990955,-47.8721204425077,
-46.8747845999555,-45.8774487574032,-44.880112914851,-43.8827770722987,
-42.8854412297465,-41.8881053871943,-41.7916535919159),.UNSPECIFIED.);
#2257=B_SPLINE_CURVE_WITH_KNOTS('',3,(#29997,#29998,#29999,#30000,#30001,
#30002,#30003,#30004,#30005,#30006,#30007,#30008,#30009,#30010,#30011,#30012,
#30013,#30014,#30015,#30016,#30017,#30018,#30019,#30020,#30021),
 .UNSPECIFIED.,.F.,.F.,(4,3,3,3,3,3,3,3,4),(38.813302881107,38.9222718545735,
39.9202788252036,40.9182857958337,41.9162927664637,42.9142997370938,43.9123067077239,
44.910313678354,45.0964881882866),.UNSPECIFIED.);
#2258=B_SPLINE_CURVE_WITH_KNOTS('',3,(#30026,#30027,#30028,#30029,#30030,
#30031,#30032,#30033,#30034,#30035,#30036,#30037,#30038,#30039,#30040,#30041,
#30042,#30043,#30044,#30045,#30046,#30047),.UNSPECIFIED.,.F.,.F.,(4,3,3,
3,3,3,3,4),(-54.3580242062751,-53.8561354978212,-52.8587996552689,-51.8614638127167,
-50.8641279701645,-49.8667921276122,-48.86945628506,-48.0748388990955),
 .UNSPECIFIED.);
#2259=B_SPLINE_CURVE_WITH_KNOTS('',3,(#30048,#30049,#30050,#30051,#30052,
#30053,#30054,#30055,#30056,#30057,#30058,#30059,#30060,#30061,#30062,#30063,
#30064,#30065,#30066,#30067,#30068,#30069),.UNSPECIFIED.,.F.,.F.,(4,3,3,
3,3,3,3,4),(45.0964881882866,45.9083206489841,46.9063276196142,47.9043345902443,
48.9023415608744,49.9003485315045,50.8983555021345,51.3796734954662),
 .UNSPECIFIED.);
#2260=B_SPLINE_CURVE_WITH_KNOTS('',3,(#30074,#30075,#30076,#30077,#30078,
#30079,#30080,#30081,#30082,#30083,#30084,#30085,#30086,#30087,#30088,#30089,
#30090,#30091,#30092,#30093,#30094,#30095),.UNSPECIFIED.,.F.,.F.,(4,3,3,
3,3,3,3,4),(-60.6412095134546,-59.8401505531347,-58.8428147105824,-57.8454788680302,
-56.8481430254779,-55.8508071829257,-54.8534713403734,-54.3580242062751),
 .UNSPECIFIED.);
#2261=B_SPLINE_CURVE_WITH_KNOTS('',3,(#30096,#30097,#30098,#30099,#30100,
#30101,#30102,#30103,#30104,#30105,#30106,#30107,#30108,#30109,#30110,#30111,
#30112,#30113,#30114,#30115,#30116,#30117),.UNSPECIFIED.,.F.,.F.,(4,3,3,
3,3,3,3,4),(51.3796734954662,51.8963624727646,52.8943694433947,53.8923764140248,
54.8903833846549,55.888390355285,56.8863973259151,57.6628588026458),
 .UNSPECIFIED.);
#2262=B_SPLINE_CURVE_WITH_KNOTS('',3,(#30122,#30123,#30124,#30125,#30126,
#30127,#30128,#30129,#30130,#30131,#30132,#30133,#30134,#30135,#30136,#30137,
#30138,#30139,#30140,#30141,#30142,#30143,#30144,#30145,#30146),
 .UNSPECIFIED.,.F.,.F.,(4,3,3,3,3,3,3,3,4),(-66.9243948206342,-66.8215014510004,
-65.8241656084481,-64.8268297658959,-63.8294939233436,-62.8321580807914,
-61.8348222382391,-60.8374863956869,-60.6412095134546),.UNSPECIFIED.);
#2263=B_SPLINE_CURVE_WITH_KNOTS('',3,(#30147,#30148,#30149,#30150,#30151,
#30152,#30153,#30154,#30155,#30156,#30157,#30158,#30159,#30160,#30161,#30162,
#30163,#30164,#30165,#30166,#30167,#30168,#30169,#30170,#30171),
 .UNSPECIFIED.,.F.,.F.,(4,3,3,3,3,3,3,3,4),(57.6628588026458,57.8844042965452,
58.8824112671752,59.8804182378054,60.8784252084354,61.8764321790655,62.8744391496956,
63.8724461203257,63.9460441098254),.UNSPECIFIED.);
#2264=B_SPLINE_CURVE_WITH_KNOTS('',3,(#30176,#30177,#30178,#30179,#30180,
#30181,#30182,#30183,#30184,#30185,#30186,#30187,#30188,#30189,#30190,#30191,
#30192,#30193,#30194,#30195,#30196,#30197),.UNSPECIFIED.,.F.,.F.,(4,3,3,
3,3,3,3,4),(-73.2075801278138,-72.8055165063138,-71.8081806637616,-70.8108448212093,
-69.8135089786571,-68.8161731361048,-67.8188372935526,-66.9243948206342),
 .UNSPECIFIED.);
#2265=B_SPLINE_CURVE_WITH_KNOTS('',3,(#30198,#30199,#30200,#30201,#30202,
#30203,#30204,#30205,#30206,#30207,#30208,#30209,#30210,#30211,#30212,#30213,
#30214,#30215,#30216,#30217,#30218,#30219),.UNSPECIFIED.,.F.,.F.,(4,3,3,
3,3,3,3,4),(63.9460441098254,64.8704530909558,65.8684600615859,66.866467032216,
67.8644740028461,68.8624809734761,69.8604879441062,70.229229417005),
 .UNSPECIFIED.);
#2266=B_SPLINE_CURVE_WITH_KNOTS('',3,(#30224,#30225,#30226,#30227,#30228,
#30229,#30230,#30231,#30232,#30233,#30234,#30235,#30236,#30237,#30238,#30239,
#30240,#30241,#30242,#30243,#30244,#30245),.UNSPECIFIED.,.F.,.F.,(4,3,3,
3,3,3,3,4),(-79.4907654349934,-78.7895315616273,-77.792195719075,-76.7948598765228,
-75.7975240339705,-74.8001881914183,-73.802852348866,-73.2075801278138),
 .UNSPECIFIED.);
#2267=B_SPLINE_CURVE_WITH_KNOTS('',3,(#30246,#30247,#30248,#30249,#30250,
#30251,#30252,#30253,#30254,#30255,#30256,#30257,#30258,#30259,#30260,#30261,
#30262,#30263,#30264,#30265,#30266,#30267),.UNSPECIFIED.,.F.,.F.,(4,3,3,
3,3,3,3,4),(70.229229417005,70.8584949147363,71.8565018853664,72.8545088559965,
73.8525158266266,74.8505227972567,75.8485297678868,76.5124147241846),
 .UNSPECIFIED.);
#2268=B_SPLINE_CURVE_WITH_KNOTS('',3,(#30272,#30273,#30274,#30275,#30276,
#30277,#30278,#30279,#30280,#30281,#30282,#30283,#30284,#30285,#30286,#30287,
#30288,#30289,#30290,#30291,#30292,#30293),.UNSPECIFIED.,.F.,.F.,(4,3,3,
3,3,3,3,4),(-85.773950742173,-84.7735466169407,-83.7762107743885,-82.7788749318363,
-81.781539089284,-80.7842032467318,-79.7868674041795,-79.4907654349934),
 .UNSPECIFIED.);
#2269=B_SPLINE_CURVE_WITH_KNOTS('',3,(#30294,#30295,#30296,#30297,#30298,
#30299,#30300,#30301,#30302,#30303,#30304,#30305,#30306,#30307,#30308,#30309,
#30310,#30311,#30312,#30313,#30314,#30315),.UNSPECIFIED.,.F.,.F.,(4,3,3,
3,3,3,3,4),(76.5124147241846,76.8465367385169,77.8445437091469,78.842550679777,
79.8405576504071,80.8385646210372,81.8365715916673,82.7956000313642),
 .UNSPECIFIED.);
#2270=B_SPLINE_CURVE_WITH_KNOTS('',3,(#30320,#30321,#30322,#30323,#30324,
#30325,#30326,#30327,#30328,#30329,#30330,#30331,#30332,#30333,#30334,#30335,
#30336,#30337,#30338,#30339,#30340,#30341),.UNSPECIFIED.,.F.,.F.,(4,3,3,
3,3,3,3,4),(-92.0571360493526,-91.7548975148065,-90.7575616722542,-89.760225829702,
-88.7628899871497,-87.7655541445975,-86.7682183020452,-85.773950742173),
 .UNSPECIFIED.);
#2271=B_SPLINE_CURVE_WITH_KNOTS('',3,(#30342,#30343,#30344,#30345,#30346,
#30347,#30348,#30349,#30350,#30351,#30352,#30353,#30354,#30355,#30356,#30357,
#30358,#30359,#30360,#30361,#30362,#30363,#30364,#30365,#30366),
 .UNSPECIFIED.,.F.,.F.,(4,3,3,3,3,3,3,3,4),(82.7956000313642,82.8345785622974,
83.8325855329275,84.8305925035576,85.8285994741877,86.8266064448178,87.8246134154479,
88.822620386078,89.0787853385438),.UNSPECIFIED.);
#2272=B_SPLINE_CURVE_WITH_KNOTS('',3,(#30371,#30372,#30373,#30374,#30375,
#30376,#30377,#30378,#30379,#30380,#30381,#30382,#30383,#30384,#30385,#30386,
#30387,#30388,#30389,#30390,#30391,#30392),.UNSPECIFIED.,.F.,.F.,(4,3,3,
3,3,3,3,4),(-98.3403213565322,-97.7389125701199,-96.7415767275677,-95.7442408850154,
-94.7469050424632,-93.7495691999109,-92.7522333573587,-92.0571360493526),
 .UNSPECIFIED.);
#2273=B_SPLINE_CURVE_WITH_KNOTS('',3,(#30393,#30394,#30395,#30396,#30397,
#30398,#30399,#30400,#30401,#30402,#30403,#30404,#30405,#30406,#30407,#30408,
#30409,#30410,#30411,#30412,#30413,#30414),.UNSPECIFIED.,.F.,.F.,(4,3,3,
3,3,3,3,4),(89.0787853385438,89.820627356708,90.8186343273381,91.8166412979682,
92.8146482685983,93.8126552392284,94.8106622098585,95.3619706457233),
 .UNSPECIFIED.);
#2274=B_SPLINE_CURVE_WITH_KNOTS('',3,(#30420,#30421,#30422,#30423,#30424,
#30425,#30426,#30427),.UNSPECIFIED.,.F.,.F.,(4,1,1,1,1,4),(109.955742875643,
110.351669931783,111.349005774335,112.346341616887,113.343677459439,114.341013301992),
 .UNSPECIFIED.);
#2275=B_SPLINE_CURVE_WITH_KNOTS('',3,(#30430,#30431,#30432,#30433,#30434,
#30435,#30436),.UNSPECIFIED.,.F.,.F.,(4,1,1,1,4),(109.955742875643,110.107297927009,
111.105304897639,112.103311868269,113.101318838899),.UNSPECIFIED.);
#2276=B_SPLINE_CURVE_WITH_KNOTS('',3,(#30441,#30442,#30443,#30444,#30445,
#30446,#30447,#30448,#30449,#30450),.UNSPECIFIED.,.F.,.F.,(4,1,1,1,1,1,
1,4),(103.672557568463,104.367654876469,105.364990719021,106.362326561574,
107.359662404126,108.356998246678,109.35433408923,109.955742875643),
 .UNSPECIFIED.);
#2277=B_SPLINE_CURVE_WITH_KNOTS('',3,(#30451,#30452,#30453,#30454,#30455,
#30456,#30457,#30458,#30459,#30460),.UNSPECIFIED.,.F.,.F.,(4,1,1,1,1,1,
1,4),(103.672557568463,104.119256103228,105.117263073858,106.115270044488,
107.113277015118,108.111283985749,109.109290956379,109.955742875643),
 .UNSPECIFIED.);
#2278=B_SPLINE_CURVE_WITH_KNOTS('',3,(#30465,#30466,#30467,#30468,#30469,
#30470,#30471,#30472,#30473,#30474),.UNSPECIFIED.,.F.,.F.,(4,1,1,1,1,1,
1,4),(97.3893722612836,98.3836398211558,99.380975663708,100.37831150626,
101.375647348812,102.372983191365,103.370319033917,103.672557568463),
 .UNSPECIFIED.);
#2279=B_SPLINE_CURVE_WITH_KNOTS('',3,(#30475,#30476,#30477,#30478,#30479,
#30480,#30481,#30482,#30483,#30484),.UNSPECIFIED.,.F.,.F.,(4,1,1,1,1,1,
1,4),(97.3893722612836,98.1312142794477,99.1292212500778,100.127228220708,
101.125235191338,102.123242161968,103.121249132598,103.672557568463),
 .UNSPECIFIED.);
#2280=B_SPLINE_CURVE_WITH_KNOTS('',3,(#30489,#30490,#30491,#30492,#30493,
#30494,#30495,#30496,#30497,#30498,#30499),.UNSPECIFIED.,.F.,.F.,(4,1,1,
1,1,1,1,1,4),(91.106186954104,91.4022889232901,92.3996247658423,93.3969606083945,
94.3942964509468,95.391632293499,96.3889681360513,97.3863039786035,97.3893722612836),
 .UNSPECIFIED.);
#2281=B_SPLINE_CURVE_WITH_KNOTS('',3,(#30500,#30501,#30502,#30503,#30504,
#30505,#30506,#30507,#30508,#30509,#30510),.UNSPECIFIED.,.F.,.F.,(4,1,1,
1,1,1,1,1,4),(91.106186954104,91.1451654850371,92.1431724556672,93.1411794262973,
94.1391863969273,95.1371933675574,96.1352003381875,97.1332073088176,97.3893722612836),
 .UNSPECIFIED.);
#2282=B_SPLINE_CURVE_WITH_KNOTS('',3,(#30515,#30516,#30517,#30518,#30519,
#30520,#30521,#30522,#30523,#30524),.UNSPECIFIED.,.F.,.F.,(4,1,1,1,1,1,
1,4),(84.8230016469244,85.4182738679766,86.4156097105288,87.4129455530811,
88.4102813956333,89.4076172381856,90.4049530807378,91.106186954104),
 .UNSPECIFIED.);
#2283=B_SPLINE_CURVE_WITH_KNOTS('',3,(#30525,#30526,#30527,#30528,#30529,
#30530,#30531,#30532,#30533,#30534),.UNSPECIFIED.,.F.,.F.,(4,1,1,1,1,1,
1,4),(84.8230016469244,85.1571236612565,86.1551306318866,87.1531376025167,
88.1511445731468,89.1491515437769,90.147158514407,91.106186954104),
 .UNSPECIFIED.);
#2284=B_SPLINE_CURVE_WITH_KNOTS('',3,(#30539,#30540,#30541,#30542,#30543,
#30544,#30545,#30546,#30547,#30548),.UNSPECIFIED.,.F.,.F.,(4,1,1,1,1,1,
1,4),(78.5398163397448,79.4342588126631,80.4315946552154,81.4289304977676,
82.4262663403199,83.4236021828721,84.4209380254243,84.8230016469244),
 .UNSPECIFIED.);
#2285=B_SPLINE_CURVE_WITH_KNOTS('',3,(#30549,#30550,#30551,#30552,#30553,
#30554,#30555,#30556,#30557,#30558),.UNSPECIFIED.,.F.,.F.,(4,1,1,1,1,1,
1,4),(78.5398163397448,79.169081837476,80.1670888081061,81.1650957787362,
82.1631027493663,83.1611097199964,84.1591166906264,84.8230016469244),
 .UNSPECIFIED.);
#2286=B_SPLINE_CURVE_WITH_KNOTS('',3,(#30563,#30564,#30565,#30566,#30567,
#30568,#30569,#30570,#30571,#30572,#30573),.UNSPECIFIED.,.F.,.F.,(4,1,1,
1,1,1,1,1,4),(72.2566310325652,72.4529079147974,73.4502437573497,74.4475795999019,
75.4449154424541,76.4422512850064,77.4395871275586,78.4369229701109,78.5398163397448),
 .UNSPECIFIED.);
#2287=B_SPLINE_CURVE_WITH_KNOTS('',3,(#30574,#30575,#30576,#30577,#30578,
#30579,#30580,#30581,#30582,#30583),.UNSPECIFIED.,.F.,.F.,(4,1,1,1,1,1,
1,4),(72.2566310325652,73.1810400136955,74.1790469843256,75.1770539549557,
76.1750609255857,77.1730678962158,78.1710748668459,78.5398163397448),
 .UNSPECIFIED.);
#2288=B_SPLINE_CURVE_WITH_KNOTS('',3,(#30588,#30589,#30590,#30591,#30592,
#30593,#30594,#30595,#30596,#30597),.UNSPECIFIED.,.F.,.F.,(4,1,1,1,1,1,
1,4),(65.9734457253856,66.468892859484,67.4662287020362,68.4635645445884,
69.4609003871407,70.4582362296929,71.4555720722452,72.2566310325652),
 .UNSPECIFIED.);
#2289=B_SPLINE_CURVE_WITH_KNOTS('',3,(#30598,#30599,#30600,#30601,#30602,
#30603,#30604,#30605,#30606,#30607,#30608),.UNSPECIFIED.,.F.,.F.,(4,1,1,
1,1,1,1,1,4),(65.9734457253856,66.1949912192848,67.1929981899149,68.191005160545,
69.1890121311751,70.1870191018052,71.1850260724353,72.1830330430654,72.2566310325652),
 .UNSPECIFIED.);
#2290=B_SPLINE_CURVE_WITH_KNOTS('',3,(#30613,#30614,#30615,#30616,#30617,
#30618,#30619,#30620,#30621,#30622),.UNSPECIFIED.,.F.,.F.,(4,1,1,1,1,1,
1,4),(59.690260418206,60.4848778041705,61.4822136467227,62.479549489275,
63.4768853318272,64.4742211743795,65.4715570169317,65.9734457253856),
 .UNSPECIFIED.);
#2291=B_SPLINE_CURVE_WITH_KNOTS('',3,(#30623,#30624,#30625,#30626,#30627,
#30628,#30629,#30630,#30631,#30632),.UNSPECIFIED.,.F.,.F.,(4,1,1,1,1,1,
1,4),(59.690260418206,60.2069493955043,61.2049563661344,62.2029633367645,
63.2009703073946,64.1989772780247,65.1969842486548,65.9734457253856),
 .UNSPECIFIED.);
#2292=B_SPLINE_CURVE_WITH_KNOTS('',3,(#30637,#30638,#30639,#30640,#30641,
#30642,#30643,#30644,#30645,#30646,#30647),.UNSPECIFIED.,.F.,.F.,(4,1,1,
1,1,1,1,1,4),(53.4070751110265,53.5035269063048,54.500862748857,55.4981985914093,
56.4955344339615,57.4928702765138,58.490206119066,59.4875419616182,59.690260418206),
 .UNSPECIFIED.);
#2293=B_SPLINE_CURVE_WITH_KNOTS('',3,(#30648,#30649,#30650,#30651,#30652,
#30653,#30654,#30655,#30656,#30657),.UNSPECIFIED.,.F.,.F.,(4,1,1,1,1,1,
1,4),(53.4070751110264,54.2189075717238,55.2169145423539,56.214921512984,
57.212928483614,58.2109354542441,59.2089424248742,59.690260418206),
 .UNSPECIFIED.);
#2294=B_SPLINE_CURVE_WITH_KNOTS('',3,(#30662,#30663,#30664,#30665,#30666,
#30667,#30668,#30669,#30670,#30671),.UNSPECIFIED.,.F.,.F.,(4,1,1,1,1,1,
1,4),(47.1238898038469,47.5195118509913,48.5168476935436,49.5141835360958,
50.5115193786481,51.5088552212003,52.5061910637525,53.4070751110265),
 .UNSPECIFIED.);
#2295=B_SPLINE_CURVE_WITH_KNOTS('',3,(#30672,#30673,#30674,#30675,#30676,
#30677,#30678,#30679,#30680,#30681,#30682),.UNSPECIFIED.,.F.,.F.,(4,1,1,
1,1,1,1,1,4),(47.1238898038468,47.2328587773132,48.2308657479432,49.2288727185733,
50.2268796892034,51.2248866598335,52.2228936304636,53.2209006010937,53.4070751110264),
 .UNSPECIFIED.);
#2296=B_SPLINE_CURVE_WITH_KNOTS('',3,(#30687,#30688,#30689,#30690,#30691,
#30692,#30693,#30694,#30695,#30696),.UNSPECIFIED.,.F.,.F.,(4,1,1,1,1,1,
1,4),(40.8407044966673,41.5354967956779,42.5328326382301,43.5301684807823,
44.5275043233346,45.5248401658868,46.5221760084391,47.1238898038469),
 .UNSPECIFIED.);
#2297=B_SPLINE_CURVE_WITH_KNOTS('',3,(#30697,#30698,#30699,#30700,#30701,
#30702,#30703,#30704,#30705,#30706),.UNSPECIFIED.,.F.,.F.,(4,1,1,1,1,1,
1,4),(40.8407044966672,41.2448169535326,42.2428239241627,43.2408308947928,
44.2388378654229,45.236844836053,46.2348518066831,47.1238898038468),
 .UNSPECIFIED.);
#2298=B_SPLINE_CURVE_WITH_KNOTS('',3,(#30711,#30712,#30713,#30714,#30715,
#30716,#30717,#30718,#30719,#30720),.UNSPECIFIED.,.F.,.F.,(4,1,1,1,1,1,
1,4),(34.5575191894877,35.5514817403644,36.5488175829166,37.5461534254689,
38.5434892680211,39.5408251105734,40.5381609531256,40.8407044966673),
 .UNSPECIFIED.);
#2299=B_SPLINE_CURVE_WITH_KNOTS('',3,(#30721,#30722,#30723,#30724,#30725,
#30726,#30727,#30728,#30729,#30730),.UNSPECIFIED.,.F.,.F.,(4,1,1,1,1,1,
1,4),(34.5575191894876,35.2567751297521,36.2547821003822,37.2527890710123,
38.2507960416424,39.2488030122724,40.2468099829025,40.8407044966672),
 .UNSPECIFIED.);
#2300=B_SPLINE_CURVE_WITH_KNOTS('',3,(#30735,#30736,#30737,#30738,#30739,
#30740,#30741,#30742,#30743,#30744,#30745),.UNSPECIFIED.,.F.,.F.,(4,1,1,
1,1,1,1,1,4),(28.2743338823081,28.5701308424987,29.5674666850509,30.5648025276032,
31.5621383701554,32.5594742127077,33.5568100552599,34.5541458978121,34.5575191894877),
 .UNSPECIFIED.);
#2301=B_SPLINE_CURVE_WITH_KNOTS('',3,(#30746,#30747,#30748,#30749,#30750,
#30751,#30752,#30753,#30754,#30755),.UNSPECIFIED.,.F.,.F.,(4,1,1,1,1,1,
1,4),(28.274333882308,29.2687333059716,30.2667402766016,31.2647472472317,
32.2627542178618,33.2607611884919,34.258768159122,34.5575191894876),
 .UNSPECIFIED.);
#2302=B_SPLINE_CURVE_WITH_KNOTS('',3,(#30760,#30761,#30762,#30763,#30764,
#30765,#30766,#30767,#30768,#30769),.UNSPECIFIED.,.F.,.F.,(4,1,1,1,1,1,
1,4),(21.9911485751285,22.5861157871852,23.5834516297375,24.5807874722897,
25.5781233148419,26.5754591573942,27.5727949999464,28.2743338823081),
 .UNSPECIFIED.);
#2303=B_SPLINE_CURVE_WITH_KNOTS('',3,(#30770,#30771,#30772,#30773,#30774,
#30775,#30776,#30777,#30778,#30779,#30780),.UNSPECIFIED.,.F.,.F.,(4,1,1,
1,1,1,1,1,4),(21.9911485751285,22.2826845115609,23.280691482191,24.2786984528211,
25.2767054234512,26.2747123940813,27.2727193647114,28.2707263353415,28.274333882308),
 .UNSPECIFIED.);
#2304=B_SPLINE_CURVE_WITH_KNOTS('',3,(#30785,#30786,#30787,#30788,#30789,
#30790,#30791,#30792,#30793,#30794),.UNSPECIFIED.,.F.,.F.,(4,1,1,1,1,1,
1,4),(15.7079632679489,16.6021007318718,17.599436574424,18.5967724169762,
19.5941082595285,20.5914441020807,21.588779944633,21.9911485751285),
 .UNSPECIFIED.);
#2305=B_SPLINE_CURVE_WITH_KNOTS('',3,(#30795,#30796,#30797,#30798,#30799,
#30800,#30801,#30802,#30803,#30804),.UNSPECIFIED.,.F.,.F.,(4,1,1,1,1,1,
1,4),(15.7079632679489,16.2946426877804,17.2926496584105,18.2906566290406,
19.2886635996707,20.2866705703008,21.2846775409308,21.9911485751285),
 .UNSPECIFIED.);
#2306=B_SPLINE_CURVE_WITH_KNOTS('',3,(#30807,#30808,#30809,#30810,#30811,
#30812,#30813,#30814,#30815,#30816,#30817,#30818,#30819,#30820,#30821,#30822,
#30823,#30824,#30825,#30826,#30827,#30828,#30829,#30830,#30831,#30832,#30833,
#30834,#30835,#30836,#30837,#30838,#30839,#30840,#30841,#30842,#30843,#30844,
#30845,#30846,#30847,#30848,#30849,#30850,#30851,#30852,#30853,#30854,#30855,
#30856,#30857,#30858,#30859,#30860,#30861,#30862,#30863,#30864,#30865,#30866,
#30867,#30868,#30869,#30870,#30871,#30872,#30873,#30874,#30875,#30876,#30877,
#30878,#30879,#30880,#30881,#30882,#30883,#30884,#30885),.UNSPECIFIED.,
 .F.,.F.,(4,3,3,3,3,3,3,3,3,3,3,3,3,3,3,3,3,3,3,3,3,3,3,3,3,3,4),(-0.996917990983956,
-0.964197655296454,-0.951513094737375,-0.939590005196496,-0.910398139253692,
-0.896458168447615,-0.866624051431682,-0.848513043381918,-0.839276821658768,
-0.836789934415749,-0.803176729602168,-0.780362864215826,-0.769651322799483,
-0.734439153414668,-0.711686399207869,-0.700944767019061,-0.669566542377212,
-0.648981044332524,-0.637888877288902,-0.602287825523676,-0.584615028650125,
-0.570052223933311,-0.532768447080654,-0.516116381189141,-0.50154558318824,
-0.495484670227998,-0.468408511919796),.UNSPECIFIED.);
#2307=B_SPLINE_CURVE_WITH_KNOTS('',3,(#30887,#30888,#30889,#30890,#30891,
#30892,#30893,#30894,#30895,#30896,#30897,#30898,#30899,#30900,#30901,#30902,
#30903,#30904,#30905,#30906,#30907,#30908,#30909,#30910,#30911,#30912,#30913,
#30914,#30915,#30916,#30917,#30918,#30919,#30920),.UNSPECIFIED.,.F.,.F.,
(4,3,3,3,3,3,3,3,3,3,3,4),(-0.271362855059921,-0.23333358174471,-0.202109628804149,
-0.191194824123734,-0.172574372312687,-0.139871461148431,-0.130049418747569,
-0.0948265930323134,-0.0669749700089491,-0.0565955729248257,-0.0239539643597006,
0.),.UNSPECIFIED.);
#2308=B_SPLINE_CURVE_WITH_KNOTS('',3,(#30923,#30924,#30925,#30926,#30927,
#30928,#30929,#30930,#30931,#30932,#30933,#30934,#30935,#30936,#30937,#30938,
#30939,#30940,#30941,#30942,#30943,#30944,#30945,#30946,#30947,#30948,#30949,
#30950,#30951,#30952,#30953,#30954,#30955,#30956,#30957,#30958,#30959,#30960,
#30961,#30962,#30963,#30964,#30965,#30966,#30967,#30968,#30969,#30970,#30971,
#30972,#30973,#30974,#30975,#30976,#30977,#30978,#30979,#30980,#30981,#30982,
#30983,#30984,#30985,#30986),.UNSPECIFIED.,.F.,.F.,(4,3,3,3,3,3,3,3,3,3,
3,3,3,3,3,3,3,3,3,3,3,4),(-0.468408511919796,-0.44532089356327,-0.431869826400524,
-0.394574417707956,-0.377959024336246,-0.36718387876206,-0.329707820210052,
-0.314417154781481,-0.297766482794163,-0.286364248592707,-0.248901620010442,
-0.233074500624702,-0.216543640108336,-0.17799293612575,-0.152182016671258,
-0.141011423916894,-0.12652726456846,-0.094895448426345,-0.0796457512037788,
-0.0683009962329189,-0.0289678476755453,0.),.UNSPECIFIED.);
#2309=B_SPLINE_CURVE_WITH_KNOTS('',3,(#31415,#31416,#31417,#31418,#31419,
#31420,#31421,#31422),.UNSPECIFIED.,.F.,.F.,(4,1,1,1,1,4),(11.6154215191105,
12.6127573616628,13.610093204215,14.6074290467673,15.6047648893195,15.7079632679489),
 .UNSPECIFIED.);
#2310=B_SPLINE_CURVE_WITH_KNOTS('',3,(#31423,#31424,#31425,#31426,#31427,
#31428,#31429,#31430,#31431,#31432,#31433,#31434,#31435,#31436,#31437,#31438,
#31439,#31440,#31441,#31442,#31443,#31444,#31445,#31446,#31447,#31448,#31449,
#31450,#31451,#31452,#31453,#31454,#31455,#31456,#31457,#31458,#31459,#31460,
#31461,#31462,#31463,#31464,#31465,#31466,#31467,#31468,#31469,#31470,#31471,
#31472,#31473,#31474,#31475,#31476,#31477,#31478,#31479,#31480),
 .UNSPECIFIED.,.F.,.F.,(4,3,3,3,3,3,3,3,3,3,3,3,3,3,3,3,3,3,3,4),(-0.364629307890661,
-0.350885759085945,-0.324346713718219,-0.304152838893849,-0.282934787914253,
-0.264003466919189,-0.252764227803326,-0.216347623970161,-0.198031500011342,
-0.186602740018901,-0.166173598315468,-0.146000730648533,-0.128382123165429,
-0.119003916100956,-0.0892529370757172,-0.0724905256163614,-0.0619084956994276,
-0.0517443199161659,-0.0194955210690912,0.),.UNSPECIFIED.);
#2311=B_SPLINE_CURVE_WITH_KNOTS('',3,(#31481,#31482,#31483,#31484,#31485,
#31486,#31487,#31488,#31489,#31490,#31491,#31492,#31493),.UNSPECIFIED.,
 .F.,.F.,(4,3,3,3,4),(-101.213804280572,-100.730920097777,-99.7335842552244,
-98.7362484126722,-98.3403213565322),.UNSPECIFIED.);
#2312=B_SPLINE_CURVE_WITH_KNOTS('',3,(#31496,#31497,#31498,#31499,#31500,
#31501,#31502,#31503,#31504),.UNSPECIFIED.,.F.,.F.,(4,1,1,1,1,1,4),(10.3757270560178,
11.30460783463,12.30261480526,13.3006217758901,14.2986287465202,15.2966357171503,
15.7079632679489),.UNSPECIFIED.);
#2313=B_SPLINE_CURVE_WITH_KNOTS('',3,(#31938,#31939,#31940,#31941,#31942,
#31943,#31944,#31945,#31946,#31947,#31948,#31949,#31950,#31951,#31952,#31953),
 .UNSPECIFIED.,.F.,.F.,(4,3,3,3,3,4),(95.3619706457233,95.8086691804886,
96.8066761511186,97.8046831217487,98.8026900923788,99.1486641472938),
 .UNSPECIFIED.);
#2314=B_SPLINE_CURVE_WITH_KNOTS('',3,(#31954,#31955,#31956,#31957,#31958,
#31959,#31960,#31961,#31962,#31963,#31964,#31965,#31966,#31967,#31968,#31969,
#31970,#31971,#31972,#31973,#31974,#31975,#31976,#31977,#31978,#31979,#31980,
#31981,#31982,#31983,#31984,#31985,#31986,#31987,#31988,#31989,#31990,#31991,
#31992,#31993,#31994,#31995,#31996,#31997,#31998,#31999,#32000,#32001,#32002,
#32003,#32004,#32005),.UNSPECIFIED.,.F.,.F.,(4,3,3,3,3,3,3,3,3,3,3,3,3,
3,3,3,3,4),(-0.366397579005845,-0.355461226466819,-0.328804438442731,-0.31606471842091,
-0.292558951597566,-0.280250898914551,-0.245275213061006,-0.218626183485931,
-0.207947804736759,-0.187209422476688,-0.163808244667102,-0.149577787474042,
-0.13876424622794,-0.104073184670955,-0.0827908372522071,-0.0667764467402658,
-0.0282827470320728,0.),.UNSPECIFIED.);
#2315=B_SPLINE_CURVE_WITH_KNOTS('',3,(#32059,#32060,#32061,#32062,#32063,
#32064,#32065,#32066,#32067,#32068),.UNSPECIFIED.,.F.,.F.,(4,3,3,4),(-4.09202352044854,
-3.99291737327004,-2.99468802995253,-2.07317267331973),.UNSPECIFIED.);
#2316=B_SPLINE_CURVE_WITH_KNOTS('',3,(#32071,#32072,#32073,#32074,#32075,
#32076,#32077),.UNSPECIFIED.,.F.,.F.,(4,3,4),(0.,0.999341140225982,1.12274180646093),
 .UNSPECIFIED.);
#2317=B_SPLINE_CURVE_WITH_KNOTS('',3,(#32082,#32083,#32084,#32085,#32086,
#32087,#32088,#32089,#32090,#32091,#32092,#32093,#32094,#32095,#32096,#32097,
#32098,#32099,#32100,#32101,#32102,#32103),.UNSPECIFIED.,.F.,.F.,(4,3,3,
3,3,3,3,4),(-10.3752088276281,-9.9822934331751,-8.98406408985759,-7.98583474654008,
-6.98760540322257,-5.98937605990506,-4.99114671658755,-4.09202352044854),
 .UNSPECIFIED.);
#2318=B_SPLINE_CURVE_WITH_KNOTS('',3,(#32104,#32105,#32106,#32107,#32108,
#32109,#32110,#32111,#32112,#32113,#32114,#32115,#32116,#32117,#32118,#32119,
#32120,#32121,#32122,#32123,#32124,#32125),.UNSPECIFIED.,.F.,.F.,(4,3,3,
3,3,3,3,4),(1.12274180646093,1.99868228045197,2.99802342067795,3.99736456090394,
4.99670570112992,5.99604684135591,6.99538798158189,7.40592711364052),
 .UNSPECIFIED.);
#2319=B_SPLINE_CURVE_WITH_KNOTS('',3,(#32130,#32131,#32132,#32133,#32134,
#32135,#32136,#32137,#32138,#32139,#32140,#32141,#32142,#32143,#32144,#32145,
#32146,#32147,#32148,#32149,#32150,#32151),.UNSPECIFIED.,.F.,.F.,(4,3,3,
3,3,3,3,4),(-16.6583941348077,-15.9716694930802,-14.9734401497627,-13.9752108064451,
-12.9769814631276,-11.9787521198101,-10.9805227764926,-10.3752088276281),
 .UNSPECIFIED.);
#2320=B_SPLINE_CURVE_WITH_KNOTS('',3,(#32152,#32153,#32154,#32155,#32156,
#32157,#32158,#32159,#32160,#32161,#32162,#32163,#32164,#32165,#32166,#32167,
#32168,#32169,#32170,#32171,#32172,#32173),.UNSPECIFIED.,.F.,.F.,(4,3,3,
3,3,3,3,4),(7.40592711364052,7.99472912180787,8.99407026203386,9.99341140225984,
10.9927525424858,11.9920936827118,12.9914348229378,13.6891124208201),
 .UNSPECIFIED.);
#2321=B_SPLINE_CURVE_WITH_KNOTS('',3,(#32178,#32179,#32180,#32181,#32182,
#32183,#32184,#32185,#32186,#32187,#32188,#32189,#32190,#32191,#32192,#32193,
#32194,#32195,#32196,#32197,#32198,#32199),.UNSPECIFIED.,.F.,.F.,(4,3,3,
3,3,3,3,4),(-22.9415794419873,-21.9610455529852,-20.9628162096677,-19.9645868663502,
-18.9663575230327,-17.9681281797152,-16.9698988363977,-16.6583941348077),
 .UNSPECIFIED.);
#2322=B_SPLINE_CURVE_WITH_KNOTS('',3,(#32200,#32201,#32202,#32203,#32204,
#32205,#32206,#32207,#32208,#32209,#32210,#32211,#32212,#32213,#32214,#32215,
#32216,#32217,#32218,#32219,#32220,#32221),.UNSPECIFIED.,.F.,.F.,(4,3,3,
3,3,3,3,4),(13.6891124208201,13.9907759631638,14.9901171033898,15.9894582436157,
16.9887993838417,17.9881405240677,18.9874816642937,19.9722977279997),
 .UNSPECIFIED.);
#2323=B_SPLINE_CURVE_WITH_KNOTS('',3,(#32226,#32227,#32228,#32229,#32230,
#32231,#32232,#32233,#32234,#32235,#32236,#32237,#32238,#32239,#32240,#32241,
#32242,#32243,#32244,#32245,#32246,#32247,#32248,#32249,#32250),
 .UNSPECIFIED.,.F.,.F.,(4,3,3,3,3,3,3,3,4),(-29.2247647491669,-28.9486509562078,
-27.9504216128903,-26.9521922695728,-25.9539629262553,-24.9557335829378,
-23.9575042396202,-22.9592748963027,-22.9415794419873),.UNSPECIFIED.);
#2324=B_SPLINE_CURVE_WITH_KNOTS('',3,(#32251,#32252,#32253,#32254,#32255,
#32256,#32257,#32258,#32259,#32260,#32261,#32262,#32263,#32264,#32265,#32266,
#32267,#32268,#32269,#32270,#32271,#32272,#32273,#32274,#32275),
 .UNSPECIFIED.,.F.,.F.,(4,3,3,3,3,3,3,3,4),(19.9722977279997,19.9868228045197,
20.9861639447457,21.9855050849716,22.9848462251976,23.9841873654236,24.9835285056496,
25.9828696458756,26.2554830351793),.UNSPECIFIED.);
#2325=B_SPLINE_CURVE_WITH_KNOTS('',3,(#32280,#32281,#32282,#32283,#32284,
#32285,#32286,#32287,#32288,#32289,#32290,#32291,#32292,#32293,#32294,#32295,
#32296,#32297,#32298,#32299,#32300,#32301),.UNSPECIFIED.,.F.,.F.,(4,3,3,
3,3,3,3,4),(-35.5079500563465,-34.9380270161129,-33.9397976727954,-32.9415683294778,
-31.9433389861603,-30.9451096428428,-29.9468802995253,-29.2247647491669),
 .UNSPECIFIED.);
#2326=B_SPLINE_CURVE_WITH_KNOTS('',3,(#32302,#32303,#32304,#32305,#32306,
#32307,#32308,#32309,#32310,#32311,#32312,#32313,#32314,#32315,#32316,#32317,
#32318,#32319,#32320,#32321,#32322,#32323),.UNSPECIFIED.,.F.,.F.,(4,3,3,
3,3,3,3,4),(26.2554830351793,26.9822107861016,27.9815519263275,28.9808930665535,
29.9802342067795,30.9795753470055,31.9789164872315,32.5386683423589),
 .UNSPECIFIED.);
#2327=B_SPLINE_CURVE_WITH_KNOTS('',3,(#32328,#32329,#32330,#32331,#32332,
#32333,#32334,#32335,#32336,#32337,#32338,#32339,#32340,#32341,#32342,#32343,
#32344,#32345,#32346,#32347,#32348,#32349),.UNSPECIFIED.,.F.,.F.,(4,3,3,
3,3,3,3,4),(-41.7911353635261,-40.9274030760179,-39.9291737327004,-38.9309443893829,
-37.9327150460654,-36.9344857027479,-35.9362563594304,-35.5079500563465),
 .UNSPECIFIED.);
#2328=B_SPLINE_CURVE_WITH_KNOTS('',3,(#32350,#32351,#32352,#32353,#32354,
#32355,#32356,#32357,#32358,#32359,#32360,#32361,#32362,#32363,#32364,#32365,
#32366,#32367,#32368,#32369,#32370,#32371),.UNSPECIFIED.,.F.,.F.,(4,3,3,
3,3,3,3,4),(32.5386683423589,32.9782576274575,33.9775987676834,34.9769399079094,
35.9762810481354,36.9756221883614,37.9749633285874,38.8218536495385),
 .UNSPECIFIED.);
#2329=B_SPLINE_CURVE_WITH_KNOTS('',3,(#32376,#32377,#32378,#32379,#32380,
#32381,#32382,#32383,#32384,#32385,#32386,#32387,#32388,#32389,#32390,#32391,
#32392,#32393,#32394,#32395,#32396,#32397,#32398,#32399,#32400),
 .UNSPECIFIED.,.F.,.F.,(4,3,3,3,3,3,3,3,4),(-48.0743206707057,-47.9150084792405,
-46.916779135923,-45.9185497926055,-44.920320449288,-43.9220911059705,-42.9238617626529,
-41.9256324193354,-41.7911353635261),.UNSPECIFIED.);
#2330=B_SPLINE_CURVE_WITH_KNOTS('',3,(#32401,#32402,#32403,#32404,#32405,
#32406,#32407,#32408,#32409,#32410,#32411,#32412,#32413,#32414,#32415,#32416,
#32417,#32418,#32419,#32420,#32421,#32422,#32423,#32424,#32425),
 .UNSPECIFIED.,.F.,.F.,(4,3,3,3,3,3,3,3,4),(38.8218536495385,38.9743044688134,
39.9736456090394,40.9729867492653,41.9723278894913,42.9716690297173,43.9710101699433,
44.9703513101693,45.105038956718),.UNSPECIFIED.);
#2331=B_SPLINE_CURVE_WITH_KNOTS('',3,(#32430,#32431,#32432,#32433,#32434,
#32435,#32436,#32437,#32438,#32439,#32440,#32441,#32442,#32443,#32444,#32445,
#32446,#32447,#32448,#32449,#32450,#32451),.UNSPECIFIED.,.F.,.F.,(4,3,3,
3,3,3,3,4),(-54.3575059778853,-53.9043845391456,-52.906155195828,-51.9079258525105,
-50.909696509193,-49.9114671658755,-48.913237822558,-48.0743206707057),
 .UNSPECIFIED.);
#2332=B_SPLINE_CURVE_WITH_KNOTS('',3,(#32452,#32453,#32454,#32455,#32456,
#32457,#32458,#32459,#32460,#32461,#32462,#32463,#32464,#32465,#32466,#32467,
#32468,#32469,#32470,#32471,#32472,#32473),.UNSPECIFIED.,.F.,.F.,(4,3,3,
3,3,3,3,4),(45.105038956718,45.9696924503953,46.9690335906212,47.9683747308472,
48.9677158710732,49.9670570112992,50.9663981515252,51.3882242638976),
 .UNSPECIFIED.);
#2333=B_SPLINE_CURVE_WITH_KNOTS('',3,(#32478,#32479,#32480,#32481,#32482,
#32483,#32484,#32485,#32486,#32487,#32488,#32489,#32490,#32491,#32492,#32493,
#32494,#32495,#32496,#32497,#32498,#32499),.UNSPECIFIED.,.F.,.F.,(4,3,3,
3,3,3,3,4),(-60.6406912850648,-59.8937605990506,-58.8955312557331,-57.8973019124156,
-56.8990725690981,-55.9008432257806,-54.9026138824631,-54.3575059778853),
 .UNSPECIFIED.);
#2334=B_SPLINE_CURVE_WITH_KNOTS('',3,(#32500,#32501,#32502,#32503,#32504,
#32505,#32506,#32507,#32508,#32509,#32510,#32511,#32512,#32513,#32514,#32515,
#32516,#32517,#32518,#32519,#32520,#32521),.UNSPECIFIED.,.F.,.F.,(4,3,3,
3,3,3,3,4),(51.3882242638976,51.9657392917511,52.9650804319771,53.9644215722031,
54.9637627124291,55.9631038526551,56.9624449928811,57.6714095710772),
 .UNSPECIFIED.);
#2335=B_SPLINE_CURVE_WITH_KNOTS('',3,(#32527,#32528,#32529,#32530,#32531,
#32532,#32533,#32534,#32535,#32536),.UNSPECIFIED.,.F.,.F.,(4,1,1,1,1,1,
1,4),(72.2566310325653,72.5079296898685,73.506159033186,74.5043883765035,
75.502617719821,76.5008470631385,77.499076406456,78.4973057497735),
 .UNSPECIFIED.);
#2336=B_SPLINE_CURVE_WITH_KNOTS('',3,(#32539,#32540,#32541,#32542,#32543,
#32544,#32545,#32546,#32547),.UNSPECIFIED.,.F.,.F.,(4,1,1,1,1,1,4),(72.2566310325652,
72.2598691287713,73.2592102689973,74.2585514092233,75.2578925494492,76.2572336896752,
77.2565748299012),.UNSPECIFIED.);
#2337=B_SPLINE_CURVE_WITH_KNOTS('',3,(#32552,#32553,#32554,#32555,#32556,
#32557,#32558,#32559,#32560,#32561),.UNSPECIFIED.,.F.,.F.,(4,1,1,1,1,1,
1,4),(65.9734457253856,66.5185536299634,67.5167829732809,68.5150123165984,
69.513241659916,70.5114710032335,71.509700346551,72.2566310325653),
 .UNSPECIFIED.);
#2338=B_SPLINE_CURVE_WITH_KNOTS('',3,(#32562,#32563,#32564,#32565,#32566,
#32567,#32568,#32569,#32570,#32571),.UNSPECIFIED.,.F.,.F.,(4,1,1,1,1,1,
1,4),(65.9734457253856,66.2638222874154,67.2631634276414,68.2625045678674,
69.2618457080933,70.2611868483193,71.2605279885453,72.2566310325652),
 .UNSPECIFIED.);
#2339=B_SPLINE_CURVE_WITH_KNOTS('',3,(#32576,#32577,#32578,#32579,#32580,
#32581,#32582,#32583,#32584,#32585),.UNSPECIFIED.,.F.,.F.,(4,1,1,1,1,1,
1,4),(59.6902604182061,60.5291775700584,61.5274069133759,62.5256362566934,
63.5238656000109,64.5220949433284,65.5203242866459,65.9734457253856),
 .UNSPECIFIED.);
#2340=B_SPLINE_CURVE_WITH_KNOTS('',3,(#32586,#32587,#32588,#32589,#32590,
#32591,#32592,#32593,#32594,#32595),.UNSPECIFIED.,.F.,.F.,(4,1,1,1,1,1,
1,4),(59.6902604182061,60.2677754460595,61.2671165862855,62.2664577265115,
63.2657988667374,64.2651400069634,65.2644811471894,65.9734457253856),
 .UNSPECIFIED.);
#2341=B_SPLINE_CURVE_WITH_KNOTS('',3,(#32600,#32601,#32602,#32603,#32604,
#32605,#32606,#32607,#32608,#32609,#32610),.UNSPECIFIED.,.F.,.F.,(4,1,1,
1,1,1,1,1,4),(53.4070751110265,53.5415721668358,54.5398015101533,55.5380308534708,
56.5362601967883,57.5344895401058,58.5327188834233,59.5309482267409,59.6902604182061),
 .UNSPECIFIED.);
#2342=B_SPLINE_CURVE_WITH_KNOTS('',3,(#32611,#32612,#32613,#32614,#32615,
#32616,#32617,#32618,#32619,#32620),.UNSPECIFIED.,.F.,.F.,(4,1,1,1,1,1,
1,4),(53.4070751110265,54.2717286047036,55.2710697449296,56.2704108851556,
57.2697520253815,58.2690931656075,59.2684343058335,59.6902604182061),
 .UNSPECIFIED.);
#2343=B_SPLINE_CURVE_WITH_KNOTS('',3,(#32625,#32626,#32627,#32628,#32629,
#32630,#32631,#32632,#32633,#32634),.UNSPECIFIED.,.F.,.F.,(4,1,1,1,1,1,
1,4),(47.1238898038469,47.5521961069307,48.5504254502482,49.5486547935658,
50.5468841368833,51.5451134802008,52.5433428235183,53.4070751110265),
 .UNSPECIFIED.);
#2344=B_SPLINE_CURVE_WITH_KNOTS('',3,(#32635,#32636,#32637,#32638,#32639,
#32640,#32641,#32642,#32643,#32644,#32645),.UNSPECIFIED.,.F.,.F.,(4,1,1,
1,1,1,1,1,4),(47.1238898038469,47.2763406231217,48.2756817633477,49.2750229035737,
50.2743640437997,51.2737051840256,52.2730463242516,53.2723874644776,53.4070751110265),
 .UNSPECIFIED.);
#2345=B_SPLINE_CURVE_WITH_KNOTS('',3,(#32650,#32651,#32652,#32653,#32654,
#32655,#32656,#32657,#32658,#32659),.UNSPECIFIED.,.F.,.F.,(4,1,1,1,1,1,
1,4),(40.8407044966673,41.5628200470257,42.5610493903432,43.5592787336607,
44.5575080769782,45.5557374202957,46.5539667636132,47.1238898038469),
 .UNSPECIFIED.);
#2346=B_SPLINE_CURVE_WITH_KNOTS('',3,(#32660,#32661,#32662,#32663,#32664,
#32665,#32666,#32667,#32668,#32669),.UNSPECIFIED.,.F.,.F.,(4,1,1,1,1,1,
1,4),(40.8407044966673,41.2802937817658,42.2796349219918,43.2789760622178,
44.2783172024438,45.2776583426697,46.2769994828957,47.1238898038469),
 .UNSPECIFIED.);
#2347=B_SPLINE_CURVE_WITH_KNOTS('',3,(#32674,#32675,#32676,#32677,#32678,
#32679,#32680,#32681,#32682,#32683,#32684),.UNSPECIFIED.,.F.,.F.,(4,1,1,
1,1,1,1,1,4),(34.5575191894877,34.5752146438031,35.5734439871206,36.5716733304381,
37.5699026737556,38.5681320170731,39.5663613603907,40.5645907037082,40.8407044966673),
 .UNSPECIFIED.);
#2348=B_SPLINE_CURVE_WITH_KNOTS('',3,(#32685,#32686,#32687,#32688,#32689,
#32690,#32691,#32692,#32693,#32694),.UNSPECIFIED.,.F.,.F.,(4,1,1,1,1,1,
1,4),(34.5575191894877,35.2842469404099,36.2835880806359,37.2829292208619,
38.2822703610879,39.2816115013138,40.2809526415398,40.8407044966673),
 .UNSPECIFIED.);
#2349=B_SPLINE_CURVE_WITH_KNOTS('',3,(#32699,#32700,#32701,#32702,#32703,
#32704,#32705,#32706,#32707,#32708),.UNSPECIFIED.,.F.,.F.,(4,1,1,1,1,1,
1,4),(28.2743338823081,28.585838583898,29.5840679272155,30.5822972705331,
31.5805266138506,32.5787559571681,33.5769853004856,34.5575191894877),
 .UNSPECIFIED.);
#2350=B_SPLINE_CURVE_WITH_KNOTS('',3,(#32709,#32710,#32711,#32712,#32713,
#32714,#32715,#32716,#32717,#32718,#32719),.UNSPECIFIED.,.F.,.F.,(4,1,1,
1,1,1,1,1,4),(28.2743338823081,28.288858958828,29.288200099054,30.28754123928,
31.286882379506,32.2862235197319,33.2855646599579,34.2849058001839,34.5575191894877),
 .UNSPECIFIED.);
#2351=B_SPLINE_CURVE_WITH_KNOTS('',3,(#32724,#32725,#32726,#32727,#32728,
#32729,#32730,#32731,#32732,#32733),.UNSPECIFIED.,.F.,.F.,(4,1,1,1,1,1,
1,4),(21.9911485751285,22.596462523993,23.5946918673105,24.592921210628,
25.5911505539455,26.589379897263,27.5876092405805,28.2743338823081),
 .UNSPECIFIED.);
#2352=B_SPLINE_CURVE_WITH_KNOTS('',3,(#32734,#32735,#32736,#32737,#32738,
#32739,#32740,#32741,#32742,#32743),.UNSPECIFIED.,.F.,.F.,(4,1,1,1,1,1,
1,4),(21.9911485751285,22.2928121174721,23.2921532576981,24.2914943979241,
25.2908355381501,26.290176678376,27.289517818602,28.2743338823081),
 .UNSPECIFIED.);
#2353=B_SPLINE_CURVE_WITH_KNOTS('',3,(#32748,#32749,#32750,#32751,#32752,
#32753,#32754,#32755,#32756,#32757),.UNSPECIFIED.,.F.,.F.,(4,1,1,1,1,1,
1,4),(15.7079632679489,16.6070864640879,17.6053158074054,18.6035451507229,
19.6017744940404,20.600003837358,21.5982331806755,21.9911485751285),
 .UNSPECIFIED.);
#2354=B_SPLINE_CURVE_WITH_KNOTS('',3,(#32758,#32759,#32760,#32761,#32762,
#32763,#32764,#32765,#32766,#32767),.UNSPECIFIED.,.F.,.F.,(4,1,1,1,1,1,
1,4),(15.7079632679489,16.2967652761162,17.2961064163422,18.2954475565682,
19.2947886967942,20.2941298370201,21.2934709772461,21.9911485751285),
 .UNSPECIFIED.);
#2355=B_SPLINE_CURVE_WITH_KNOTS('',3,(#32770,#32771,#32772,#32773,#32774,
#32775,#32776,#32777,#32778,#32779,#32780,#32781,#32782,#32783,#32784,#32785,
#32786,#32787,#32788,#32789,#32790,#32791,#32792,#32793,#32794,#32795,#32796,
#32797,#32798,#32799,#32800,#32801,#32802,#32803,#32804,#32805,#32806,#32807,
#32808,#32809,#32810,#32811,#32812,#32813,#32814,#32815,#32816,#32817,#32818,
#32819,#32820,#32821,#32822,#32823,#32824,#32825,#32826,#32827,#32828,#32829,
#32830,#32831,#32832,#32833,#32834,#32835,#32836,#32837,#32838,#32839,#32840,
#32841,#32842,#32843,#32844,#32845,#32846,#32847,#32848,#32849,#32850,#32851,
#32852,#32853,#32854,#32855,#32856,#32857,#32858,#32859,#32860,#32861,#32862,
#32863,#32864,#32865,#32866,#32867,#32868,#32869,#32870,#32871,#32872,#32873,
#32874,#32875,#32876,#32877,#32878,#32879,#32880,#32881,#32882,#32883,#32884,
#32885,#32886,#32887,#32888,#32889,#32890,#32891,#32892,#32893),
 .UNSPECIFIED.,.F.,.F.,(4,3,3,3,3,3,3,3,3,3,3,3,3,3,3,3,3,3,3,3,3,3,3,3,
3,3,3,3,3,3,3,3,3,3,3,3,3,3,3,3,3,4),(-0.753008129282183,-0.726412785409006,
-0.715916399573649,-0.694852053413067,-0.683242780289961,-0.673766450589417,
-0.652778815266657,-0.639500919906121,-0.631791179943898,-0.604637195598433,
-0.591408327349303,-0.58243092328052,-0.553935160168246,-0.540392555827386,
-0.528208940192808,-0.505508318677634,-0.491429191967348,-0.477982436820105,
-0.452062180399923,-0.438863938010204,-0.427153921531904,-0.400727666335641,
-0.382198730280871,-0.374301411139377,-0.345303428221882,-0.331998698266984,
-0.322788462765202,-0.292662279142726,-0.279737557595205,-0.270213961274558,
-0.2400599353808,-0.238094602813322,-0.224912522130576,-0.21640841250359,
-0.186556730675161,-0.170795284707343,-0.161336087437576,-0.129168886313724,
-0.116523493465494,-0.106577361616136,-0.097001685189873,-0.096536015547866),
 .UNSPECIFIED.);
#2356=B_SPLINE_CURVE_WITH_KNOTS('',3,(#32895,#32896,#32897,#32898,#32899,
#32900,#32901,#32902,#32903,#32904,#32905,#32906,#32907,#32908,#32909,#32910,
#32911,#32912,#32913,#32914,#32915,#32916,#32917,#32918,#32919,#32920,#32921,
#32922,#32923,#32924,#32925,#32926,#32927,#32928,#32929,#32930,#32931),
 .UNSPECIFIED.,.F.,.F.,(4,3,3,3,3,3,3,3,3,3,3,3,4),(-0.204609524178328,
-0.17392271218969,-0.152224313672341,-0.142809800777549,-0.129914959151416,
-0.113620867578377,-0.100585910230378,-0.0924114342381335,-0.0693085756786001,
-0.0545304238088379,-0.0417479715798885,-0.0152833907299223,0.),
 .UNSPECIFIED.);
#2357=B_SPLINE_CURVE_WITH_KNOTS('',3,(#32934,#32935,#32936,#32937,#32938,
#32939,#32940,#32941,#32942,#32943,#32944,#32945,#32946,#32947,#32948,#32949),
 .UNSPECIFIED.,.F.,.F.,(4,3,3,3,3,4),(-0.096536015547866,-0.0724020116608995,
-0.0590251911255789,-0.0503900123732228,-0.0186970194324831,0.),
 .UNSPECIFIED.);
#2358=B_SPLINE_CURVE_WITH_KNOTS('',3,(#33234,#33235,#33236,#33237,#33238,
#33239,#33240,#33241),.UNSPECIFIED.,.F.,.F.,(4,1,1,1,1,4),(11.6159397475004,
12.6141690908179,13.6123984341354,14.6106277774529,15.6088571207704,15.7079632679489),
 .UNSPECIFIED.);
#2359=B_SPLINE_CURVE_WITH_KNOTS('',3,(#33242,#33243,#33244,#33245,#33246,
#33247,#33248,#33249,#33250,#33251,#33252,#33253,#33254,#33255,#33256,#33257,
#33258,#33259,#33260,#33261,#33262,#33263,#33264,#33265,#33266,#33267,#33268,
#33269,#33270,#33271,#33272,#33273,#33274,#33275,#33276,#33277,#33278,#33279,
#33280,#33281,#33282,#33283,#33284,#33285,#33286,#33287,#33288,#33289,#33290),
 .UNSPECIFIED.,.F.,.F.,(4,3,3,3,3,3,3,3,3,3,3,3,3,3,3,3,4),(-0.275362278356883,
-0.264159546247523,-0.242523917618953,-0.228489201611509,-0.209076761803474,
-0.198077656999141,-0.168436231356347,-0.151777330299101,-0.139830254922987,
-0.12544363295055,-0.101855794992709,-0.0891849033129337,-0.0668886774847003,
-0.0515641266869526,-0.0405229119346731,-0.0142790183076863,0.),
 .UNSPECIFIED.);
#2360=B_SPLINE_CURVE_WITH_KNOTS('',3,(#33291,#33292,#33293,#33294,#33295,
#33296,#33297,#33298,#33299,#33300,#33301,#33302,#33303,#33304,#33305,#33306,
#33307,#33308,#33309),.UNSPECIFIED.,.F.,.F.,(4,3,3,3,3,3,4),(-65.3636982725397,
-64.8849073156381,-63.8866779723206,-62.8884486290032,-61.8902192856856,
-60.8919899423681,-60.6406912850648),.UNSPECIFIED.);
#2361=B_SPLINE_CURVE_WITH_KNOTS('',3,(#33312,#33313,#33314,#33315,#33316,
#33317,#33318,#33319,#33320),.UNSPECIFIED.,.F.,.F.,(4,1,1,1,1,1,4),(10.375208827628,
11.3000595749863,12.2994007152123,13.2987418554383,14.2980829956642,15.2974241358902,
15.7079632679489),.UNSPECIFIED.);
#2362=B_SPLINE_CURVE_WITH_KNOTS('',3,(#33610,#33611,#33612,#33613,#33614,
#33615,#33616,#33617,#33618,#33619,#33620,#33621,#33622,#33623,#33624,#33625,
#33626,#33627,#33628,#33629,#33630,#33631),.UNSPECIFIED.,.F.,.F.,(4,3,3,
3,3,3,3,4),(57.6714095710772,57.9617861331071,58.961127273333,59.960468413559,
60.959809553785,61.959150694011,62.958491834237,63.29052559922),
 .UNSPECIFIED.);
#2363=B_SPLINE_CURVE_WITH_KNOTS('',3,(#33632,#33633,#33634,#33635,#33636,
#33637,#33638,#33639,#33640,#33641,#33642,#33643,#33644,#33645,#33646,#33647,
#33648,#33649,#33650,#33651,#33652,#33653,#33654,#33655,#33656,#33657,#33658,
#33659,#33660,#33661,#33662,#33663,#33664,#33665,#33666,#33667,#33668,#33669,
#33670,#33671,#33672,#33673,#33674,#33675,#33676,#33677,#33678,#33679,#33680,
#33681,#33682,#33683),.UNSPECIFIED.,.F.,.F.,(4,3,3,3,3,3,3,3,3,3,3,3,3,
3,3,3,3,4),(-0.276631791712725,-0.267716618892456,-0.246046101828633,-0.235289362386452,
-0.214941892616146,-0.204749662554743,-0.176256346031651,-0.161806307413905,
-0.15286753466007,-0.140652476775023,-0.120886137603943,-0.110226811379351,
-0.100669960776508,-0.0755024705823808,-0.058604244392821,-0.0491682800449266,
-0.0181536719473738,0.),.UNSPECIFIED.);
#2364=B_SPLINE_CURVE_WITH_KNOTS('',3,(#33737,#33738,#33739,#33740,#33741,
#33742,#33743,#33744,#33745,#33746),.UNSPECIFIED.,.F.,.F.,(4,3,3,4),(-4.09202352044855,
-3.97107960880372,-2.97830970660279,-2.07317267331974),.UNSPECIFIED.);
#2365=B_SPLINE_CURVE_WITH_KNOTS('',3,(#33749,#33750,#33751,#33752,#33753,
#33754,#33755),.UNSPECIFIED.,.F.,.F.,(4,3,4),(0.,0.993500176108578,1.12274180646087),
 .UNSPECIFIED.);
#2366=B_SPLINE_CURVE_WITH_KNOTS('',3,(#33760,#33761,#33762,#33763,#33764,
#33765,#33766,#33767,#33768,#33769,#33770,#33771,#33772,#33773,#33774,#33775,
#33776,#33777,#33778,#33779,#33780,#33781),.UNSPECIFIED.,.F.,.F.,(4,3,3,
3,3,3,3,4),(-10.3752088276281,-9.92769902200931,-8.93492911980838,-7.94215921760745,
-6.94938931540652,-5.95661941320559,-4.96384951100465,-4.09202352044855),
 .UNSPECIFIED.);
#2367=B_SPLINE_CURVE_WITH_KNOTS('',3,(#33782,#33783,#33784,#33785,#33786,
#33787,#33788,#33789,#33790,#33791,#33792,#33793,#33794,#33795,#33796,#33797,
#33798,#33799,#33800,#33801,#33802,#33803),.UNSPECIFIED.,.F.,.F.,(4,3,3,
3,3,3,3,4),(1.12274180646087,1.98700035221716,2.98050052832574,3.97400070443431,
4.96750088054289,5.96100105665147,6.95450123276005,7.40592711364046),
 .UNSPECIFIED.);
#2368=B_SPLINE_CURVE_WITH_KNOTS('',3,(#33808,#33809,#33810,#33811,#33812,
#33813,#33814,#33815,#33816,#33817,#33818,#33819,#33820,#33821,#33822,#33823,
#33824,#33825,#33826,#33827,#33828,#33829),.UNSPECIFIED.,.F.,.F.,(4,3,3,
3,3,3,3,4),(-16.6583941348077,-15.8843184352149,-14.891548533014,-13.898778630813,
-12.9060087286121,-11.9132388264112,-10.9204689242102,-10.3752088276281),
 .UNSPECIFIED.);
#2369=B_SPLINE_CURVE_WITH_KNOTS('',3,(#33830,#33831,#33832,#33833,#33834,
#33835,#33836,#33837,#33838,#33839,#33840,#33841,#33842,#33843,#33844,#33845,
#33846,#33847,#33848,#33849,#33850,#33851),.UNSPECIFIED.,.F.,.F.,(4,3,3,
3,3,3,3,4),(7.40592711364046,7.94800140886863,8.94150158497721,9.93500176108579,
10.9285019371944,11.922002113303,12.9155022894115,13.68911242082),
 .UNSPECIFIED.);
#2370=B_SPLINE_CURVE_WITH_KNOTS('',3,(#33856,#33857,#33858,#33859,#33860,
#33861,#33862,#33863,#33864,#33865,#33866,#33867,#33868,#33869,#33870,#33871,
#33872,#33873,#33874,#33875,#33876,#33877,#33878,#33879,#33880),
 .UNSPECIFIED.,.F.,.F.,(4,3,3,3,3,3,3,3,4),(-22.9415794419873,-22.8337077506214,
-21.8409378484205,-20.8481679462195,-19.8553980440186,-18.8626281418177,
-17.8698582396168,-16.8770883374158,-16.6583941348077),.UNSPECIFIED.);
#2371=B_SPLINE_CURVE_WITH_KNOTS('',3,(#33881,#33882,#33883,#33884,#33885,
#33886,#33887,#33888,#33889,#33890,#33891,#33892,#33893,#33894,#33895,#33896,
#33897,#33898,#33899,#33900,#33901,#33902,#33903,#33904,#33905),
 .UNSPECIFIED.,.F.,.F.,(4,3,3,3,3,3,3,3,4),(13.68911242082,13.9090024655201,
14.9025026416287,15.8960028177373,16.8895029938458,17.8830031699544,18.876503346063,
19.8700035221716,19.9722977279996),.UNSPECIFIED.);
#2372=B_SPLINE_CURVE_WITH_KNOTS('',3,(#33910,#33911,#33912,#33913,#33914,
#33915,#33916,#33917,#33918,#33919,#33920,#33921,#33922,#33923,#33924,#33925,
#33926,#33927,#33928,#33929,#33930,#33931),.UNSPECIFIED.,.F.,.F.,(4,3,3,
3,3,3,3,4),(-29.2247647491669,-28.790327163827,-27.7975572616261,-26.8047873594251,
-25.8120174572242,-24.8192475550233,-23.8264776528223,-22.9415794419873),
 .UNSPECIFIED.);
#2373=B_SPLINE_CURVE_WITH_KNOTS('',3,(#33932,#33933,#33934,#33935,#33936,
#33937,#33938,#33939,#33940,#33941,#33942,#33943,#33944,#33945,#33946,#33947,
#33948,#33949,#33950,#33951,#33952,#33953),.UNSPECIFIED.,.F.,.F.,(4,3,3,
3,3,3,3,4),(19.9722977279996,20.8635036982802,21.8570038743887,22.8505040504973,
23.8440042266059,24.8375044027145,25.8310045788231,26.2554830351792),
 .UNSPECIFIED.);
#2374=B_SPLINE_CURVE_WITH_KNOTS('',3,(#33958,#33959,#33960,#33961,#33962,
#33963,#33964,#33965,#33966,#33967,#33968,#33969,#33970,#33971,#33972,#33973,
#33974,#33975,#33976,#33977,#33978,#33979),.UNSPECIFIED.,.F.,.F.,(4,3,3,
3,3,3,3,4),(-35.5079500563465,-34.7469465770326,-33.7541766748316,-32.7614067726307,
-31.7686368704298,-30.7758669682288,-29.7830970660279,-29.2247647491669),
 .UNSPECIFIED.);
#2375=B_SPLINE_CURVE_WITH_KNOTS('',3,(#33980,#33981,#33982,#33983,#33984,
#33985,#33986,#33987,#33988,#33989,#33990,#33991,#33992,#33993,#33994,#33995,
#33996,#33997,#33998,#33999,#34000,#34001),.UNSPECIFIED.,.F.,.F.,(4,3,3,
3,3,3,3,4),(26.2554830351792,26.8245047549316,27.8180049310402,28.8115051071488,
29.8050052832574,30.798505459366,31.7920056354745,32.5386683423588),
 .UNSPECIFIED.);
#2376=B_SPLINE_CURVE_WITH_KNOTS('',3,(#34006,#34007,#34008,#34009,#34010,
#34011,#34012,#34013,#34014,#34015,#34016,#34017,#34018,#34019,#34020,#34021,
#34022,#34023,#34024,#34025,#34026,#34027,#34028,#34029,#34030),
 .UNSPECIFIED.,.F.,.F.,(4,3,3,3,3,3,3,3,4),(-41.7911353635261,-41.6963358924391,
-40.7035659902382,-39.7107960880372,-38.7180261858363,-37.7252562836354,
-36.7324863814344,-35.7397164792335,-35.5079500563465),.UNSPECIFIED.);
#2377=B_SPLINE_CURVE_WITH_KNOTS('',3,(#34031,#34032,#34033,#34034,#34035,
#34036,#34037,#34038,#34039,#34040,#34041,#34042,#34043,#34044,#34045,#34046,
#34047,#34048,#34049,#34050,#34051,#34052,#34053,#34054,#34055),
 .UNSPECIFIED.,.F.,.F.,(4,3,3,3,3,3,3,3,4),(32.5386683423588,32.7855058115831,
33.7790059876917,34.7725061638003,35.7660063399088,36.7595065160174,37.753006692126,
38.7465068682346,38.8218536495384),.UNSPECIFIED.);
#2378=B_SPLINE_CURVE_WITH_KNOTS('',3,(#34060,#34061,#34062,#34063,#34064,
#34065,#34066,#34067,#34068,#34069,#34070,#34071,#34072,#34073,#34074,#34075,
#34076,#34077,#34078,#34079,#34080,#34081),.UNSPECIFIED.,.F.,.F.,(4,3,3,
3,3,3,3,4),(-48.0743206707057,-47.6529553056447,-46.6601854034437,-45.6674155012428,
-44.6746455990419,-43.6818756968409,-42.68910579464,-41.7911353635261),
 .UNSPECIFIED.);
#2379=B_SPLINE_CURVE_WITH_KNOTS('',3,(#34082,#34083,#34084,#34085,#34086,
#34087,#34088,#34089,#34090,#34091,#34092,#34093,#34094,#34095,#34096,#34097,
#34098,#34099,#34100,#34101,#34102,#34103),.UNSPECIFIED.,.F.,.F.,(4,3,3,
3,3,3,3,4),(38.8218536495384,39.7400070443432,40.7335072204517,41.7270073965603,
42.7205075726689,43.7140077487775,44.7075079248861,45.105038956718),
 .UNSPECIFIED.);
#2380=B_SPLINE_CURVE_WITH_KNOTS('',3,(#34108,#34109,#34110,#34111,#34112,
#34113,#34114,#34115,#34116,#34117,#34118,#34119,#34120,#34121,#34122,#34123,
#34124,#34125,#34126,#34127,#34128,#34129),.UNSPECIFIED.,.F.,.F.,(4,3,3,
3,3,3,3,4),(-54.3575059778853,-53.6095747188503,-52.6168048166493,-51.6240349144484,
-50.6312650122475,-49.6384951100465,-48.6457252078456,-48.0743206707057),
 .UNSPECIFIED.);
#2381=B_SPLINE_CURVE_WITH_KNOTS('',3,(#34130,#34131,#34132,#34133,#34134,
#34135,#34136,#34137,#34138,#34139,#34140,#34141,#34142,#34143,#34144,#34145,
#34146,#34147,#34148,#34149,#34150,#34151),.UNSPECIFIED.,.F.,.F.,(4,3,3,
3,3,3,3,4),(45.105038956718,45.7010081009946,46.6945082771032,47.6880084532118,
48.6815086293204,49.675008805429,50.6685089815375,51.3882242638976),
 .UNSPECIFIED.);
#2382=B_SPLINE_CURVE_WITH_KNOTS('',3,(#34156,#34157,#34158,#34159,#34160,
#34161,#34162,#34163,#34164,#34165,#34166,#34167,#34168,#34169,#34170,#34171,
#34172,#34173,#34174,#34175,#34176,#34177,#34178,#34179,#34180),
 .UNSPECIFIED.,.F.,.F.,(4,3,3,3,3,3,3,3,4),(-60.6406912850649,-60.5589640342568,
-59.5661941320559,-58.5734242298549,-57.580654327654,-56.5878844254531,
-55.5951145232521,-54.6023446210512,-54.3575059778853),.UNSPECIFIED.);
#2383=B_SPLINE_CURVE_WITH_KNOTS('',3,(#34181,#34182,#34183,#34184,#34185,
#34186,#34187,#34188,#34189,#34190,#34191,#34192,#34193,#34194,#34195,#34196,
#34197,#34198,#34199,#34200,#34201,#34202,#34203,#34204,#34205),
 .UNSPECIFIED.,.F.,.F.,(4,3,3,3,3,3,3,3,4),(51.3882242638976,51.6620091576461,
52.6555093337547,53.6490095098633,54.6425096859719,55.6360098620804,56.629510038189,
57.6230102142976,57.6714095710772),.UNSPECIFIED.);
#2384=B_SPLINE_CURVE_WITH_KNOTS('',3,(#34210,#34211,#34212,#34213,#34214,
#34215,#34216,#34217,#34218,#34219,#34220,#34221,#34222,#34223,#34224,#34225,
#34226,#34227,#34228,#34229,#34230,#34231),.UNSPECIFIED.,.F.,.F.,(4,3,3,
3,3,3,3,4),(-66.9238765922445,-66.5155834474624,-65.5228135452614,-64.5300436430605,
-63.5372737408596,-62.5445038386586,-61.5517339364577,-60.6406912850649),
 .UNSPECIFIED.);
#2385=B_SPLINE_CURVE_WITH_KNOTS('',3,(#34232,#34233,#34234,#34235,#34236,
#34237,#34238,#34239,#34240,#34241,#34242,#34243,#34244,#34245,#34246,#34247,
#34248,#34249,#34250,#34251,#34252,#34253),.UNSPECIFIED.,.F.,.F.,(4,3,3,
3,3,3,3,4),(57.6714095710772,58.6165103904062,59.6100105665148,60.6035107426233,
61.5970109187319,62.5905110948405,63.5840112709491,63.9545948782568),
 .UNSPECIFIED.);
#2386=B_SPLINE_CURVE_WITH_KNOTS('',3,(#34258,#34259,#34260,#34261,#34262,
#34263,#34264,#34265,#34266,#34267,#34268,#34269,#34270,#34271,#34272,#34273,
#34274,#34275,#34276,#34277,#34278,#34279),.UNSPECIFIED.,.F.,.F.,(4,3,3,
3,3,3,3,4),(-73.207061899424,-72.4722028606679,-71.479432958467,-70.4866630562661,
-69.4938931540652,-68.5011232518642,-67.5083533496633,-66.9238765922445),
 .UNSPECIFIED.);
#2387=B_SPLINE_CURVE_WITH_KNOTS('',3,(#34280,#34281,#34282,#34283,#34284,
#34285,#34286,#34287,#34288,#34289,#34290,#34291,#34292,#34293,#34294,#34295,
#34296,#34297,#34298,#34299,#34300,#34301),.UNSPECIFIED.,.F.,.F.,(4,3,3,
3,3,3,3,4),(63.9545948782568,64.5775114470576,65.5710116231662,66.5645117992748,
67.5580119753834,68.551512151492,69.5450123276005,70.2377801854364),
 .UNSPECIFIED.);
#2388=B_SPLINE_CURVE_WITH_KNOTS('',3,(#34306,#34307,#34308,#34309,#34310,
#34311,#34312,#34313,#34314,#34315,#34316,#34317,#34318,#34319,#34320,#34321,
#34322,#34323,#34324,#34325,#34326,#34327,#34328,#34329,#34330),
 .UNSPECIFIED.,.F.,.F.,(4,3,3,3,3,3,3,3,4),(-79.4902472066036,-79.4215921760745,
-78.4288222738735,-77.4360523716726,-76.4432824694717,-75.4505125672707,
-74.4577426650698,-73.4649727628689,-73.207061899424),.UNSPECIFIED.);
#2389=B_SPLINE_CURVE_WITH_KNOTS('',3,(#34331,#34332,#34333,#34334,#34335,
#34336,#34337,#34338,#34339,#34340,#34341,#34342,#34343,#34344,#34345,#34346,
#34347,#34348,#34349,#34350,#34351,#34352,#34353,#34354,#34355),
 .UNSPECIFIED.,.F.,.F.,(4,3,3,3,3,3,3,3,4),(70.2377801854364,70.5385125037091,
71.5320126798177,72.5255128559263,73.5190130320348,74.5125132081434,75.506013384252,
76.4995135603606,76.520965492616),.UNSPECIFIED.);
#2390=B_SPLINE_CURVE_WITH_KNOTS('',3,(#34360,#34361,#34362,#34363,#34364,
#34365,#34366,#34367,#34368,#34369,#34370,#34371,#34372,#34373,#34374,#34375,
#34376,#34377,#34378,#34379,#34380,#34381),.UNSPECIFIED.,.F.,.F.,(4,3,3,
3,3,3,3,4),(-85.7734325137832,-85.3782115892801,-84.3854416870791,-83.3926717848782,
-82.3999018826773,-81.4071319804763,-80.4143620782754,-79.4902472066036),
 .UNSPECIFIED.);
#2391=B_SPLINE_CURVE_WITH_KNOTS('',3,(#34382,#34383,#34384,#34385,#34386,
#34387,#34388,#34389,#34390,#34391,#34392,#34393,#34394,#34395,#34396,#34397,
#34398,#34399,#34400,#34401,#34402,#34403),.UNSPECIFIED.,.F.,.F.,(4,3,3,
3,3,3,3,4),(76.520965492616,77.4930137364692,78.4865139125777,79.4800140886863,
80.4735142647949,81.4670144409035,82.4605146170121,82.8041507997956),
 .UNSPECIFIED.);
#2392=B_SPLINE_CURVE_WITH_KNOTS('',3,(#34408,#34409,#34410,#34411,#34412,
#34413,#34414,#34415,#34416,#34417,#34418,#34419,#34420,#34421,#34422,#34423,
#34424,#34425,#34426,#34427,#34428,#34429),.UNSPECIFIED.,.F.,.F.,(4,3,3,
3,3,3,3,4),(-92.0566178209628,-91.3348310024856,-90.3420611002847,-89.3492911980838,
-88.3565212958828,-87.3637513936819,-86.370981491481,-85.7734325137832),
 .UNSPECIFIED.);
#2393=B_SPLINE_CURVE_WITH_KNOTS('',3,(#34430,#34431,#34432,#34433,#34434,
#34435,#34436,#34437,#34438,#34439,#34440,#34441,#34442,#34443,#34444,#34445,
#34446,#34447,#34448,#34449,#34450,#34451),.UNSPECIFIED.,.F.,.F.,(4,3,3,
3,3,3,3,4),(82.8041507997956,83.4540147931206,84.4475149692292,85.4410151453378,
86.4345153214464,87.428015497555,88.4215156736635,89.0873361069751),
 .UNSPECIFIED.);
#2394=B_SPLINE_CURVE_WITH_KNOTS('',3,(#34456,#34457,#34458,#34459,#34460,
#34461,#34462,#34463,#34464,#34465,#34466,#34467,#34468,#34469,#34470,#34471,
#34472,#34473,#34474,#34475,#34476,#34477,#34478,#34479,#34480),
 .UNSPECIFIED.,.F.,.F.,(4,3,3,3,3,3,3,3,4),(-98.3398031281424,-98.2842203178921,
-97.2914504156912,-96.2986805134903,-95.3059106112893,-94.3131407090884,
-93.3203708068875,-92.3276009046866,-92.0566178209628),.UNSPECIFIED.);
#2395=B_SPLINE_CURVE_WITH_KNOTS('',3,(#34481,#34482,#34483,#34484,#34485,
#34486,#34487,#34488,#34489,#34490,#34491,#34492,#34493,#34494,#34495,#34496,
#34497,#34498,#34499,#34500,#34501,#34502),.UNSPECIFIED.,.F.,.F.,(4,3,3,
3,3,3,3,4),(89.0873361069751,89.4150158497721,90.4085160258807,91.4020162019893,
92.3955163780979,93.3890165542064,94.382516730315,95.3705214141547),
 .UNSPECIFIED.);
#2396=B_SPLINE_CURVE_WITH_KNOTS('',3,(#34507,#34508,#34509,#34510,#34511,
#34512,#34513,#34514,#34515,#34516,#34517,#34518,#34519,#34520,#34521,#34522,
#34523,#34524,#34525,#34526,#34527,#34528),.UNSPECIFIED.,.F.,.F.,(4,3,3,
3,3,3,3,4),(-104.622988435322,-104.240839731098,-103.248069828897,-102.255299926696,
-101.262530024495,-100.269760122294,-99.2769902200931,-98.3398031281424),
 .UNSPECIFIED.);
#2397=B_SPLINE_CURVE_WITH_KNOTS('',3,(#34529,#34530,#34531,#34532,#34533,
#34534,#34535,#34536,#34537,#34538,#34539,#34540,#34541,#34542,#34543,#34544,
#34545,#34546,#34547,#34548,#34549,#34550),.UNSPECIFIED.,.F.,.F.,(4,3,3,
3,3,3,3,4),(95.3705214141547,96.3695170825322,97.3630172586407,98.3565174347493,
99.3500176108579,100.343517786966,101.337017963075,101.653706721334),
 .UNSPECIFIED.);
#2398=B_SPLINE_CURVE_WITH_KNOTS('',3,(#34555,#34556,#34557,#34558,#34559,
#34560,#34561,#34562,#34563,#34564,#34565,#34566,#34567,#34568,#34569,#34570,
#34571,#34572,#34573,#34574,#34575,#34576),.UNSPECIFIED.,.F.,.F.,(4,3,3,
3,3,3,3,4),(-110.906173742502,-110.197459144303,-109.204689242102,-108.211919339901,
-107.219149437701,-106.2263795355,-105.233609633299,-104.622988435322),
 .UNSPECIFIED.);
#2399=B_SPLINE_CURVE_WITH_KNOTS('',3,(#34577,#34578,#34579,#34580,#34581,
#34582,#34583,#34584,#34585,#34586,#34587,#34588,#34589,#34590,#34591,#34592,
#34593,#34594,#34595,#34596,#34597,#34598),.UNSPECIFIED.,.F.,.F.,(4,3,3,
3,3,3,3,4),(101.653706721334,102.330518139184,103.324018315292,104.317518491401,
105.311018667509,106.304518843618,107.298019019727,107.936892028514),
 .UNSPECIFIED.);
#2400=B_SPLINE_CURVE_WITH_KNOTS('',3,(#34604,#34605,#34606,#34607,#34608,
#34609,#34610,#34611,#34612,#34613),.UNSPECIFIED.,.F.,.F.,(4,1,1,1,1,1,
1,4),(122.522113490002,122.806168794005,123.798938696205,124.791708598406,
125.784478500607,126.777248402808,127.770018305009,128.76278820721),
 .UNSPECIFIED.);
#2401=B_SPLINE_CURVE_WITH_KNOTS('',3,(#34616,#34617,#34618,#34619,#34620,
#34621,#34622,#34623,#34624),.UNSPECIFIED.,.F.,.F.,(4,1,1,1,1,1,4),(122.522113490002,
122.554556406795,123.548056582903,124.541556759012,125.535056935121,126.528557111229,
127.522057287338),.UNSPECIFIED.);
#2402=B_SPLINE_CURVE_WITH_KNOTS('',3,(#34629,#34630,#34631,#34632,#34633,
#34634,#34635,#34636,#34637,#34638),.UNSPECIFIED.,.F.,.F.,(4,1,1,1,1,1,
1,4),(116.238928182822,116.849549380799,117.842319283,118.835089185201,
119.827859087402,120.820628989603,121.813398891804,122.522113490002),
 .UNSPECIFIED.);
#2403=B_SPLINE_CURVE_WITH_KNOTS('',3,(#34639,#34640,#34641,#34642,#34643,
#34644,#34645,#34646,#34647,#34648),.UNSPECIFIED.,.F.,.F.,(4,1,1,1,1,1,
1,4),(116.238928182822,116.593555350143,117.587055526252,118.580555702361,
119.574055878469,120.567556054578,121.561056230686,122.522113490002),
 .UNSPECIFIED.);
#2404=B_SPLINE_CURVE_WITH_KNOTS('',3,(#34653,#34654,#34655,#34656,#34657,
#34658,#34659,#34660,#34661,#34662),.UNSPECIFIED.,.F.,.F.,(4,1,1,1,1,1,
1,4),(109.955742875643,110.892929967593,111.885699869794,112.878469771995,
113.871239674196,114.864009576397,115.856779478598,116.238928182822),
 .UNSPECIFIED.);
#2405=B_SPLINE_CURVE_WITH_KNOTS('',3,(#34663,#34664,#34665,#34666,#34667,
#34668,#34669,#34670,#34671,#34672),.UNSPECIFIED.,.F.,.F.,(4,1,1,1,1,1,
1,4),(109.955742875643,110.632554293492,111.626054469601,112.619554645709,
113.613054821818,114.606554997926,115.600055174035,116.238928182822),
 .UNSPECIFIED.);
#2406=B_SPLINE_CURVE_WITH_KNOTS('',3,(#34677,#34678,#34679,#34680,#34681,
#34682,#34683,#34684,#34685,#34686,#34687),.UNSPECIFIED.,.F.,.F.,(4,1,1,
1,1,1,1,1,4),(103.672557568463,103.943540652187,104.936310554388,105.929080456589,
106.92185035879,107.914620260991,108.907390163192,109.900160065392,109.955742875643),
 .UNSPECIFIED.);
#2407=B_SPLINE_CURVE_WITH_KNOTS('',3,(#34688,#34689,#34690,#34691,#34692,
#34693,#34694,#34695,#34696,#34697,#34698),.UNSPECIFIED.,.F.,.F.,(4,1,1,
1,1,1,1,1,4),(103.672557568463,103.678053060732,104.67155323684,105.665053412949,
106.658553589058,107.652053765166,108.645553941275,109.639054117383,109.955742875643),
 .UNSPECIFIED.);
#2408=B_SPLINE_CURVE_WITH_KNOTS('',3,(#34703,#34704,#34705,#34706,#34707,
#34708,#34709,#34710,#34711,#34712),.UNSPECIFIED.,.F.,.F.,(4,1,1,1,1,1,
1,4),(97.3893722612836,97.9869212389813,98.9796911411822,99.9724610433832,
100.965230945584,101.958000847785,102.950770749986,103.672557568463),
 .UNSPECIFIED.);
#2409=B_SPLINE_CURVE_WITH_KNOTS('',3,(#34713,#34714,#34715,#34716,#34717,
#34718,#34719,#34720,#34721,#34722),.UNSPECIFIED.,.F.,.F.,(4,1,1,1,1,1,
1,4),(97.3893722612835,97.7170520040804,98.710552180189,99.7040523562976,
100.697552532406,101.691052708515,102.684552884623,103.672557568463),
 .UNSPECIFIED.);
#2410=B_SPLINE_CURVE_WITH_KNOTS('',3,(#34727,#34728,#34729,#34730,#34731,
#34732,#34733,#34734,#34735,#34736),.UNSPECIFIED.,.F.,.F.,(4,1,1,1,1,1,
1,4),(91.106186954104,92.0303018257757,93.0230717279766,94.0158416301776,
95.0086115323785,96.0013814345794,96.9941513367804,97.3893722612836),
 .UNSPECIFIED.);
#2411=B_SPLINE_CURVE_WITH_KNOTS('',3,(#34737,#34738,#34739,#34740,#34741,
#34742,#34743,#34744,#34745,#34746),.UNSPECIFIED.,.F.,.F.,(4,1,1,1,1,1,
1,4),(91.106186954104,91.756050947429,92.7495511235375,93.7430512996461,
94.7365514757547,95.7300516518633,96.7235518279718,97.3893722612835),
 .UNSPECIFIED.);
#2412=B_SPLINE_CURVE_WITH_KNOTS('',3,(#34751,#34752,#34753,#34754,#34755,
#34756,#34757,#34758,#34759,#34760,#34761),.UNSPECIFIED.,.F.,.F.,(4,1,1,
1,1,1,1,1,4),(84.8230016469244,85.0809125103692,86.0736824125701,87.0664523147711,
88.059222216972,89.0519921191729,90.0447620213739,91.0375319235748,91.106186954104),
 .UNSPECIFIED.);
#2413=B_SPLINE_CURVE_WITH_KNOTS('',3,(#34762,#34763,#34764,#34765,#34766,
#34767,#34768,#34769,#34770,#34771),.UNSPECIFIED.,.F.,.F.,(4,1,1,1,1,1,
1,4),(84.8230016469244,85.7950498907775,86.7885500668861,87.7820502429946,
88.7755504191032,89.7690505952118,90.7625507713204,91.106186954104),
 .UNSPECIFIED.);
#2414=B_SPLINE_CURVE_WITH_KNOTS('',3,(#34776,#34777,#34778,#34779,#34780,
#34781,#34782,#34783,#34784,#34785),.UNSPECIFIED.,.F.,.F.,(4,1,1,1,1,1,
1,4),(78.5398163397448,79.1242930971636,80.1170629993645,81.1098329015655,
82.1026028037664,83.0953727059673,84.0881426081683,84.8230016469244),
 .UNSPECIFIED.);
#2415=B_SPLINE_CURVE_WITH_KNOTS('',3,(#34786,#34787,#34788,#34789,#34790,
#34791,#34792,#34793,#34794,#34795,#34796),.UNSPECIFIED.,.F.,.F.,(4,1,1,
1,1,1,1,1,4),(78.5398163397448,78.8405486580174,79.834048834126,80.8275490102346,
81.8210491863432,82.8145493624517,83.8080495385603,84.8015497146689,84.8230016469244),
 .UNSPECIFIED.);
#2416=B_SPLINE_CURVE_WITH_KNOTS('',3,(#34801,#34802,#34803,#34804,#34805,
#34806,#34807,#34808,#34809,#34810),.UNSPECIFIED.,.F.,.F.,(4,1,1,1,1,1,
1,4),(72.2566310325652,73.167673683958,74.160443586159,75.1532134883599,
76.1459833905608,77.1387532927618,78.1315231949627,78.5398163397448),
 .UNSPECIFIED.);
#2417=B_SPLINE_CURVE_WITH_KNOTS('',3,(#34811,#34812,#34813,#34814,#34815,
#34816,#34817,#34818,#34819,#34820),.UNSPECIFIED.,.F.,.F.,(4,1,1,1,1,1,
1,4),(72.2566310325652,72.879547601366,73.8730477774745,74.8665479535831,
75.8600481296917,76.8535483058003,77.8470484819088,78.5398163397448),
 .UNSPECIFIED.);
#2418=B_SPLINE_CURVE_WITH_KNOTS('',3,(#34825,#34826,#34827,#34828,#34829,
#34830,#34831,#34832,#34833,#34834,#34835),.UNSPECIFIED.,.F.,.F.,(4,1,1,
1,1,1,1,1,4),(65.9734457253856,66.2182843685515,67.2110542707524,68.2038241729534,
69.1965940751543,70.1893639773552,71.1821338795562,72.1749037817571,72.2566310325652),
 .UNSPECIFIED.);
#2419=B_SPLINE_CURVE_WITH_KNOTS('',3,(#34836,#34837,#34838,#34839,#34840,
#34841,#34842,#34843,#34844,#34845),.UNSPECIFIED.,.F.,.F.,(4,1,1,1,1,1,
1,4),(65.9734457253856,66.9185465447145,67.9120467208231,68.9055468969316,
69.8990470730402,70.8925472491488,71.8860474252574,72.2566310325652),
 .UNSPECIFIED.);
#2420=B_SPLINE_CURVE_WITH_KNOTS('',3,(#34850,#34851,#34852,#34853,#34854,
#34855,#34856,#34857,#34858,#34859),.UNSPECIFIED.,.F.,.F.,(4,1,1,1,1,1,
1,4),(59.690260418206,60.2616649553459,61.2544348575469,62.2472047597478,
63.2399746619487,64.2327445641497,65.2255144663506,65.9734457253856),
 .UNSPECIFIED.);
#2421=B_SPLINE_CURVE_WITH_KNOTS('',3,(#34860,#34861,#34862,#34863,#34864,
#34865,#34866,#34867,#34868,#34869,#34870),.UNSPECIFIED.,.F.,.F.,(4,1,1,
1,1,1,1,1,4),(59.690260418206,59.9640453119544,60.957545488063,61.9510456641716,
62.9445458402802,63.9380460163887,64.9315461924973,65.9250463686059,65.9734457253856),
 .UNSPECIFIED.);
#2422=B_SPLINE_CURVE_WITH_KNOTS('',3,(#34875,#34876,#34877,#34878,#34879,
#34880,#34881,#34882,#34883,#34884),.UNSPECIFIED.,.F.,.F.,(4,1,1,1,1,1,
1,4),(53.4070751110264,54.3050455421403,55.2978154443413,56.2905853465422,
57.2833552487431,58.2761251509441,59.268895053145,59.690260418206),
 .UNSPECIFIED.);
#2423=B_SPLINE_CURVE_WITH_KNOTS('',3,(#34885,#34886,#34887,#34888,#34889,
#34890,#34891,#34892,#34893,#34894),.UNSPECIFIED.,.F.,.F.,(4,1,1,1,1,1,
1,4),(53.4070751110264,54.003044255303,54.9965444314115,55.9900446075201,
56.9835447836287,57.9770449597373,58.9705451358458,59.690260418206),
 .UNSPECIFIED.);
#2424=B_SPLINE_CURVE_WITH_KNOTS('',3,(#34899,#34900,#34901,#34902,#34903,
#34904,#34905,#34906,#34907,#34908,#34909),.UNSPECIFIED.,.F.,.F.,(4,1,1,
1,1,1,1,1,4),(47.1238898038468,47.3556562267338,48.3484261289348,49.3411960311357,
50.3339659333366,51.3267358355376,52.3195057377385,53.3122756399394,53.4070751110264),
 .UNSPECIFIED.);
#2425=B_SPLINE_CURVE_WITH_KNOTS('',3,(#34910,#34911,#34912,#34913,#34914,
#34915,#34916,#34917,#34918,#34919),.UNSPECIFIED.,.F.,.F.,(4,1,1,1,1,1,
1,4),(47.1238898038468,48.0420431986515,49.0355433747601,50.0290435508686,
51.0225437269772,52.0160439030858,53.0095440791944,53.4070751110264),
 .UNSPECIFIED.);
#2426=B_SPLINE_CURVE_WITH_KNOTS('',3,(#34924,#34925,#34926,#34927,#34928,
#34929,#34930,#34931,#34932,#34933),.UNSPECIFIED.,.F.,.F.,(4,1,1,1,1,1,
1,4),(40.8407044966672,41.3990368135282,42.3918067157292,43.3845766179301,
44.377346520131,45.370116422332,46.3628863245329,47.1238898038468),
 .UNSPECIFIED.);
#2427=B_SPLINE_CURVE_WITH_KNOTS('',3,(#34934,#34935,#34936,#34937,#34938,
#34939,#34940,#34941,#34942,#34943,#34944),.UNSPECIFIED.,.F.,.F.,(4,1,1,
1,1,1,1,1,4),(40.8407044966672,41.0875419658914,42.081042142,43.0745423181086,
44.0680424942172,45.0615426703257,46.0550428464343,47.0485430225429,47.1238898038468),
 .UNSPECIFIED.);
#2428=B_SPLINE_CURVE_WITH_KNOTS('',3,(#34949,#34950,#34951,#34952,#34953,
#34954,#34955,#34956,#34957,#34958),.UNSPECIFIED.,.F.,.F.,(4,1,1,1,1,1,
1,4),(34.5575191894876,35.4424174003227,36.4351873025236,37.4279572047245,
38.4207271069255,39.4134970091264,40.4062669113273,40.8407044966672),
 .UNSPECIFIED.);
#2429=B_SPLINE_CURVE_WITH_KNOTS('',3,(#34959,#34960,#34961,#34962,#34963,
#34964,#34965,#34966,#34967,#34968),.UNSPECIFIED.,.F.,.F.,(4,1,1,1,1,1,
1,4),(34.5575191894876,35.1265409092399,36.1200410853485,37.1135412614571,
38.1070414375657,39.1005416136743,40.0940417897828,40.8407044966672),
 .UNSPECIFIED.);
#2430=B_SPLINE_CURVE_WITH_KNOTS('',3,(#34973,#34974,#34975,#34976,#34977,
#34978,#34979,#34980,#34981,#34982,#34983),.UNSPECIFIED.,.F.,.F.,(4,1,1,
1,1,1,1,1,4),(28.2743338823081,28.4930280849161,29.4857979871171,30.478567889318,
31.4713377915189,32.4641076937199,33.4568775959208,34.4496474981217,34.5575191894876),
 .UNSPECIFIED.);
#2431=B_SPLINE_CURVE_WITH_KNOTS('',3,(#34984,#34985,#34986,#34987,#34988,
#34989,#34990,#34991,#34992,#34993),.UNSPECIFIED.,.F.,.F.,(4,1,1,1,1,1,
1,4),(28.274333882308,29.1655398525885,30.1590400286971,31.1525402048056,
32.1460403809142,33.1395405570228,34.1330407331314,34.5575191894876),
 .UNSPECIFIED.);
#2432=B_SPLINE_CURVE_WITH_KNOTS('',3,(#34998,#34999,#35000,#35001,#35002,
#35003,#35004,#35005,#35006,#35007),.UNSPECIFIED.,.F.,.F.,(4,1,1,1,1,1,
1,4),(21.9911485751285,22.5364086717106,23.5291785739115,24.5219484761124,
25.5147183783134,26.5074882805143,27.5002581827152,28.2743338823081),
 .UNSPECIFIED.);
#2433=B_SPLINE_CURVE_WITH_KNOTS('',3,(#35008,#35009,#35010,#35011,#35012,
#35013,#35014,#35015,#35016,#35017,#35018),.UNSPECIFIED.,.F.,.F.,(4,1,1,
1,1,1,1,1,4),(21.9911485751284,22.2110386198284,23.204538795937,24.1980389720456,
25.1915391481542,26.1850393242627,27.1785395003713,28.1720396764799,28.274333882308),
 .UNSPECIFIED.);
#2434=B_SPLINE_CURVE_WITH_KNOTS('',3,(#35023,#35024,#35025,#35026,#35027,
#35028,#35029,#35030,#35031,#35032),.UNSPECIFIED.,.F.,.F.,(4,1,1,1,1,1,
1,4),(15.7079632679489,16.579789258505,17.5725591607059,18.5653290629068,
19.5580989651078,20.5508688673087,21.5436387695096,21.9911485751285),
 .UNSPECIFIED.);
#2435=B_SPLINE_CURVE_WITH_KNOTS('',3,(#35033,#35034,#35035,#35036,#35037,
#35038,#35039,#35040,#35041,#35042),.UNSPECIFIED.,.F.,.F.,(4,1,1,1,1,1,
1,4),(15.7079632679489,16.2500375631769,17.2435377392855,18.2370379153941,
19.2305380915027,20.2240382676113,21.2175384437198,21.9911485751284),
 .UNSPECIFIED.);
#2436=B_SPLINE_CURVE_WITH_KNOTS('',3,(#35045,#35046,#35047,#35048,#35049,
#35050,#35051,#35052,#35053,#35054,#35055,#35056,#35057,#35058,#35059,#35060,
#35061,#35062,#35063,#35064,#35065,#35066,#35067,#35068,#35069,#35070,#35071,
#35072,#35073,#35074,#35075,#35076,#35077,#35078,#35079,#35080,#35081,#35082,
#35083,#35084,#35085,#35086,#35087,#35088,#35089,#35090,#35091,#35092,#35093,
#35094,#35095,#35096,#35097,#35098,#35099,#35100,#35101,#35102,#35103,#35104,
#35105,#35106,#35107,#35108,#35109,#35110,#35111,#35112,#35113,#35114,#35115,
#35116,#35117,#35118,#35119,#35120,#35121,#35122,#35123,#35124,#35125,#35126,
#35127,#35128,#35129,#35130,#35131,#35132,#35133,#35134,#35135,#35136,#35137,
#35138,#35139,#35140,#35141,#35142,#35143,#35144,#35145,#35146,#35147,#35148,
#35149,#35150,#35151,#35152,#35153,#35154,#35155,#35156,#35157,#35158,#35159,
#35160,#35161,#35162,#35163,#35164,#35165),.UNSPECIFIED.,.F.,.F.,(4,3,3,
3,3,3,3,3,3,3,3,3,3,3,3,3,3,3,3,3,3,3,3,3,3,3,3,3,3,3,3,3,3,3,3,3,3,3,3,
3,4),(-0.753008129282273,-0.726411087083563,-0.715881786499564,-0.695023186638146,
-0.683336694953651,-0.673827840112005,-0.646303346018245,-0.632512441881234,
-0.6236006747729,-0.596001444533992,-0.585111150938268,-0.576118283133321,
-0.547602758918121,-0.536376015702489,-0.528202226180116,-0.507015336770619,
-0.486225152468931,-0.477897600046977,-0.452583818906367,-0.439178352550759,
-0.427196798483684,-0.40191963698411,-0.385160728199621,-0.376642475484535,
-0.347726720901875,-0.333286923643958,-0.323497787746622,-0.293375916145958,
-0.277554167376485,-0.267492310267894,-0.241337846280271,-0.224844604159538,
-0.216317003933383,-0.18753716728625,-0.170582917097926,-0.162078349438165,
-0.131638003391508,-0.115498895283149,-0.106874758104641,-0.101197657344851,
-0.0965360155478817),.UNSPECIFIED.);
#2437=B_SPLINE_CURVE_WITH_KNOTS('',3,(#35167,#35168,#35169,#35170,#35171,
#35172,#35173,#35174,#35175,#35176,#35177,#35178,#35179,#35180,#35181,#35182,
#35183,#35184,#35185,#35186,#35187,#35188,#35189,#35190,#35191,#35192,#35193,
#35194,#35195,#35196,#35197,#35198,#35199,#35200),.UNSPECIFIED.,.F.,.F.,
(4,3,3,3,3,3,3,3,3,3,3,4),(-0.204609524178367,-0.173916487069214,-0.152160152794692,
-0.142779925772755,-0.129154387771013,-0.104956417030493,-0.0922484622970884,
-0.0691863467228163,-0.0542893062834328,-0.041770965424307,-0.0153008738219011,
0.),.UNSPECIFIED.);
#2438=B_SPLINE_CURVE_WITH_KNOTS('',3,(#35203,#35204,#35205,#35206,#35207,
#35208,#35209,#35210,#35211,#35212,#35213,#35214,#35215,#35216,#35217,#35218),
 .UNSPECIFIED.,.F.,.F.,(4,3,3,3,3,4),(-0.0965360155478817,-0.0724020116609113,
-0.0590192863946756,-0.0503863222172558,-0.0186895043865902,0.),
 .UNSPECIFIED.);
#2439=B_SPLINE_CURVE_WITH_KNOTS('',3,(#35707,#35708,#35709,#35710,#35711,
#35712,#35713,#35714),.UNSPECIFIED.,.F.,.F.,(4,1,1,1,1,4),(11.6159397475003,
12.6087096497013,13.6014795519022,14.5942494541031,15.5870193563041,15.7079632679489),
 .UNSPECIFIED.);
#2440=B_SPLINE_CURVE_WITH_KNOTS('',3,(#35715,#35716,#35717,#35718,#35719,
#35720,#35721,#35722,#35723,#35724,#35725,#35726,#35727,#35728,#35729,#35730,
#35731,#35732,#35733,#35734,#35735,#35736,#35737,#35738,#35739,#35740,#35741,
#35742,#35743,#35744,#35745,#35746,#35747,#35748,#35749,#35750,#35751,#35752,
#35753,#35754,#35755,#35756,#35757,#35758,#35759,#35760,#35761,#35762,#35763,
#35764,#35765,#35766,#35767,#35768,#35769),.UNSPECIFIED.,.F.,.F.,(4,3,3,
3,3,3,3,3,3,3,3,3,3,3,3,3,3,3,4),(-0.275362278356885,-0.262570109468003,
-0.240166040204702,-0.228737803218204,-0.209304350143588,-0.199561001302199,
-0.189130684518224,-0.159734566166372,-0.148075950500899,-0.139790942517999,
-0.124720142759856,-0.107306928893897,-0.096279762610833,-0.086780292972213,
-0.0650852197291597,-0.0467838010330817,-0.0380963509139461,-0.011916188874275,
0.),.UNSPECIFIED.);
#2441=B_SPLINE_CURVE_WITH_KNOTS('',3,(#35770,#35771,#35772,#35773,#35774,
#35775,#35776,#35777,#35778,#35779,#35780,#35781,#35782,#35783,#35784,#35785,
#35786,#35787,#35788),.UNSPECIFIED.,.F.,.F.,(4,3,3,3,3,3,4),(-115.629180729976,
-115.161308655308,-114.168538753107,-113.175768850906,-112.182998948705,
-111.190229046504,-110.906173742502),.UNSPECIFIED.);
#2442=B_SPLINE_CURVE_WITH_KNOTS('',3,(#35791,#35792,#35793,#35794,#35795,
#35796,#35797,#35798,#35799),.UNSPECIFIED.,.F.,.F.,(4,1,1,1,1,1,4),(10.375208827628,
11.282536682634,12.2760368587426,13.2695370348512,14.2630372109598,15.2565373870684,
15.7079632679489),.UNSPECIFIED.);
#2443=B_SPLINE_CURVE_WITH_KNOTS('',3,(#36293,#36294,#36295,#36296,#36297,
#36298,#36299,#36300,#36301,#36302,#36303,#36304,#36305,#36306,#36307,#36308,
#36309,#36310,#36311,#36312,#36313,#36314),.UNSPECIFIED.,.F.,.F.,(4,3,3,
3,3,3,3,4),(107.936892028514,108.291519195835,109.285019371944,110.278519548052,
111.272019724161,112.265519900269,113.259020076378,113.556008056657),
 .UNSPECIFIED.);
#2444=B_SPLINE_CURVE_WITH_KNOTS('',3,(#36315,#36316,#36317,#36318,#36319,
#36320,#36321,#36322,#36323,#36324,#36325,#36326,#36327,#36328,#36329,#36330,
#36331,#36332,#36333,#36334,#36335,#36336,#36337,#36338,#36339,#36340,#36341,
#36342,#36343,#36344,#36345,#36346,#36347,#36348,#36349,#36350,#36351,#36352,
#36353,#36354,#36355,#36356,#36357,#36358,#36359,#36360,#36361,#36362,#36363,
#36364,#36365,#36366),.UNSPECIFIED.,.F.,.F.,(4,3,3,3,3,3,3,3,3,3,3,3,3,
3,3,3,3,4),(-0.276631791712727,-0.266310431017225,-0.251016700765444,-0.236970857216412,
-0.216553357237997,-0.204277578780747,-0.175779167785564,-0.164239042752865,
-0.155154932673123,-0.139868422463251,-0.120223860282124,-0.110723029685393,
-0.100734922391118,-0.0755511917933386,-0.0588149891352748,-0.049317539854096,
-0.0183008691858031,0.),.UNSPECIFIED.);
#2445=LINE('',#12705,#3019);
#2446=LINE('',#12740,#3020);
#2447=LINE('',#12767,#3021);
#2448=LINE('',#12818,#3022);
#2449=LINE('',#12866,#3023);
#2450=LINE('',#12914,#3024);
#2451=LINE('',#12965,#3025);
#2452=LINE('',#13013,#3026);
#2453=LINE('',#13061,#3027);
#2454=LINE('',#13112,#3028);
#2455=LINE('',#13163,#3029);
#2456=LINE('',#13211,#3030);
#2457=LINE('',#13262,#3031);
#2458=LINE('',#13301,#3032);
#2459=LINE('',#13323,#3033);
#2460=LINE('',#13347,#3034);
#2461=LINE('',#13372,#3035);
#2462=LINE('',#13397,#3036);
#2463=LINE('',#13421,#3037);
#2464=LINE('',#13446,#3038);
#2465=LINE('',#13470,#3039);
#2466=LINE('',#13495,#3040);
#2467=LINE('',#13519,#3041);
#2468=LINE('',#13544,#3042);
#2469=LINE('',#13569,#3043);
#2470=LINE('',#13593,#3044);
#2471=LINE('',#13610,#3045);
#2472=LINE('',#13645,#3046);
#2473=LINE('',#13672,#3047);
#2474=LINE('',#13723,#3048);
#2475=LINE('',#13771,#3049);
#2476=LINE('',#13819,#3050);
#2477=LINE('',#13870,#3051);
#2478=LINE('',#13918,#3052);
#2479=LINE('',#13966,#3053);
#2480=LINE('',#14017,#3054);
#2481=LINE('',#14068,#3055);
#2482=LINE('',#14116,#3056);
#2483=LINE('',#14167,#3057);
#2484=LINE('',#14206,#3058);
#2485=LINE('',#14228,#3059);
#2486=LINE('',#14252,#3060);
#2487=LINE('',#14277,#3061);
#2488=LINE('',#14302,#3062);
#2489=LINE('',#14326,#3063);
#2490=LINE('',#14351,#3064);
#2491=LINE('',#14375,#3065);
#2492=LINE('',#14400,#3066);
#2493=LINE('',#14424,#3067);
#2494=LINE('',#14449,#3068);
#2495=LINE('',#14474,#3069);
#2496=LINE('',#14498,#3070);
#2497=LINE('',#14515,#3071);
#2498=LINE('',#14550,#3072);
#2499=LINE('',#14577,#3073);
#2500=LINE('',#14628,#3074);
#2501=LINE('',#14676,#3075);
#2502=LINE('',#14724,#3076);
#2503=LINE('',#14775,#3077);
#2504=LINE('',#14823,#3078);
#2505=LINE('',#14871,#3079);
#2506=LINE('',#14922,#3080);
#2507=LINE('',#14973,#3081);
#2508=LINE('',#15021,#3082);
#2509=LINE('',#15072,#3083);
#2510=LINE('',#15111,#3084);
#2511=LINE('',#15133,#3085);
#2512=LINE('',#15157,#3086);
#2513=LINE('',#15182,#3087);
#2514=LINE('',#15207,#3088);
#2515=LINE('',#15231,#3089);
#2516=LINE('',#15256,#3090);
#2517=LINE('',#15280,#3091);
#2518=LINE('',#15305,#3092);
#2519=LINE('',#15329,#3093);
#2520=LINE('',#15354,#3094);
#2521=LINE('',#15379,#3095);
#2522=LINE('',#15403,#3096);
#2523=LINE('',#15420,#3097);
#2524=LINE('',#15455,#3098);
#2525=LINE('',#15482,#3099);
#2526=LINE('',#15533,#3100);
#2527=LINE('',#15581,#3101);
#2528=LINE('',#15629,#3102);
#2529=LINE('',#15680,#3103);
#2530=LINE('',#15728,#3104);
#2531=LINE('',#15776,#3105);
#2532=LINE('',#15827,#3106);
#2533=LINE('',#15878,#3107);
#2534=LINE('',#15926,#3108);
#2535=LINE('',#15977,#3109);
#2536=LINE('',#16016,#3110);
#2537=LINE('',#16038,#3111);
#2538=LINE('',#16062,#3112);
#2539=LINE('',#16087,#3113);
#2540=LINE('',#16112,#3114);
#2541=LINE('',#16136,#3115);
#2542=LINE('',#16161,#3116);
#2543=LINE('',#16185,#3117);
#2544=LINE('',#16210,#3118);
#2545=LINE('',#16234,#3119);
#2546=LINE('',#16259,#3120);
#2547=LINE('',#16284,#3121);
#2548=LINE('',#16308,#3122);
#2549=LINE('',#16327,#3123);
#2550=LINE('',#16330,#3124);
#2551=LINE('',#16333,#3125);
#2552=LINE('',#16335,#3126);
#2553=LINE('',#16336,#3127);
#2554=LINE('',#16341,#3128);
#2555=LINE('',#16345,#3129);
#2556=LINE('',#16347,#3130);
#2557=LINE('',#16348,#3131);
#2558=LINE('',#16354,#3132);
#2559=LINE('',#16357,#3133);
#2560=LINE('',#16359,#3134);
#2561=LINE('',#16361,#3135);
#2562=LINE('',#16371,#3136);
#2563=LINE('',#16372,#3137);
#2564=LINE('',#16380,#3138);
#2565=LINE('',#16389,#3139);
#2566=LINE('',#16391,#3140);
#2567=LINE('',#16400,#3141);
#2568=LINE('',#16402,#3142);
#2569=LINE('',#20303,#3143);
#2570=LINE('',#20309,#3144);
#2571=LINE('',#20314,#3145);
#2572=LINE('',#20316,#3146);
#2573=LINE('',#20318,#3147);
#2574=LINE('',#20319,#3148);
#2575=LINE('',#20322,#3149);
#2576=LINE('',#20324,#3150);
#2577=LINE('',#20325,#3151);
#2578=LINE('',#20328,#3152);
#2579=LINE('',#20330,#3153);
#2580=LINE('',#20331,#3154);
#2581=LINE('',#20333,#3155);
#2582=LINE('',#20337,#3156);
#2583=LINE('',#20339,#3157);
#2584=LINE('',#20341,#3158);
#2585=LINE('',#20342,#3159);
#2586=LINE('',#20346,#3160);
#2587=LINE('',#20348,#3161);
#2588=LINE('',#20350,#3162);
#2589=LINE('',#20351,#3163);
#2590=LINE('',#20353,#3164);
#2591=LINE('',#20354,#3165);
#2592=LINE('',#20356,#3166);
#2593=LINE('',#20361,#3167);
#2594=LINE('',#20366,#3168);
#2595=LINE('',#20369,#3169);
#2596=LINE('',#20374,#3170);
#2597=LINE('',#20376,#3171);
#2598=LINE('',#20378,#3172);
#2599=LINE('',#20379,#3173);
#2600=LINE('',#20381,#3174);
#2601=LINE('',#20383,#3175);
#2602=LINE('',#20385,#3176);
#2603=LINE('',#20386,#3177);
#2604=LINE('',#20389,#3178);
#2605=LINE('',#20391,#3179);
#2606=LINE('',#20392,#3180);
#2607=LINE('',#20394,#3181);
#2608=LINE('',#20395,#3182);
#2609=LINE('',#20396,#3183);
#2610=LINE('',#20404,#3184);
#2611=LINE('',#20410,#3185);
#2612=LINE('',#20416,#3186);
#2613=LINE('',#20422,#3187);
#2614=LINE('',#20428,#3188);
#2615=LINE('',#20433,#3189);
#2616=LINE('',#20435,#3190);
#2617=LINE('',#20437,#3191);
#2618=LINE('',#20438,#3192);
#2619=LINE('',#20441,#3193);
#2620=LINE('',#20443,#3194);
#2621=LINE('',#20444,#3195);
#2622=LINE('',#20447,#3196);
#2623=LINE('',#20449,#3197);
#2624=LINE('',#20450,#3198);
#2625=LINE('',#20452,#3199);
#2626=LINE('',#20453,#3200);
#2627=LINE('',#20464,#3201);
#2628=LINE('',#20472,#3202);
#2629=LINE('',#20476,#3203);
#2630=LINE('',#20482,#3204);
#2631=LINE('',#20503,#3205);
#2632=LINE('',#20554,#3206);
#2633=LINE('',#20605,#3207);
#2634=LINE('',#20653,#3208);
#2635=LINE('',#20704,#3209);
#2636=LINE('',#20755,#3210);
#2637=LINE('',#20803,#3211);
#2638=LINE('',#20842,#3212);
#2639=LINE('',#20863,#3213);
#2640=LINE('',#20914,#3214);
#2641=LINE('',#20965,#3215);
#2642=LINE('',#21013,#3216);
#2643=LINE('',#21064,#3217);
#2644=LINE('',#21115,#3218);
#2645=LINE('',#21163,#3219);
#2646=LINE('',#21202,#3220);
#2647=LINE('',#21226,#3221);
#2648=LINE('',#21250,#3222);
#2649=LINE('',#21275,#3223);
#2650=LINE('',#21300,#3224);
#2651=LINE('',#21324,#3225);
#2652=LINE('',#21349,#3226);
#2653=LINE('',#21374,#3227);
#2654=LINE('',#21391,#3228);
#2655=LINE('',#21415,#3229);
#2656=LINE('',#21439,#3230);
#2657=LINE('',#21464,#3231);
#2658=LINE('',#21489,#3232);
#2659=LINE('',#21513,#3233);
#2660=LINE('',#21538,#3234);
#2661=LINE('',#21563,#3235);
#2662=LINE('',#22304,#3236);
#2663=LINE('',#22306,#3237);
#2664=LINE('',#22308,#3238);
#2665=LINE('',#22310,#3239);
#2666=LINE('',#22311,#3240);
#2667=LINE('',#23040,#3241);
#2668=LINE('',#23046,#3242);
#2669=LINE('',#23051,#3243);
#2670=LINE('',#23053,#3244);
#2671=LINE('',#23055,#3245);
#2672=LINE('',#23056,#3246);
#2673=LINE('',#23059,#3247);
#2674=LINE('',#23061,#3248);
#2675=LINE('',#23062,#3249);
#2676=LINE('',#23065,#3250);
#2677=LINE('',#23067,#3251);
#2678=LINE('',#23069,#3252);
#2679=LINE('',#23071,#3253);
#2680=LINE('',#23073,#3254);
#2681=LINE('',#23075,#3255);
#2682=LINE('',#23076,#3256);
#2683=LINE('',#23079,#3257);
#2684=LINE('',#23080,#3258);
#2685=LINE('',#23083,#3259);
#2686=LINE('',#23084,#3260);
#2687=LINE('',#23087,#3261);
#2688=LINE('',#23088,#3262);
#2689=LINE('',#23093,#3263);
#2690=LINE('',#23094,#3264);
#2691=LINE('',#23099,#3265);
#2692=LINE('',#23100,#3266);
#2693=LINE('',#23103,#3267);
#2694=LINE('',#23104,#3268);
#2695=LINE('',#23109,#3269);
#2696=LINE('',#23111,#3270);
#2697=LINE('',#23112,#3271);
#2698=LINE('',#23115,#3272);
#2699=LINE('',#23117,#3273);
#2700=LINE('',#23118,#3274);
#2701=LINE('',#23120,#3275);
#2702=LINE('',#23123,#3276);
#2703=LINE('',#23125,#3277);
#2704=LINE('',#23126,#3278);
#2705=LINE('',#23128,#3279);
#2706=LINE('',#23133,#3280);
#2707=LINE('',#23141,#3281);
#2708=LINE('',#23147,#3282);
#2709=LINE('',#23152,#3283);
#2710=LINE('',#23154,#3284);
#2711=LINE('',#23156,#3285);
#2712=LINE('',#23157,#3286);
#2713=LINE('',#23160,#3287);
#2714=LINE('',#23162,#3288);
#2715=LINE('',#23163,#3289);
#2716=LINE('',#23166,#3290);
#2717=LINE('',#23168,#3291);
#2718=LINE('',#23169,#3292);
#2719=LINE('',#23171,#3293);
#2720=LINE('',#23172,#3294);
#2721=LINE('',#23180,#3295);
#2722=LINE('',#23185,#3296);
#2723=LINE('',#23192,#3297);
#2724=LINE('',#23199,#3298);
#2725=LINE('',#23203,#3299);
#2726=LINE('',#23205,#3300);
#2727=LINE('',#23210,#3301);
#2728=LINE('',#23245,#3302);
#2729=LINE('',#23272,#3303);
#2730=LINE('',#23323,#3304);
#2731=LINE('',#23371,#3305);
#2732=LINE('',#23419,#3306);
#2733=LINE('',#23470,#3307);
#2734=LINE('',#23518,#3308);
#2735=LINE('',#23566,#3309);
#2736=LINE('',#23617,#3310);
#2737=LINE('',#23668,#3311);
#2738=LINE('',#23716,#3312);
#2739=LINE('',#23767,#3313);
#2740=LINE('',#23806,#3314);
#2741=LINE('',#23828,#3315);
#2742=LINE('',#23852,#3316);
#2743=LINE('',#23877,#3317);
#2744=LINE('',#23902,#3318);
#2745=LINE('',#23926,#3319);
#2746=LINE('',#23951,#3320);
#2747=LINE('',#23975,#3321);
#2748=LINE('',#24000,#3322);
#2749=LINE('',#24024,#3323);
#2750=LINE('',#24049,#3324);
#2751=LINE('',#24074,#3325);
#2752=LINE('',#24098,#3326);
#2753=LINE('',#24115,#3327);
#2754=LINE('',#24124,#3328);
#2755=LINE('',#24141,#3329);
#2756=LINE('',#24192,#3330);
#2757=LINE('',#24243,#3331);
#2758=LINE('',#24291,#3332);
#2759=LINE('',#24342,#3333);
#2760=LINE('',#24393,#3334);
#2761=LINE('',#24441,#3335);
#2762=LINE('',#24492,#3336);
#2763=LINE('',#24543,#3337);
#2764=LINE('',#24591,#3338);
#2765=LINE('',#24642,#3339);
#2766=LINE('',#24693,#3340);
#2767=LINE('',#24741,#3341);
#2768=LINE('',#24792,#3342);
#2769=LINE('',#24843,#3343);
#2770=LINE('',#24891,#3344);
#2771=LINE('',#24942,#3345);
#2772=LINE('',#24981,#3346);
#2773=LINE('',#25005,#3347);
#2774=LINE('',#25029,#3348);
#2775=LINE('',#25054,#3349);
#2776=LINE('',#25079,#3350);
#2777=LINE('',#25103,#3351);
#2778=LINE('',#25128,#3352);
#2779=LINE('',#25153,#3353);
#2780=LINE('',#25177,#3354);
#2781=LINE('',#25202,#3355);
#2782=LINE('',#25227,#3356);
#2783=LINE('',#25251,#3357);
#2784=LINE('',#25276,#3358);
#2785=LINE('',#25301,#3359);
#2786=LINE('',#25325,#3360);
#2787=LINE('',#25350,#3361);
#2788=LINE('',#25375,#3362);
#2789=LINE('',#25399,#3363);
#2790=LINE('',#27619,#3364);
#2791=LINE('',#27621,#3365);
#2792=LINE('',#27623,#3366);
#2793=LINE('',#27624,#3367);
#2794=LINE('',#27627,#3368);
#2795=LINE('',#27629,#3369);
#2796=LINE('',#27630,#3370);
#2797=LINE('',#27633,#3371);
#2798=LINE('',#27635,#3372);
#2799=LINE('',#27636,#3373);
#2800=LINE('',#27638,#3374);
#2801=LINE('',#27639,#3375);
#2802=LINE('',#27646,#3376);
#2803=LINE('',#27655,#3377);
#2804=LINE('',#27672,#3378);
#2805=LINE('',#27723,#3379);
#2806=LINE('',#27774,#3380);
#2807=LINE('',#27822,#3381);
#2808=LINE('',#27870,#3382);
#2809=LINE('',#27921,#3383);
#2810=LINE('',#27972,#3384);
#2811=LINE('',#28020,#3385);
#2812=LINE('',#28071,#3386);
#2813=LINE('',#28110,#3387);
#2814=LINE('',#28134,#3388);
#2815=LINE('',#28158,#3389);
#2816=LINE('',#28183,#3390);
#2817=LINE('',#28207,#3391);
#2818=LINE('',#28232,#3392);
#2819=LINE('',#28256,#3393);
#2820=LINE('',#28281,#3394);
#2821=LINE('',#28306,#3395);
#2822=LINE('',#28330,#3396);
#2823=LINE('',#29169,#3397);
#2824=LINE('',#29174,#3398);
#2825=LINE('',#29176,#3399);
#2826=LINE('',#29178,#3400);
#2827=LINE('',#29179,#3401);
#2828=LINE('',#29183,#3402);
#2829=LINE('',#29184,#3403);
#2830=LINE('',#29185,#3404);
#2831=LINE('',#29188,#3405);
#2832=LINE('',#29190,#3406);
#2833=LINE('',#29192,#3407);
#2834=LINE('',#29193,#3408);
#2835=LINE('',#29196,#3409);
#2836=LINE('',#29197,#3410);
#2837=LINE('',#29200,#3411);
#2838=LINE('',#29202,#3412);
#2839=LINE('',#29203,#3413);
#2840=LINE('',#29205,#3414);
#2841=LINE('',#29206,#3415);
#2842=LINE('',#29214,#3416);
#2843=LINE('',#29219,#3417);
#2844=LINE('',#29221,#3418);
#2845=LINE('',#29223,#3419);
#2846=LINE('',#29224,#3420);
#2847=LINE('',#29227,#3421);
#2848=LINE('',#29229,#3422);
#2849=LINE('',#29230,#3423);
#2850=LINE('',#29233,#3424);
#2851=LINE('',#29235,#3425);
#2852=LINE('',#29236,#3426);
#2853=LINE('',#29238,#3427);
#2854=LINE('',#29239,#3428);
#2855=LINE('',#29247,#3429);
#2856=LINE('',#29253,#3430);
#2857=LINE('',#29262,#3431);
#2858=LINE('',#29273,#3432);
#2859=LINE('',#29281,#3433);
#2860=LINE('',#29285,#3434);
#2861=LINE('',#29291,#3435);
#2862=LINE('',#29293,#3436);
#2863=LINE('',#29295,#3437);
#2864=LINE('',#29296,#3438);
#2865=LINE('',#29300,#3439);
#2866=LINE('',#29302,#3440);
#2867=LINE('',#29304,#3441);
#2868=LINE('',#29305,#3442);
#2869=LINE('',#29645,#3443);
#2870=LINE('',#29651,#3444);
#2871=LINE('',#29659,#3445);
#2872=LINE('',#29683,#3446);
#2873=LINE('',#29731,#3447);
#2874=LINE('',#29779,#3448);
#2875=LINE('',#29827,#3449);
#2876=LINE('',#29875,#3450);
#2877=LINE('',#29923,#3451);
#2878=LINE('',#29971,#3452);
#2879=LINE('',#30025,#3453);
#2880=LINE('',#30073,#3454);
#2881=LINE('',#30121,#3455);
#2882=LINE('',#30175,#3456);
#2883=LINE('',#30223,#3457);
#2884=LINE('',#30271,#3458);
#2885=LINE('',#30319,#3459);
#2886=LINE('',#30370,#3460);
#2887=LINE('',#30418,#3461);
#2888=LINE('',#30440,#3462);
#2889=LINE('',#30464,#3463);
#2890=LINE('',#30488,#3464);
#2891=LINE('',#30514,#3465);
#2892=LINE('',#30538,#3466);
#2893=LINE('',#30562,#3467);
#2894=LINE('',#30587,#3468);
#2895=LINE('',#30612,#3469);
#2896=LINE('',#30636,#3470);
#2897=LINE('',#30661,#3471);
#2898=LINE('',#30686,#3472);
#2899=LINE('',#30710,#3473);
#2900=LINE('',#30734,#3474);
#2901=LINE('',#30759,#3475);
#2902=LINE('',#30784,#3476);
#2903=LINE('',#30988,#3477);
#2904=LINE('',#32010,#3478);
#2905=LINE('',#32012,#3479);
#2906=LINE('',#32014,#3480);
#2907=LINE('',#32015,#3481);
#2908=LINE('',#32018,#3482);
#2909=LINE('',#32020,#3483);
#2910=LINE('',#32021,#3484);
#2911=LINE('',#32024,#3485);
#2912=LINE('',#32026,#3486);
#2913=LINE('',#32027,#3487);
#2914=LINE('',#32030,#3488);
#2915=LINE('',#32032,#3489);
#2916=LINE('',#32033,#3490);
#2917=LINE('',#32036,#3491);
#2918=LINE('',#32038,#3492);
#2919=LINE('',#32039,#3493);
#2920=LINE('',#32041,#3494);
#2921=LINE('',#32042,#3495);
#2922=LINE('',#32049,#3496);
#2923=LINE('',#32057,#3497);
#2924=LINE('',#32081,#3498);
#2925=LINE('',#32129,#3499);
#2926=LINE('',#32177,#3500);
#2927=LINE('',#32225,#3501);
#2928=LINE('',#32279,#3502);
#2929=LINE('',#32327,#3503);
#2930=LINE('',#32375,#3504);
#2931=LINE('',#32429,#3505);
#2932=LINE('',#32477,#3506);
#2933=LINE('',#32525,#3507);
#2934=LINE('',#32551,#3508);
#2935=LINE('',#32575,#3509);
#2936=LINE('',#32599,#3510);
#2937=LINE('',#32624,#3511);
#2938=LINE('',#32649,#3512);
#2939=LINE('',#32673,#3513);
#2940=LINE('',#32698,#3514);
#2941=LINE('',#32723,#3515);
#2942=LINE('',#32747,#3516);
#2943=LINE('',#32951,#3517);
#2944=LINE('',#33688,#3518);
#2945=LINE('',#33690,#3519);
#2946=LINE('',#33692,#3520);
#2947=LINE('',#33693,#3521);
#2948=LINE('',#33696,#3522);
#2949=LINE('',#33698,#3523);
#2950=LINE('',#33699,#3524);
#2951=LINE('',#33702,#3525);
#2952=LINE('',#33704,#3526);
#2953=LINE('',#33705,#3527);
#2954=LINE('',#33708,#3528);
#2955=LINE('',#33710,#3529);
#2956=LINE('',#33711,#3530);
#2957=LINE('',#33714,#3531);
#2958=LINE('',#33716,#3532);
#2959=LINE('',#33717,#3533);
#2960=LINE('',#33719,#3534);
#2961=LINE('',#33720,#3535);
#2962=LINE('',#33727,#3536);
#2963=LINE('',#33735,#3537);
#2964=LINE('',#33759,#3538);
#2965=LINE('',#33807,#3539);
#2966=LINE('',#33855,#3540);
#2967=LINE('',#33909,#3541);
#2968=LINE('',#33957,#3542);
#2969=LINE('',#34005,#3543);
#2970=LINE('',#34059,#3544);
#2971=LINE('',#34107,#3545);
#2972=LINE('',#34155,#3546);
#2973=LINE('',#34209,#3547);
#2974=LINE('',#34257,#3548);
#2975=LINE('',#34305,#3549);
#2976=LINE('',#34359,#3550);
#2977=LINE('',#34407,#3551);
#2978=LINE('',#34455,#3552);
#2979=LINE('',#34506,#3553);
#2980=LINE('',#34554,#3554);
#2981=LINE('',#34602,#3555);
#2982=LINE('',#34628,#3556);
#2983=LINE('',#34652,#3557);
#2984=LINE('',#34676,#3558);
#2985=LINE('',#34702,#3559);
#2986=LINE('',#34726,#3560);
#2987=LINE('',#34750,#3561);
#2988=LINE('',#34775,#3562);
#2989=LINE('',#34800,#3563);
#2990=LINE('',#34824,#3564);
#2991=LINE('',#34849,#3565);
#2992=LINE('',#34874,#3566);
#2993=LINE('',#34898,#3567);
#2994=LINE('',#34923,#3568);
#2995=LINE('',#34948,#3569);
#2996=LINE('',#34972,#3570);
#2997=LINE('',#34997,#3571);
#2998=LINE('',#35022,#3572);
#2999=LINE('',#35220,#3573);
#3000=LINE('',#36371,#3574);
#3001=LINE('',#36373,#3575);
#3002=LINE('',#36375,#3576);
#3003=LINE('',#36376,#3577);
#3004=LINE('',#36379,#3578);
#3005=LINE('',#36381,#3579);
#3006=LINE('',#36382,#3580);
#3007=LINE('',#36385,#3581);
#3008=LINE('',#36387,#3582);
#3009=LINE('',#36388,#3583);
#3010=LINE('',#36391,#3584);
#3011=LINE('',#36393,#3585);
#3012=LINE('',#36394,#3586);
#3013=LINE('',#36397,#3587);
#3014=LINE('',#36399,#3588);
#3015=LINE('',#36400,#3589);
#3016=LINE('',#36402,#3590);
#3017=LINE('',#36403,#3591);
#3018=LINE('',#36410,#3592);
#3019=VECTOR('',#10696,0.2);
#3020=VECTOR('',#10699,0.2);
#3021=VECTOR('',#10704,0.2);
#3022=VECTOR('',#10707,0.2);
#3023=VECTOR('',#10710,0.2);
#3024=VECTOR('',#10713,0.2);
#3025=VECTOR('',#10716,0.2);
#3026=VECTOR('',#10719,0.2);
#3027=VECTOR('',#10722,0.2);
#3028=VECTOR('',#10725,0.2);
#3029=VECTOR('',#10728,0.2);
#3030=VECTOR('',#10731,0.2);
#3031=VECTOR('',#10734,0.2);
#3032=VECTOR('',#10739,0.205475);
#3033=VECTOR('',#10744,0.205475);
#3034=VECTOR('',#10747,0.205475);
#3035=VECTOR('',#10750,0.205475);
#3036=VECTOR('',#10753,0.205475);
#3037=VECTOR('',#10756,0.205475);
#3038=VECTOR('',#10759,0.205475);
#3039=VECTOR('',#10762,0.205475);
#3040=VECTOR('',#10765,0.205475);
#3041=VECTOR('',#10768,0.205475);
#3042=VECTOR('',#10771,0.205475);
#3043=VECTOR('',#10774,0.205475);
#3044=VECTOR('',#10777,0.205475);
#3045=VECTOR('',#10782,0.2);
#3046=VECTOR('',#10785,0.2);
#3047=VECTOR('',#10790,0.2);
#3048=VECTOR('',#10793,0.2);
#3049=VECTOR('',#10796,0.2);
#3050=VECTOR('',#10799,0.2);
#3051=VECTOR('',#10802,0.2);
#3052=VECTOR('',#10805,0.2);
#3053=VECTOR('',#10808,0.2);
#3054=VECTOR('',#10811,0.2);
#3055=VECTOR('',#10814,0.2);
#3056=VECTOR('',#10817,0.2);
#3057=VECTOR('',#10820,0.2);
#3058=VECTOR('',#10825,0.205475000000001);
#3059=VECTOR('',#10830,0.205475000000001);
#3060=VECTOR('',#10833,0.205475000000001);
#3061=VECTOR('',#10836,0.205475000000001);
#3062=VECTOR('',#10839,0.205475000000001);
#3063=VECTOR('',#10842,0.205475000000001);
#3064=VECTOR('',#10845,0.205475000000001);
#3065=VECTOR('',#10848,0.205475000000001);
#3066=VECTOR('',#10851,0.205475000000001);
#3067=VECTOR('',#10854,0.205475000000001);
#3068=VECTOR('',#10857,0.205475000000001);
#3069=VECTOR('',#10860,0.205475000000001);
#3070=VECTOR('',#10863,0.205475000000001);
#3071=VECTOR('',#10868,0.2);
#3072=VECTOR('',#10871,0.2);
#3073=VECTOR('',#10876,0.2);
#3074=VECTOR('',#10879,0.2);
#3075=VECTOR('',#10882,0.2);
#3076=VECTOR('',#10885,0.2);
#3077=VECTOR('',#10888,0.2);
#3078=VECTOR('',#10891,0.2);
#3079=VECTOR('',#10894,0.2);
#3080=VECTOR('',#10897,0.2);
#3081=VECTOR('',#10900,0.2);
#3082=VECTOR('',#10903,0.2);
#3083=VECTOR('',#10906,0.2);
#3084=VECTOR('',#10911,0.205475000000001);
#3085=VECTOR('',#10916,0.205475000000001);
#3086=VECTOR('',#10919,0.205475000000001);
#3087=VECTOR('',#10922,0.205475000000001);
#3088=VECTOR('',#10925,0.205475000000001);
#3089=VECTOR('',#10928,0.205475000000001);
#3090=VECTOR('',#10931,0.205475000000001);
#3091=VECTOR('',#10934,0.205475000000001);
#3092=VECTOR('',#10937,0.205475000000001);
#3093=VECTOR('',#10940,0.205475000000001);
#3094=VECTOR('',#10943,0.205475000000001);
#3095=VECTOR('',#10946,0.205475000000001);
#3096=VECTOR('',#10949,0.205475000000001);
#3097=VECTOR('',#10954,0.2);
#3098=VECTOR('',#10957,0.2);
#3099=VECTOR('',#10962,0.2);
#3100=VECTOR('',#10965,0.2);
#3101=VECTOR('',#10968,0.2);
#3102=VECTOR('',#10971,0.2);
#3103=VECTOR('',#10974,0.2);
#3104=VECTOR('',#10977,0.2);
#3105=VECTOR('',#10980,0.2);
#3106=VECTOR('',#10983,0.2);
#3107=VECTOR('',#10986,0.2);
#3108=VECTOR('',#10989,0.2);
#3109=VECTOR('',#10992,0.2);
#3110=VECTOR('',#10997,0.205475);
#3111=VECTOR('',#11002,0.205475);
#3112=VECTOR('',#11005,0.205475);
#3113=VECTOR('',#11008,0.205475);
#3114=VECTOR('',#11011,0.205475);
#3115=VECTOR('',#11014,0.205475);
#3116=VECTOR('',#11017,0.205475);
#3117=VECTOR('',#11020,0.205475);
#3118=VECTOR('',#11023,0.205475);
#3119=VECTOR('',#11026,0.205475);
#3120=VECTOR('',#11029,0.205475);
#3121=VECTOR('',#11032,0.205475);
#3122=VECTOR('',#11035,0.205475);
#3123=VECTOR('',#11042,1.);
#3124=VECTOR('',#11045,1.);
#3125=VECTOR('',#11048,1.);
#3126=VECTOR('',#11049,1.);
#3127=VECTOR('',#11050,1.);
#3128=VECTOR('',#11055,1.);
#3129=VECTOR('',#11060,1.);
#3130=VECTOR('',#11061,1.);
#3131=VECTOR('',#11062,1.);
#3132=VECTOR('',#11067,1.);
#3133=VECTOR('',#11070,1.);
#3134=VECTOR('',#11073,1.);
#3135=VECTOR('',#11074,1.);
#3136=VECTOR('',#11085,1.);
#3137=VECTOR('',#11086,1.);
#3138=VECTOR('',#11097,0.6);
#3139=VECTOR('',#11108,0.4);
#3140=VECTOR('',#11111,0.25);
#3141=VECTOR('',#11122,0.4);
#3142=VECTOR('',#11125,0.25);
#3143=VECTOR('',#11162,0.3);
#3144=VECTOR('',#11169,0.3);
#3145=VECTOR('',#11174,1.);
#3146=VECTOR('',#11175,1.);
#3147=VECTOR('',#11176,1.);
#3148=VECTOR('',#11177,1.);
#3149=VECTOR('',#11180,1.);
#3150=VECTOR('',#11181,1.);
#3151=VECTOR('',#11182,1.);
#3152=VECTOR('',#11185,1.);
#3153=VECTOR('',#11186,1.);
#3154=VECTOR('',#11187,1.);
#3155=VECTOR('',#11190,1.);
#3156=VECTOR('',#11193,1.);
#3157=VECTOR('',#11194,1.);
#3158=VECTOR('',#11195,1.);
#3159=VECTOR('',#11196,1.);
#3160=VECTOR('',#11199,1.);
#3161=VECTOR('',#11200,1.);
#3162=VECTOR('',#11201,1.);
#3163=VECTOR('',#11202,1.);
#3164=VECTOR('',#11205,1.);
#3165=VECTOR('',#11206,1.);
#3166=VECTOR('',#11209,1.);
#3167=VECTOR('',#11214,0.65);
#3168=VECTOR('',#11221,0.8);
#3169=VECTOR('',#11226,1.);
#3170=VECTOR('',#11231,1.);
#3171=VECTOR('',#11232,1.);
#3172=VECTOR('',#11233,1.);
#3173=VECTOR('',#11234,1.);
#3174=VECTOR('',#11237,1.);
#3175=VECTOR('',#11238,1.);
#3176=VECTOR('',#11239,1.);
#3177=VECTOR('',#11240,1.);
#3178=VECTOR('',#11243,1.);
#3179=VECTOR('',#11244,1.);
#3180=VECTOR('',#11245,1.);
#3181=VECTOR('',#11248,1.);
#3182=VECTOR('',#11249,1.);
#3183=VECTOR('',#11250,1.);
#3184=VECTOR('',#11261,0.25);
#3185=VECTOR('',#11268,0.25);
#3186=VECTOR('',#11275,0.25);
#3187=VECTOR('',#11282,0.25);
#3188=VECTOR('',#11289,0.6);
#3189=VECTOR('',#11294,1.);
#3190=VECTOR('',#11295,1.);
#3191=VECTOR('',#11296,1.);
#3192=VECTOR('',#11297,1.);
#3193=VECTOR('',#11300,1.);
#3194=VECTOR('',#11301,1.);
#3195=VECTOR('',#11302,1.);
#3196=VECTOR('',#11305,1.);
#3197=VECTOR('',#11306,1.);
#3198=VECTOR('',#11307,1.);
#3199=VECTOR('',#11310,1.);
#3200=VECTOR('',#11311,1.);
#3201=VECTOR('',#11326,0.8);
#3202=VECTOR('',#11337,0.4);
#3203=VECTOR('',#11342,0.6);
#3204=VECTOR('',#11349,0.15);
#3205=VECTOR('',#11354,0.15);
#3206=VECTOR('',#11357,0.15);
#3207=VECTOR('',#11360,0.15);
#3208=VECTOR('',#11363,0.15);
#3209=VECTOR('',#11366,0.15);
#3210=VECTOR('',#11369,0.15);
#3211=VECTOR('',#11372,0.15);
#3212=VECTOR('',#11377,0.15);
#3213=VECTOR('',#11382,0.15);
#3214=VECTOR('',#11385,0.15);
#3215=VECTOR('',#11388,0.15);
#3216=VECTOR('',#11391,0.15);
#3217=VECTOR('',#11394,0.15);
#3218=VECTOR('',#11397,0.15);
#3219=VECTOR('',#11400,0.15);
#3220=VECTOR('',#11405,0.1543);
#3221=VECTOR('',#11410,0.1543);
#3222=VECTOR('',#11413,0.1543);
#3223=VECTOR('',#11416,0.1543);
#3224=VECTOR('',#11419,0.1543);
#3225=VECTOR('',#11422,0.1543);
#3226=VECTOR('',#11425,0.1543);
#3227=VECTOR('',#11428,0.1543);
#3228=VECTOR('',#11433,0.1543);
#3229=VECTOR('',#11438,0.1543);
#3230=VECTOR('',#11441,0.1543);
#3231=VECTOR('',#11444,0.1543);
#3232=VECTOR('',#11447,0.1543);
#3233=VECTOR('',#11450,0.1543);
#3234=VECTOR('',#11453,0.1543);
#3235=VECTOR('',#11456,0.1543);
#3236=VECTOR('',#11465,1.);
#3237=VECTOR('',#11466,1.);
#3238=VECTOR('',#11467,1.);
#3239=VECTOR('',#11468,1.);
#3240=VECTOR('',#11469,1.);
#3241=VECTOR('',#11480,0.2);
#3242=VECTOR('',#11487,0.2);
#3243=VECTOR('',#11492,1.);
#3244=VECTOR('',#11493,1.);
#3245=VECTOR('',#11494,1.);
#3246=VECTOR('',#11495,1.);
#3247=VECTOR('',#11498,1.);
#3248=VECTOR('',#11499,1.);
#3249=VECTOR('',#11500,1.);
#3250=VECTOR('',#11503,1.);
#3251=VECTOR('',#11504,1.);
#3252=VECTOR('',#11505,1.);
#3253=VECTOR('',#11506,1.);
#3254=VECTOR('',#11507,1.);
#3255=VECTOR('',#11508,1.);
#3256=VECTOR('',#11509,1.);
#3257=VECTOR('',#11512,1.);
#3258=VECTOR('',#11513,1.);
#3259=VECTOR('',#11516,1.);
#3260=VECTOR('',#11517,1.);
#3261=VECTOR('',#11520,1.);
#3262=VECTOR('',#11521,1.);
#3263=VECTOR('',#11526,1.);
#3264=VECTOR('',#11527,1.);
#3265=VECTOR('',#11532,1.);
#3266=VECTOR('',#11533,1.);
#3267=VECTOR('',#11538,1.);
#3268=VECTOR('',#11539,1.);
#3269=VECTOR('',#11546,1.);
#3270=VECTOR('',#11547,1.);
#3271=VECTOR('',#11548,1.);
#3272=VECTOR('',#11551,1.);
#3273=VECTOR('',#11552,1.);
#3274=VECTOR('',#11553,1.);
#3275=VECTOR('',#11556,1.);
#3276=VECTOR('',#11559,1.);
#3277=VECTOR('',#11560,1.);
#3278=VECTOR('',#11561,1.);
#3279=VECTOR('',#11564,1.);
#3280=VECTOR('',#11571,0.6);
#3281=VECTOR('',#11582,0.2);
#3282=VECTOR('',#11589,0.2);
#3283=VECTOR('',#11594,1.);
#3284=VECTOR('',#11595,1.);
#3285=VECTOR('',#11596,1.);
#3286=VECTOR('',#11597,1.);
#3287=VECTOR('',#11600,1.);
#3288=VECTOR('',#11601,1.);
#3289=VECTOR('',#11602,1.);
#3290=VECTOR('',#11605,1.);
#3291=VECTOR('',#11606,1.);
#3292=VECTOR('',#11607,1.);
#3293=VECTOR('',#11610,1.);
#3294=VECTOR('',#11611,1.);
#3295=VECTOR('',#11622,0.65);
#3296=VECTOR('',#11629,0.7);
#3297=VECTOR('',#11638,0.65);
#3298=VECTOR('',#11647,0.35);
#3299=VECTOR('',#11652,0.3);
#3300=VECTOR('',#11655,0.35);
#3301=VECTOR('',#11660,0.2);
#3302=VECTOR('',#11663,0.2);
#3303=VECTOR('',#11668,0.2);
#3304=VECTOR('',#11671,0.2);
#3305=VECTOR('',#11674,0.2);
#3306=VECTOR('',#11677,0.2);
#3307=VECTOR('',#11680,0.2);
#3308=VECTOR('',#11683,0.2);
#3309=VECTOR('',#11686,0.2);
#3310=VECTOR('',#11689,0.2);
#3311=VECTOR('',#11692,0.2);
#3312=VECTOR('',#11695,0.2);
#3313=VECTOR('',#11698,0.2);
#3314=VECTOR('',#11703,0.205475);
#3315=VECTOR('',#11708,0.205475);
#3316=VECTOR('',#11711,0.205475);
#3317=VECTOR('',#11714,0.205475);
#3318=VECTOR('',#11717,0.205475);
#3319=VECTOR('',#11720,0.205475);
#3320=VECTOR('',#11723,0.205475);
#3321=VECTOR('',#11726,0.205475);
#3322=VECTOR('',#11729,0.205475);
#3323=VECTOR('',#11732,0.205475);
#3324=VECTOR('',#11735,0.205475);
#3325=VECTOR('',#11738,0.205475);
#3326=VECTOR('',#11741,0.205475);
#3327=VECTOR('',#11746,0.15);
#3328=VECTOR('',#11749,0.15);
#3329=VECTOR('',#11756,0.15);
#3330=VECTOR('',#11759,0.15);
#3331=VECTOR('',#11762,0.15);
#3332=VECTOR('',#11765,0.15);
#3333=VECTOR('',#11768,0.15);
#3334=VECTOR('',#11771,0.15);
#3335=VECTOR('',#11774,0.15);
#3336=VECTOR('',#11777,0.15);
#3337=VECTOR('',#11780,0.15);
#3338=VECTOR('',#11783,0.15);
#3339=VECTOR('',#11786,0.15);
#3340=VECTOR('',#11789,0.15);
#3341=VECTOR('',#11792,0.15);
#3342=VECTOR('',#11795,0.15);
#3343=VECTOR('',#11798,0.15);
#3344=VECTOR('',#11801,0.15);
#3345=VECTOR('',#11804,0.15);
#3346=VECTOR('',#11809,0.1543);
#3347=VECTOR('',#11814,0.1543);
#3348=VECTOR('',#11817,0.1543);
#3349=VECTOR('',#11820,0.1543);
#3350=VECTOR('',#11823,0.1543);
#3351=VECTOR('',#11826,0.1543);
#3352=VECTOR('',#11829,0.1543);
#3353=VECTOR('',#11832,0.1543);
#3354=VECTOR('',#11835,0.1543);
#3355=VECTOR('',#11838,0.1543);
#3356=VECTOR('',#11841,0.1543);
#3357=VECTOR('',#11844,0.1543);
#3358=VECTOR('',#11847,0.1543);
#3359=VECTOR('',#11850,0.1543);
#3360=VECTOR('',#11853,0.1543);
#3361=VECTOR('',#11856,0.1543);
#3362=VECTOR('',#11859,0.1543);
#3363=VECTOR('',#11862,0.1543);
#3364=VECTOR('',#11883,1.);
#3365=VECTOR('',#11884,1.);
#3366=VECTOR('',#11885,1.);
#3367=VECTOR('',#11886,1.);
#3368=VECTOR('',#11889,1.);
#3369=VECTOR('',#11890,1.);
#3370=VECTOR('',#11891,1.);
#3371=VECTOR('',#11894,1.);
#3372=VECTOR('',#11895,1.);
#3373=VECTOR('',#11896,1.);
#3374=VECTOR('',#11899,1.);
#3375=VECTOR('',#11900,1.);
#3376=VECTOR('',#11909,0.15);
#3377=VECTOR('',#11912,0.15);
#3378=VECTOR('',#11919,0.15);
#3379=VECTOR('',#11922,0.15);
#3380=VECTOR('',#11925,0.15);
#3381=VECTOR('',#11928,0.15);
#3382=VECTOR('',#11931,0.15);
#3383=VECTOR('',#11934,0.15);
#3384=VECTOR('',#11937,0.15);
#3385=VECTOR('',#11940,0.15);
#3386=VECTOR('',#11943,0.15);
#3387=VECTOR('',#11948,0.1543);
#3388=VECTOR('',#11953,0.1543);
#3389=VECTOR('',#11956,0.1543);
#3390=VECTOR('',#11959,0.1543);
#3391=VECTOR('',#11962,0.1543);
#3392=VECTOR('',#11965,0.1543);
#3393=VECTOR('',#11968,0.1543);
#3394=VECTOR('',#11971,0.1543);
#3395=VECTOR('',#11974,0.1543);
#3396=VECTOR('',#11977,0.1543);
#3397=VECTOR('',#11992,0.2);
#3398=VECTOR('',#11997,1.);
#3399=VECTOR('',#11998,1.);
#3400=VECTOR('',#11999,1.);
#3401=VECTOR('',#12000,1.);
#3402=VECTOR('',#12003,1.);
#3403=VECTOR('',#12004,1.);
#3404=VECTOR('',#12005,1.);
#3405=VECTOR('',#12008,1.);
#3406=VECTOR('',#12009,1.);
#3407=VECTOR('',#12010,1.);
#3408=VECTOR('',#12011,1.);
#3409=VECTOR('',#12014,1.);
#3410=VECTOR('',#12015,1.);
#3411=VECTOR('',#12018,1.);
#3412=VECTOR('',#12019,1.);
#3413=VECTOR('',#12020,1.);
#3414=VECTOR('',#12023,1.);
#3415=VECTOR('',#12024,1.);
#3416=VECTOR('',#12035,0.2);
#3417=VECTOR('',#12040,1.);
#3418=VECTOR('',#12041,1.);
#3419=VECTOR('',#12042,1.);
#3420=VECTOR('',#12043,1.);
#3421=VECTOR('',#12046,1.);
#3422=VECTOR('',#12047,1.);
#3423=VECTOR('',#12048,1.);
#3424=VECTOR('',#12051,1.);
#3425=VECTOR('',#12052,1.);
#3426=VECTOR('',#12053,1.);
#3427=VECTOR('',#12056,1.);
#3428=VECTOR('',#12057,1.);
#3429=VECTOR('',#12068,0.2);
#3430=VECTOR('',#12075,0.3);
#3431=VECTOR('',#12088,0.15);
#3432=VECTOR('',#12103,0.2);
#3433=VECTOR('',#12112,0.4);
#3434=VECTOR('',#12119,0.2);
#3435=VECTOR('',#12126,1.);
#3436=VECTOR('',#12127,1.);
#3437=VECTOR('',#12128,1.);
#3438=VECTOR('',#12129,1.);
#3439=VECTOR('',#12132,1.);
#3440=VECTOR('',#12133,1.);
#3441=VECTOR('',#12134,1.);
#3442=VECTOR('',#12135,1.);
#3443=VECTOR('',#12168,0.2);
#3444=VECTOR('',#12175,0.4);
#3445=VECTOR('',#12186,0.2);
#3446=VECTOR('',#12191,0.2);
#3447=VECTOR('',#12194,0.2);
#3448=VECTOR('',#12197,0.2);
#3449=VECTOR('',#12200,0.2);
#3450=VECTOR('',#12203,0.2);
#3451=VECTOR('',#12206,0.2);
#3452=VECTOR('',#12209,0.2);
#3453=VECTOR('',#12212,0.2);
#3454=VECTOR('',#12215,0.2);
#3455=VECTOR('',#12218,0.2);
#3456=VECTOR('',#12221,0.2);
#3457=VECTOR('',#12224,0.2);
#3458=VECTOR('',#12227,0.2);
#3459=VECTOR('',#12230,0.2);
#3460=VECTOR('',#12233,0.2);
#3461=VECTOR('',#12236,0.15555);
#3462=VECTOR('',#12241,0.15555);
#3463=VECTOR('',#12244,0.15555);
#3464=VECTOR('',#12247,0.15555);
#3465=VECTOR('',#12250,0.15555);
#3466=VECTOR('',#12253,0.15555);
#3467=VECTOR('',#12256,0.15555);
#3468=VECTOR('',#12259,0.15555);
#3469=VECTOR('',#12262,0.15555);
#3470=VECTOR('',#12265,0.15555);
#3471=VECTOR('',#12268,0.15555);
#3472=VECTOR('',#12271,0.15555);
#3473=VECTOR('',#12274,0.15555);
#3474=VECTOR('',#12277,0.15555);
#3475=VECTOR('',#12280,0.15555);
#3476=VECTOR('',#12283,0.15555);
#3477=VECTOR('',#12288,0.15);
#3478=VECTOR('',#12299,1.);
#3479=VECTOR('',#12300,1.);
#3480=VECTOR('',#12301,1.);
#3481=VECTOR('',#12302,1.);
#3482=VECTOR('',#12305,1.);
#3483=VECTOR('',#12306,1.);
#3484=VECTOR('',#12307,1.);
#3485=VECTOR('',#12310,1.);
#3486=VECTOR('',#12311,1.);
#3487=VECTOR('',#12312,1.);
#3488=VECTOR('',#12315,1.);
#3489=VECTOR('',#12316,1.);
#3490=VECTOR('',#12317,1.);
#3491=VECTOR('',#12320,1.);
#3492=VECTOR('',#12321,1.);
#3493=VECTOR('',#12322,1.);
#3494=VECTOR('',#12325,1.);
#3495=VECTOR('',#12326,1.);
#3496=VECTOR('',#12335,0.35);
#3497=VECTOR('',#12346,0.15);
#3498=VECTOR('',#12351,0.15);
#3499=VECTOR('',#12354,0.15);
#3500=VECTOR('',#12357,0.15);
#3501=VECTOR('',#12360,0.15);
#3502=VECTOR('',#12363,0.15);
#3503=VECTOR('',#12366,0.15);
#3504=VECTOR('',#12369,0.15);
#3505=VECTOR('',#12372,0.15);
#3506=VECTOR('',#12375,0.15);
#3507=VECTOR('',#12378,0.117775);
#3508=VECTOR('',#12383,0.117775);
#3509=VECTOR('',#12386,0.117775);
#3510=VECTOR('',#12389,0.117775);
#3511=VECTOR('',#12392,0.117775);
#3512=VECTOR('',#12395,0.117775);
#3513=VECTOR('',#12398,0.117775);
#3514=VECTOR('',#12401,0.117775);
#3515=VECTOR('',#12404,0.117775);
#3516=VECTOR('',#12407,0.117775);
#3517=VECTOR('',#12412,0.1);
#3518=VECTOR('',#12423,1.);
#3519=VECTOR('',#12424,1.);
#3520=VECTOR('',#12425,1.);
#3521=VECTOR('',#12426,1.);
#3522=VECTOR('',#12429,1.);
#3523=VECTOR('',#12430,1.);
#3524=VECTOR('',#12431,1.);
#3525=VECTOR('',#12434,1.);
#3526=VECTOR('',#12435,1.);
#3527=VECTOR('',#12436,1.);
#3528=VECTOR('',#12439,1.);
#3529=VECTOR('',#12440,1.);
#3530=VECTOR('',#12441,1.);
#3531=VECTOR('',#12444,1.);
#3532=VECTOR('',#12445,1.);
#3533=VECTOR('',#12446,1.);
#3534=VECTOR('',#12449,1.);
#3535=VECTOR('',#12450,1.);
#3536=VECTOR('',#12459,0.3);
#3537=VECTOR('',#12470,0.15);
#3538=VECTOR('',#12475,0.15);
#3539=VECTOR('',#12478,0.15);
#3540=VECTOR('',#12481,0.15);
#3541=VECTOR('',#12484,0.15);
#3542=VECTOR('',#12487,0.15);
#3543=VECTOR('',#12490,0.15);
#3544=VECTOR('',#12493,0.15);
#3545=VECTOR('',#12496,0.15);
#3546=VECTOR('',#12499,0.15);
#3547=VECTOR('',#12502,0.15);
#3548=VECTOR('',#12505,0.15);
#3549=VECTOR('',#12508,0.15);
#3550=VECTOR('',#12511,0.15);
#3551=VECTOR('',#12514,0.15);
#3552=VECTOR('',#12517,0.15);
#3553=VECTOR('',#12520,0.15);
#3554=VECTOR('',#12523,0.15);
#3555=VECTOR('',#12526,0.117775);
#3556=VECTOR('',#12531,0.117775);
#3557=VECTOR('',#12534,0.117775);
#3558=VECTOR('',#12537,0.117775);
#3559=VECTOR('',#12540,0.117775);
#3560=VECTOR('',#12543,0.117775);
#3561=VECTOR('',#12546,0.117775);
#3562=VECTOR('',#12549,0.117775);
#3563=VECTOR('',#12552,0.117775);
#3564=VECTOR('',#12555,0.117775);
#3565=VECTOR('',#12558,0.117775);
#3566=VECTOR('',#12561,0.117775);
#3567=VECTOR('',#12564,0.117775);
#3568=VECTOR('',#12567,0.117775);
#3569=VECTOR('',#12570,0.117775);
#3570=VECTOR('',#12573,0.117775);
#3571=VECTOR('',#12576,0.117775);
#3572=VECTOR('',#12579,0.117775);
#3573=VECTOR('',#12584,0.1);
#3574=VECTOR('',#12595,1.);
#3575=VECTOR('',#12596,1.);
#3576=VECTOR('',#12597,1.);
#3577=VECTOR('',#12598,1.);
#3578=VECTOR('',#12601,1.);
#3579=VECTOR('',#12602,1.);
#3580=VECTOR('',#12603,1.);
#3581=VECTOR('',#12606,1.);
#3582=VECTOR('',#12607,1.);
#3583=VECTOR('',#12608,1.);
#3584=VECTOR('',#12611,1.);
#3585=VECTOR('',#12612,1.);
#3586=VECTOR('',#12613,1.);
#3587=VECTOR('',#12616,1.);
#3588=VECTOR('',#12617,1.);
#3589=VECTOR('',#12618,1.);
#3590=VECTOR('',#12621,1.);
#3591=VECTOR('',#12622,1.);
#3592=VECTOR('',#12631,0.3);
#3593=VERTEX_POINT('',#12703);
#3594=VERTEX_POINT('',#12704);
#3595=VERTEX_POINT('',#12706);
#3596=VERTEX_POINT('',#12729);
#3597=VERTEX_POINT('',#12731);
#3598=VERTEX_POINT('',#12739);
#3599=VERTEX_POINT('',#12765);
#3600=VERTEX_POINT('',#12766);
#3601=VERTEX_POINT('',#12816);
#3602=VERTEX_POINT('',#12817);
#3603=VERTEX_POINT('',#12864);
#3604=VERTEX_POINT('',#12865);
#3605=VERTEX_POINT('',#12912);
#3606=VERTEX_POINT('',#12913);
#3607=VERTEX_POINT('',#12963);
#3608=VERTEX_POINT('',#12964);
#3609=VERTEX_POINT('',#13011);
#3610=VERTEX_POINT('',#13012);
#3611=VERTEX_POINT('',#13059);
#3612=VERTEX_POINT('',#13060);
#3613=VERTEX_POINT('',#13110);
#3614=VERTEX_POINT('',#13111);
#3615=VERTEX_POINT('',#13161);
#3616=VERTEX_POINT('',#13162);
#3617=VERTEX_POINT('',#13209);
#3618=VERTEX_POINT('',#13210);
#3619=VERTEX_POINT('',#13260);
#3620=VERTEX_POINT('',#13261);
#3621=VERTEX_POINT('',#13263);
#3622=VERTEX_POINT('',#13277);
#3623=VERTEX_POINT('',#13299);
#3624=VERTEX_POINT('',#13300);
#3625=VERTEX_POINT('',#13302);
#3626=VERTEX_POINT('',#13310);
#3627=VERTEX_POINT('',#13321);
#3628=VERTEX_POINT('',#13322);
#3629=VERTEX_POINT('',#13345);
#3630=VERTEX_POINT('',#13346);
#3631=VERTEX_POINT('',#13370);
#3632=VERTEX_POINT('',#13371);
#3633=VERTEX_POINT('',#13395);
#3634=VERTEX_POINT('',#13396);
#3635=VERTEX_POINT('',#13419);
#3636=VERTEX_POINT('',#13420);
#3637=VERTEX_POINT('',#13444);
#3638=VERTEX_POINT('',#13445);
#3639=VERTEX_POINT('',#13468);
#3640=VERTEX_POINT('',#13469);
#3641=VERTEX_POINT('',#13493);
#3642=VERTEX_POINT('',#13494);
#3643=VERTEX_POINT('',#13517);
#3644=VERTEX_POINT('',#13518);
#3645=VERTEX_POINT('',#13542);
#3646=VERTEX_POINT('',#13543);
#3647=VERTEX_POINT('',#13567);
#3648=VERTEX_POINT('',#13568);
#3649=VERTEX_POINT('',#13591);
#3650=VERTEX_POINT('',#13592);
#3651=VERTEX_POINT('',#13594);
#3652=VERTEX_POINT('',#13600);
#3653=VERTEX_POINT('',#13608);
#3654=VERTEX_POINT('',#13609);
#3655=VERTEX_POINT('',#13611);
#3656=VERTEX_POINT('',#13634);
#3657=VERTEX_POINT('',#13636);
#3658=VERTEX_POINT('',#13644);
#3659=VERTEX_POINT('',#13670);
#3660=VERTEX_POINT('',#13671);
#3661=VERTEX_POINT('',#13721);
#3662=VERTEX_POINT('',#13722);
#3663=VERTEX_POINT('',#13769);
#3664=VERTEX_POINT('',#13770);
#3665=VERTEX_POINT('',#13817);
#3666=VERTEX_POINT('',#13818);
#3667=VERTEX_POINT('',#13868);
#3668=VERTEX_POINT('',#13869);
#3669=VERTEX_POINT('',#13916);
#3670=VERTEX_POINT('',#13917);
#3671=VERTEX_POINT('',#13964);
#3672=VERTEX_POINT('',#13965);
#3673=VERTEX_POINT('',#14015);
#3674=VERTEX_POINT('',#14016);
#3675=VERTEX_POINT('',#14066);
#3676=VERTEX_POINT('',#14067);
#3677=VERTEX_POINT('',#14114);
#3678=VERTEX_POINT('',#14115);
#3679=VERTEX_POINT('',#14165);
#3680=VERTEX_POINT('',#14166);
#3681=VERTEX_POINT('',#14168);
#3682=VERTEX_POINT('',#14182);
#3683=VERTEX_POINT('',#14204);
#3684=VERTEX_POINT('',#14205);
#3685=VERTEX_POINT('',#14207);
#3686=VERTEX_POINT('',#14215);
#3687=VERTEX_POINT('',#14226);
#3688=VERTEX_POINT('',#14227);
#3689=VERTEX_POINT('',#14250);
#3690=VERTEX_POINT('',#14251);
#3691=VERTEX_POINT('',#14275);
#3692=VERTEX_POINT('',#14276);
#3693=VERTEX_POINT('',#14300);
#3694=VERTEX_POINT('',#14301);
#3695=VERTEX_POINT('',#14324);
#3696=VERTEX_POINT('',#14325);
#3697=VERTEX_POINT('',#14349);
#3698=VERTEX_POINT('',#14350);
#3699=VERTEX_POINT('',#14373);
#3700=VERTEX_POINT('',#14374);
#3701=VERTEX_POINT('',#14398);
#3702=VERTEX_POINT('',#14399);
#3703=VERTEX_POINT('',#14422);
#3704=VERTEX_POINT('',#14423);
#3705=VERTEX_POINT('',#14447);
#3706=VERTEX_POINT('',#14448);
#3707=VERTEX_POINT('',#14472);
#3708=VERTEX_POINT('',#14473);
#3709=VERTEX_POINT('',#14496);
#3710=VERTEX_POINT('',#14497);
#3711=VERTEX_POINT('',#14499);
#3712=VERTEX_POINT('',#14505);
#3713=VERTEX_POINT('',#14513);
#3714=VERTEX_POINT('',#14514);
#3715=VERTEX_POINT('',#14516);
#3716=VERTEX_POINT('',#14539);
#3717=VERTEX_POINT('',#14541);
#3718=VERTEX_POINT('',#14549);
#3719=VERTEX_POINT('',#14575);
#3720=VERTEX_POINT('',#14576);
#3721=VERTEX_POINT('',#14626);
#3722=VERTEX_POINT('',#14627);
#3723=VERTEX_POINT('',#14674);
#3724=VERTEX_POINT('',#14675);
#3725=VERTEX_POINT('',#14722);
#3726=VERTEX_POINT('',#14723);
#3727=VERTEX_POINT('',#14773);
#3728=VERTEX_POINT('',#14774);
#3729=VERTEX_POINT('',#14821);
#3730=VERTEX_POINT('',#14822);
#3731=VERTEX_POINT('',#14869);
#3732=VERTEX_POINT('',#14870);
#3733=VERTEX_POINT('',#14920);
#3734=VERTEX_POINT('',#14921);
#3735=VERTEX_POINT('',#14971);
#3736=VERTEX_POINT('',#14972);
#3737=VERTEX_POINT('',#15019);
#3738=VERTEX_POINT('',#15020);
#3739=VERTEX_POINT('',#15070);
#3740=VERTEX_POINT('',#15071);
#3741=VERTEX_POINT('',#15073);
#3742=VERTEX_POINT('',#15087);
#3743=VERTEX_POINT('',#15109);
#3744=VERTEX_POINT('',#15110);
#3745=VERTEX_POINT('',#15112);
#3746=VERTEX_POINT('',#15120);
#3747=VERTEX_POINT('',#15131);
#3748=VERTEX_POINT('',#15132);
#3749=VERTEX_POINT('',#15155);
#3750=VERTEX_POINT('',#15156);
#3751=VERTEX_POINT('',#15180);
#3752=VERTEX_POINT('',#15181);
#3753=VERTEX_POINT('',#15205);
#3754=VERTEX_POINT('',#15206);
#3755=VERTEX_POINT('',#15229);
#3756=VERTEX_POINT('',#15230);
#3757=VERTEX_POINT('',#15254);
#3758=VERTEX_POINT('',#15255);
#3759=VERTEX_POINT('',#15278);
#3760=VERTEX_POINT('',#15279);
#3761=VERTEX_POINT('',#15303);
#3762=VERTEX_POINT('',#15304);
#3763=VERTEX_POINT('',#15327);
#3764=VERTEX_POINT('',#15328);
#3765=VERTEX_POINT('',#15352);
#3766=VERTEX_POINT('',#15353);
#3767=VERTEX_POINT('',#15377);
#3768=VERTEX_POINT('',#15378);
#3769=VERTEX_POINT('',#15401);
#3770=VERTEX_POINT('',#15402);
#3771=VERTEX_POINT('',#15404);
#3772=VERTEX_POINT('',#15410);
#3773=VERTEX_POINT('',#15418);
#3774=VERTEX_POINT('',#15419);
#3775=VERTEX_POINT('',#15421);
#3776=VERTEX_POINT('',#15444);
#3777=VERTEX_POINT('',#15446);
#3778=VERTEX_POINT('',#15454);
#3779=VERTEX_POINT('',#15480);
#3780=VERTEX_POINT('',#15481);
#3781=VERTEX_POINT('',#15531);
#3782=VERTEX_POINT('',#15532);
#3783=VERTEX_POINT('',#15579);
#3784=VERTEX_POINT('',#15580);
#3785=VERTEX_POINT('',#15627);
#3786=VERTEX_POINT('',#15628);
#3787=VERTEX_POINT('',#15678);
#3788=VERTEX_POINT('',#15679);
#3789=VERTEX_POINT('',#15726);
#3790=VERTEX_POINT('',#15727);
#3791=VERTEX_POINT('',#15774);
#3792=VERTEX_POINT('',#15775);
#3793=VERTEX_POINT('',#15825);
#3794=VERTEX_POINT('',#15826);
#3795=VERTEX_POINT('',#15876);
#3796=VERTEX_POINT('',#15877);
#3797=VERTEX_POINT('',#15924);
#3798=VERTEX_POINT('',#15925);
#3799=VERTEX_POINT('',#15975);
#3800=VERTEX_POINT('',#15976);
#3801=VERTEX_POINT('',#15978);
#3802=VERTEX_POINT('',#15992);
#3803=VERTEX_POINT('',#16014);
#3804=VERTEX_POINT('',#16015);
#3805=VERTEX_POINT('',#16017);
#3806=VERTEX_POINT('',#16025);
#3807=VERTEX_POINT('',#16036);
#3808=VERTEX_POINT('',#16037);
#3809=VERTEX_POINT('',#16060);
#3810=VERTEX_POINT('',#16061);
#3811=VERTEX_POINT('',#16085);
#3812=VERTEX_POINT('',#16086);
#3813=VERTEX_POINT('',#16110);
#3814=VERTEX_POINT('',#16111);
#3815=VERTEX_POINT('',#16134);
#3816=VERTEX_POINT('',#16135);
#3817=VERTEX_POINT('',#16159);
#3818=VERTEX_POINT('',#16160);
#3819=VERTEX_POINT('',#16183);
#3820=VERTEX_POINT('',#16184);
#3821=VERTEX_POINT('',#16208);
#3822=VERTEX_POINT('',#16209);
#3823=VERTEX_POINT('',#16232);
#3824=VERTEX_POINT('',#16233);
#3825=VERTEX_POINT('',#16257);
#3826=VERTEX_POINT('',#16258);
#3827=VERTEX_POINT('',#16282);
#3828=VERTEX_POINT('',#16283);
#3829=VERTEX_POINT('',#16306);
#3830=VERTEX_POINT('',#16307);
#3831=VERTEX_POINT('',#16309);
#3832=VERTEX_POINT('',#16315);
#3833=VERTEX_POINT('',#16323);
#3834=VERTEX_POINT('',#16324);
#3835=VERTEX_POINT('',#16326);
#3836=VERTEX_POINT('',#16328);
#3837=VERTEX_POINT('',#16332);
#3838=VERTEX_POINT('',#16334);
#3839=VERTEX_POINT('',#16338);
#3840=VERTEX_POINT('',#16340);
#3841=VERTEX_POINT('',#16344);
#3842=VERTEX_POINT('',#16346);
#3843=VERTEX_POINT('',#16350);
#3844=VERTEX_POINT('',#16351);
#3845=VERTEX_POINT('',#16353);
#3846=VERTEX_POINT('',#16355);
#3847=VERTEX_POINT('',#16360);
#3848=VERTEX_POINT('',#16363);
#3849=VERTEX_POINT('',#16365);
#3850=VERTEX_POINT('',#16367);
#3851=VERTEX_POINT('',#16370);
#3852=VERTEX_POINT('',#16373);
#3853=VERTEX_POINT('',#16378);
#3854=VERTEX_POINT('',#16382);
#3855=VERTEX_POINT('',#16384);
#3856=VERTEX_POINT('',#16387);
#3857=VERTEX_POINT('',#16393);
#3858=VERTEX_POINT('',#16395);
#3859=VERTEX_POINT('',#16398);
#3860=VERTEX_POINT('',#20300);
#3861=VERTEX_POINT('',#20302);
#3862=VERTEX_POINT('',#20306);
#3863=VERTEX_POINT('',#20308);
#3864=VERTEX_POINT('',#20312);
#3865=VERTEX_POINT('',#20313);
#3866=VERTEX_POINT('',#20315);
#3867=VERTEX_POINT('',#20317);
#3868=VERTEX_POINT('',#20321);
#3869=VERTEX_POINT('',#20323);
#3870=VERTEX_POINT('',#20327);
#3871=VERTEX_POINT('',#20329);
#3872=VERTEX_POINT('',#20335);
#3873=VERTEX_POINT('',#20336);
#3874=VERTEX_POINT('',#20338);
#3875=VERTEX_POINT('',#20340);
#3876=VERTEX_POINT('',#20344);
#3877=VERTEX_POINT('',#20345);
#3878=VERTEX_POINT('',#20347);
#3879=VERTEX_POINT('',#20349);
#3880=VERTEX_POINT('',#20358);
#3881=VERTEX_POINT('',#20360);
#3882=VERTEX_POINT('',#20364);
#3883=VERTEX_POINT('',#20372);
#3884=VERTEX_POINT('',#20373);
#3885=VERTEX_POINT('',#20375);
#3886=VERTEX_POINT('',#20377);
#3887=VERTEX_POINT('',#20382);
#3888=VERTEX_POINT('',#20384);
#3889=VERTEX_POINT('',#20388);
#3890=VERTEX_POINT('',#20390);
#3891=VERTEX_POINT('',#20401);
#3892=VERTEX_POINT('',#20403);
#3893=VERTEX_POINT('',#20407);
#3894=VERTEX_POINT('',#20409);
#3895=VERTEX_POINT('',#20413);
#3896=VERTEX_POINT('',#20415);
#3897=VERTEX_POINT('',#20419);
#3898=VERTEX_POINT('',#20421);
#3899=VERTEX_POINT('',#20425);
#3900=VERTEX_POINT('',#20427);
#3901=VERTEX_POINT('',#20431);
#3902=VERTEX_POINT('',#20432);
#3903=VERTEX_POINT('',#20434);
#3904=VERTEX_POINT('',#20436);
#3905=VERTEX_POINT('',#20440);
#3906=VERTEX_POINT('',#20442);
#3907=VERTEX_POINT('',#20446);
#3908=VERTEX_POINT('',#20448);
#3909=VERTEX_POINT('',#20458);
#3910=VERTEX_POINT('',#20460);
#3911=VERTEX_POINT('',#20463);
#3912=VERTEX_POINT('',#20467);
#3913=VERTEX_POINT('',#20470);
#3914=VERTEX_POINT('',#20474);
#3915=VERTEX_POINT('',#20480);
#3916=VERTEX_POINT('',#20481);
#3917=VERTEX_POINT('',#20483);
#3918=VERTEX_POINT('',#20488);
#3919=VERTEX_POINT('',#20501);
#3920=VERTEX_POINT('',#20502);
#3921=VERTEX_POINT('',#20552);
#3922=VERTEX_POINT('',#20553);
#3923=VERTEX_POINT('',#20603);
#3924=VERTEX_POINT('',#20604);
#3925=VERTEX_POINT('',#20651);
#3926=VERTEX_POINT('',#20652);
#3927=VERTEX_POINT('',#20702);
#3928=VERTEX_POINT('',#20703);
#3929=VERTEX_POINT('',#20753);
#3930=VERTEX_POINT('',#20754);
#3931=VERTEX_POINT('',#20801);
#3932=VERTEX_POINT('',#20802);
#3933=VERTEX_POINT('',#20804);
#3934=VERTEX_POINT('',#20818);
#3935=VERTEX_POINT('',#20840);
#3936=VERTEX_POINT('',#20841);
#3937=VERTEX_POINT('',#20843);
#3938=VERTEX_POINT('',#20848);
#3939=VERTEX_POINT('',#20861);
#3940=VERTEX_POINT('',#20862);
#3941=VERTEX_POINT('',#20912);
#3942=VERTEX_POINT('',#20913);
#3943=VERTEX_POINT('',#20963);
#3944=VERTEX_POINT('',#20964);
#3945=VERTEX_POINT('',#21011);
#3946=VERTEX_POINT('',#21012);
#3947=VERTEX_POINT('',#21062);
#3948=VERTEX_POINT('',#21063);
#3949=VERTEX_POINT('',#21113);
#3950=VERTEX_POINT('',#21114);
#3951=VERTEX_POINT('',#21161);
#3952=VERTEX_POINT('',#21162);
#3953=VERTEX_POINT('',#21164);
#3954=VERTEX_POINT('',#21178);
#3955=VERTEX_POINT('',#21200);
#3956=VERTEX_POINT('',#21201);
#3957=VERTEX_POINT('',#21203);
#3958=VERTEX_POINT('',#21212);
#3959=VERTEX_POINT('',#21224);
#3960=VERTEX_POINT('',#21225);
#3961=VERTEX_POINT('',#21248);
#3962=VERTEX_POINT('',#21249);
#3963=VERTEX_POINT('',#21273);
#3964=VERTEX_POINT('',#21274);
#3965=VERTEX_POINT('',#21298);
#3966=VERTEX_POINT('',#21299);
#3967=VERTEX_POINT('',#21322);
#3968=VERTEX_POINT('',#21323);
#3969=VERTEX_POINT('',#21347);
#3970=VERTEX_POINT('',#21348);
#3971=VERTEX_POINT('',#21372);
#3972=VERTEX_POINT('',#21373);
#3973=VERTEX_POINT('',#21375);
#3974=VERTEX_POINT('',#21381);
#3975=VERTEX_POINT('',#21389);
#3976=VERTEX_POINT('',#21390);
#3977=VERTEX_POINT('',#21392);
#3978=VERTEX_POINT('',#21401);
#3979=VERTEX_POINT('',#21413);
#3980=VERTEX_POINT('',#21414);
#3981=VERTEX_POINT('',#21437);
#3982=VERTEX_POINT('',#21438);
#3983=VERTEX_POINT('',#21462);
#3984=VERTEX_POINT('',#21463);
#3985=VERTEX_POINT('',#21487);
#3986=VERTEX_POINT('',#21488);
#3987=VERTEX_POINT('',#21511);
#3988=VERTEX_POINT('',#21512);
#3989=VERTEX_POINT('',#21536);
#3990=VERTEX_POINT('',#21537);
#3991=VERTEX_POINT('',#21561);
#3992=VERTEX_POINT('',#21562);
#3993=VERTEX_POINT('',#21564);
#3994=VERTEX_POINT('',#21570);
#3995=VERTEX_POINT('',#22300);
#3996=VERTEX_POINT('',#22301);
#3997=VERTEX_POINT('',#22303);
#3998=VERTEX_POINT('',#22305);
#3999=VERTEX_POINT('',#22307);
#4000=VERTEX_POINT('',#22309);
#4001=VERTEX_POINT('',#23037);
#4002=VERTEX_POINT('',#23039);
#4003=VERTEX_POINT('',#23043);
#4004=VERTEX_POINT('',#23045);
#4005=VERTEX_POINT('',#23049);
#4006=VERTEX_POINT('',#23050);
#4007=VERTEX_POINT('',#23052);
#4008=VERTEX_POINT('',#23054);
#4009=VERTEX_POINT('',#23058);
#4010=VERTEX_POINT('',#23060);
#4011=VERTEX_POINT('',#23064);
#4012=VERTEX_POINT('',#23066);
#4013=VERTEX_POINT('',#23068);
#4014=VERTEX_POINT('',#23070);
#4015=VERTEX_POINT('',#23072);
#4016=VERTEX_POINT('',#23074);
#4017=VERTEX_POINT('',#23078);
#4018=VERTEX_POINT('',#23082);
#4019=VERTEX_POINT('',#23086);
#4020=VERTEX_POINT('',#23090);
#4021=VERTEX_POINT('',#23092);
#4022=VERTEX_POINT('',#23096);
#4023=VERTEX_POINT('',#23098);
#4024=VERTEX_POINT('',#23108);
#4025=VERTEX_POINT('',#23110);
#4026=VERTEX_POINT('',#23114);
#4027=VERTEX_POINT('',#23116);
#4028=VERTEX_POINT('',#23122);
#4029=VERTEX_POINT('',#23124);
#4030=VERTEX_POINT('',#23132);
#4031=VERTEX_POINT('',#23138);
#4032=VERTEX_POINT('',#23140);
#4033=VERTEX_POINT('',#23144);
#4034=VERTEX_POINT('',#23146);
#4035=VERTEX_POINT('',#23150);
#4036=VERTEX_POINT('',#23151);
#4037=VERTEX_POINT('',#23153);
#4038=VERTEX_POINT('',#23155);
#4039=VERTEX_POINT('',#23159);
#4040=VERTEX_POINT('',#23161);
#4041=VERTEX_POINT('',#23165);
#4042=VERTEX_POINT('',#23167);
#4043=VERTEX_POINT('',#23177);
#4044=VERTEX_POINT('',#23179);
#4045=VERTEX_POINT('',#23183);
#4046=VERTEX_POINT('',#23187);
#4047=VERTEX_POINT('',#23190);
#4048=VERTEX_POINT('',#23194);
#4049=VERTEX_POINT('',#23197);
#4050=VERTEX_POINT('',#23201);
#4051=VERTEX_POINT('',#23208);
#4052=VERTEX_POINT('',#23209);
#4053=VERTEX_POINT('',#23211);
#4054=VERTEX_POINT('',#23234);
#4055=VERTEX_POINT('',#23236);
#4056=VERTEX_POINT('',#23244);
#4057=VERTEX_POINT('',#23270);
#4058=VERTEX_POINT('',#23271);
#4059=VERTEX_POINT('',#23321);
#4060=VERTEX_POINT('',#23322);
#4061=VERTEX_POINT('',#23369);
#4062=VERTEX_POINT('',#23370);
#4063=VERTEX_POINT('',#23417);
#4064=VERTEX_POINT('',#23418);
#4065=VERTEX_POINT('',#23468);
#4066=VERTEX_POINT('',#23469);
#4067=VERTEX_POINT('',#23516);
#4068=VERTEX_POINT('',#23517);
#4069=VERTEX_POINT('',#23564);
#4070=VERTEX_POINT('',#23565);
#4071=VERTEX_POINT('',#23615);
#4072=VERTEX_POINT('',#23616);
#4073=VERTEX_POINT('',#23666);
#4074=VERTEX_POINT('',#23667);
#4075=VERTEX_POINT('',#23714);
#4076=VERTEX_POINT('',#23715);
#4077=VERTEX_POINT('',#23765);
#4078=VERTEX_POINT('',#23766);
#4079=VERTEX_POINT('',#23768);
#4080=VERTEX_POINT('',#23782);
#4081=VERTEX_POINT('',#23804);
#4082=VERTEX_POINT('',#23805);
#4083=VERTEX_POINT('',#23807);
#4084=VERTEX_POINT('',#23815);
#4085=VERTEX_POINT('',#23826);
#4086=VERTEX_POINT('',#23827);
#4087=VERTEX_POINT('',#23850);
#4088=VERTEX_POINT('',#23851);
#4089=VERTEX_POINT('',#23875);
#4090=VERTEX_POINT('',#23876);
#4091=VERTEX_POINT('',#23900);
#4092=VERTEX_POINT('',#23901);
#4093=VERTEX_POINT('',#23924);
#4094=VERTEX_POINT('',#23925);
#4095=VERTEX_POINT('',#23949);
#4096=VERTEX_POINT('',#23950);
#4097=VERTEX_POINT('',#23973);
#4098=VERTEX_POINT('',#23974);
#4099=VERTEX_POINT('',#23998);
#4100=VERTEX_POINT('',#23999);
#4101=VERTEX_POINT('',#24022);
#4102=VERTEX_POINT('',#24023);
#4103=VERTEX_POINT('',#24047);
#4104=VERTEX_POINT('',#24048);
#4105=VERTEX_POINT('',#24072);
#4106=VERTEX_POINT('',#24073);
#4107=VERTEX_POINT('',#24096);
#4108=VERTEX_POINT('',#24097);
#4109=VERTEX_POINT('',#24099);
#4110=VERTEX_POINT('',#24105);
#4111=VERTEX_POINT('',#24113);
#4112=VERTEX_POINT('',#24114);
#4113=VERTEX_POINT('',#24116);
#4114=VERTEX_POINT('',#24121);
#4115=VERTEX_POINT('',#24123);
#4116=VERTEX_POINT('',#24126);
#4117=VERTEX_POINT('',#24139);
#4118=VERTEX_POINT('',#24140);
#4119=VERTEX_POINT('',#24190);
#4120=VERTEX_POINT('',#24191);
#4121=VERTEX_POINT('',#24241);
#4122=VERTEX_POINT('',#24242);
#4123=VERTEX_POINT('',#24289);
#4124=VERTEX_POINT('',#24290);
#4125=VERTEX_POINT('',#24340);
#4126=VERTEX_POINT('',#24341);
#4127=VERTEX_POINT('',#24391);
#4128=VERTEX_POINT('',#24392);
#4129=VERTEX_POINT('',#24439);
#4130=VERTEX_POINT('',#24440);
#4131=VERTEX_POINT('',#24490);
#4132=VERTEX_POINT('',#24491);
#4133=VERTEX_POINT('',#24541);
#4134=VERTEX_POINT('',#24542);
#4135=VERTEX_POINT('',#24589);
#4136=VERTEX_POINT('',#24590);
#4137=VERTEX_POINT('',#24640);
#4138=VERTEX_POINT('',#24641);
#4139=VERTEX_POINT('',#24691);
#4140=VERTEX_POINT('',#24692);
#4141=VERTEX_POINT('',#24739);
#4142=VERTEX_POINT('',#24740);
#4143=VERTEX_POINT('',#24790);
#4144=VERTEX_POINT('',#24791);
#4145=VERTEX_POINT('',#24841);
#4146=VERTEX_POINT('',#24842);
#4147=VERTEX_POINT('',#24889);
#4148=VERTEX_POINT('',#24890);
#4149=VERTEX_POINT('',#24940);
#4150=VERTEX_POINT('',#24941);
#4151=VERTEX_POINT('',#24943);
#4152=VERTEX_POINT('',#24957);
#4153=VERTEX_POINT('',#24979);
#4154=VERTEX_POINT('',#24980);
#4155=VERTEX_POINT('',#24982);
#4156=VERTEX_POINT('',#24991);
#4157=VERTEX_POINT('',#25003);
#4158=VERTEX_POINT('',#25004);
#4159=VERTEX_POINT('',#25027);
#4160=VERTEX_POINT('',#25028);
#4161=VERTEX_POINT('',#25052);
#4162=VERTEX_POINT('',#25053);
#4163=VERTEX_POINT('',#25077);
#4164=VERTEX_POINT('',#25078);
#4165=VERTEX_POINT('',#25101);
#4166=VERTEX_POINT('',#25102);
#4167=VERTEX_POINT('',#25126);
#4168=VERTEX_POINT('',#25127);
#4169=VERTEX_POINT('',#25151);
#4170=VERTEX_POINT('',#25152);
#4171=VERTEX_POINT('',#25175);
#4172=VERTEX_POINT('',#25176);
#4173=VERTEX_POINT('',#25200);
#4174=VERTEX_POINT('',#25201);
#4175=VERTEX_POINT('',#25225);
#4176=VERTEX_POINT('',#25226);
#4177=VERTEX_POINT('',#25249);
#4178=VERTEX_POINT('',#25250);
#4179=VERTEX_POINT('',#25274);
#4180=VERTEX_POINT('',#25275);
#4181=VERTEX_POINT('',#25299);
#4182=VERTEX_POINT('',#25300);
#4183=VERTEX_POINT('',#25323);
#4184=VERTEX_POINT('',#25324);
#4185=VERTEX_POINT('',#25348);
#4186=VERTEX_POINT('',#25349);
#4187=VERTEX_POINT('',#25373);
#4188=VERTEX_POINT('',#25374);
#4189=VERTEX_POINT('',#25397);
#4190=VERTEX_POINT('',#25398);
#4191=VERTEX_POINT('',#25400);
#4192=VERTEX_POINT('',#25406);
#4193=VERTEX_POINT('',#27617);
#4194=VERTEX_POINT('',#27618);
#4195=VERTEX_POINT('',#27620);
#4196=VERTEX_POINT('',#27622);
#4197=VERTEX_POINT('',#27626);
#4198=VERTEX_POINT('',#27628);
#4199=VERTEX_POINT('',#27632);
#4200=VERTEX_POINT('',#27634);
#4201=VERTEX_POINT('',#27644);
#4202=VERTEX_POINT('',#27645);
#4203=VERTEX_POINT('',#27647);
#4204=VERTEX_POINT('',#27652);
#4205=VERTEX_POINT('',#27654);
#4206=VERTEX_POINT('',#27657);
#4207=VERTEX_POINT('',#27670);
#4208=VERTEX_POINT('',#27671);
#4209=VERTEX_POINT('',#27721);
#4210=VERTEX_POINT('',#27722);
#4211=VERTEX_POINT('',#27772);
#4212=VERTEX_POINT('',#27773);
#4213=VERTEX_POINT('',#27820);
#4214=VERTEX_POINT('',#27821);
#4215=VERTEX_POINT('',#27868);
#4216=VERTEX_POINT('',#27869);
#4217=VERTEX_POINT('',#27919);
#4218=VERTEX_POINT('',#27920);
#4219=VERTEX_POINT('',#27970);
#4220=VERTEX_POINT('',#27971);
#4221=VERTEX_POINT('',#28018);
#4222=VERTEX_POINT('',#28019);
#4223=VERTEX_POINT('',#28069);
#4224=VERTEX_POINT('',#28070);
#4225=VERTEX_POINT('',#28072);
#4226=VERTEX_POINT('',#28086);
#4227=VERTEX_POINT('',#28108);
#4228=VERTEX_POINT('',#28109);
#4229=VERTEX_POINT('',#28111);
#4230=VERTEX_POINT('',#28120);
#4231=VERTEX_POINT('',#28132);
#4232=VERTEX_POINT('',#28133);
#4233=VERTEX_POINT('',#28156);
#4234=VERTEX_POINT('',#28157);
#4235=VERTEX_POINT('',#28181);
#4236=VERTEX_POINT('',#28182);
#4237=VERTEX_POINT('',#28205);
#4238=VERTEX_POINT('',#28206);
#4239=VERTEX_POINT('',#28230);
#4240=VERTEX_POINT('',#28231);
#4241=VERTEX_POINT('',#28254);
#4242=VERTEX_POINT('',#28255);
#4243=VERTEX_POINT('',#28279);
#4244=VERTEX_POINT('',#28280);
#4245=VERTEX_POINT('',#28304);
#4246=VERTEX_POINT('',#28305);
#4247=VERTEX_POINT('',#28328);
#4248=VERTEX_POINT('',#28329);
#4249=VERTEX_POINT('',#28331);
#4250=VERTEX_POINT('',#28337);
#4251=VERTEX_POINT('',#29166);
#4252=VERTEX_POINT('',#29168);
#4253=VERTEX_POINT('',#29172);
#4254=VERTEX_POINT('',#29173);
#4255=VERTEX_POINT('',#29175);
#4256=VERTEX_POINT('',#29177);
#4257=VERTEX_POINT('',#29181);
#4258=VERTEX_POINT('',#29182);
#4259=VERTEX_POINT('',#29187);
#4260=VERTEX_POINT('',#29189);
#4261=VERTEX_POINT('',#29191);
#4262=VERTEX_POINT('',#29195);
#4263=VERTEX_POINT('',#29199);
#4264=VERTEX_POINT('',#29201);
#4265=VERTEX_POINT('',#29211);
#4266=VERTEX_POINT('',#29213);
#4267=VERTEX_POINT('',#29217);
#4268=VERTEX_POINT('',#29218);
#4269=VERTEX_POINT('',#29220);
#4270=VERTEX_POINT('',#29222);
#4271=VERTEX_POINT('',#29226);
#4272=VERTEX_POINT('',#29228);
#4273=VERTEX_POINT('',#29232);
#4274=VERTEX_POINT('',#29234);
#4275=VERTEX_POINT('',#29244);
#4276=VERTEX_POINT('',#29246);
#4277=VERTEX_POINT('',#29250);
#4278=VERTEX_POINT('',#29252);
#4279=VERTEX_POINT('',#29259);
#4280=VERTEX_POINT('',#29261);
#4281=VERTEX_POINT('',#29265);
#4282=VERTEX_POINT('',#29268);
#4283=VERTEX_POINT('',#29271);
#4284=VERTEX_POINT('',#29275);
#4285=VERTEX_POINT('',#29277);
#4286=VERTEX_POINT('',#29280);
#4287=VERTEX_POINT('',#29289);
#4288=VERTEX_POINT('',#29290);
#4289=VERTEX_POINT('',#29292);
#4290=VERTEX_POINT('',#29294);
#4291=VERTEX_POINT('',#29298);
#4292=VERTEX_POINT('',#29299);
#4293=VERTEX_POINT('',#29301);
#4294=VERTEX_POINT('',#29303);
#4295=VERTEX_POINT('',#29605);
#4296=VERTEX_POINT('',#29607);
#4297=VERTEX_POINT('',#29642);
#4298=VERTEX_POINT('',#29644);
#4299=VERTEX_POINT('',#29648);
#4300=VERTEX_POINT('',#29650);
#4301=VERTEX_POINT('',#29657);
#4302=VERTEX_POINT('',#29658);
#4303=VERTEX_POINT('',#29660);
#4304=VERTEX_POINT('',#29671);
#4305=VERTEX_POINT('',#29681);
#4306=VERTEX_POINT('',#29682);
#4307=VERTEX_POINT('',#29729);
#4308=VERTEX_POINT('',#29730);
#4309=VERTEX_POINT('',#29777);
#4310=VERTEX_POINT('',#29778);
#4311=VERTEX_POINT('',#29825);
#4312=VERTEX_POINT('',#29826);
#4313=VERTEX_POINT('',#29873);
#4314=VERTEX_POINT('',#29874);
#4315=VERTEX_POINT('',#29921);
#4316=VERTEX_POINT('',#29922);
#4317=VERTEX_POINT('',#29969);
#4318=VERTEX_POINT('',#29970);
#4319=VERTEX_POINT('',#30023);
#4320=VERTEX_POINT('',#30024);
#4321=VERTEX_POINT('',#30071);
#4322=VERTEX_POINT('',#30072);
#4323=VERTEX_POINT('',#30119);
#4324=VERTEX_POINT('',#30120);
#4325=VERTEX_POINT('',#30173);
#4326=VERTEX_POINT('',#30174);
#4327=VERTEX_POINT('',#30221);
#4328=VERTEX_POINT('',#30222);
#4329=VERTEX_POINT('',#30269);
#4330=VERTEX_POINT('',#30270);
#4331=VERTEX_POINT('',#30317);
#4332=VERTEX_POINT('',#30318);
#4333=VERTEX_POINT('',#30368);
#4334=VERTEX_POINT('',#30369);
#4335=VERTEX_POINT('',#30416);
#4336=VERTEX_POINT('',#30417);
#4337=VERTEX_POINT('',#30419);
#4338=VERTEX_POINT('',#30428);
#4339=VERTEX_POINT('',#30438);
#4340=VERTEX_POINT('',#30439);
#4341=VERTEX_POINT('',#30462);
#4342=VERTEX_POINT('',#30463);
#4343=VERTEX_POINT('',#30486);
#4344=VERTEX_POINT('',#30487);
#4345=VERTEX_POINT('',#30512);
#4346=VERTEX_POINT('',#30513);
#4347=VERTEX_POINT('',#30536);
#4348=VERTEX_POINT('',#30537);
#4349=VERTEX_POINT('',#30560);
#4350=VERTEX_POINT('',#30561);
#4351=VERTEX_POINT('',#30585);
#4352=VERTEX_POINT('',#30586);
#4353=VERTEX_POINT('',#30610);
#4354=VERTEX_POINT('',#30611);
#4355=VERTEX_POINT('',#30634);
#4356=VERTEX_POINT('',#30635);
#4357=VERTEX_POINT('',#30659);
#4358=VERTEX_POINT('',#30660);
#4359=VERTEX_POINT('',#30684);
#4360=VERTEX_POINT('',#30685);
#4361=VERTEX_POINT('',#30708);
#4362=VERTEX_POINT('',#30709);
#4363=VERTEX_POINT('',#30732);
#4364=VERTEX_POINT('',#30733);
#4365=VERTEX_POINT('',#30757);
#4366=VERTEX_POINT('',#30758);
#4367=VERTEX_POINT('',#30782);
#4368=VERTEX_POINT('',#30783);
#4369=VERTEX_POINT('',#30806);
#4370=VERTEX_POINT('',#30886);
#4371=VERTEX_POINT('',#30921);
#4372=VERTEX_POINT('',#30987);
#4373=VERTEX_POINT('',#31414);
#4374=VERTEX_POINT('',#31495);
#4375=VERTEX_POINT('',#32008);
#4376=VERTEX_POINT('',#32009);
#4377=VERTEX_POINT('',#32011);
#4378=VERTEX_POINT('',#32013);
#4379=VERTEX_POINT('',#32017);
#4380=VERTEX_POINT('',#32019);
#4381=VERTEX_POINT('',#32023);
#4382=VERTEX_POINT('',#32025);
#4383=VERTEX_POINT('',#32029);
#4384=VERTEX_POINT('',#32031);
#4385=VERTEX_POINT('',#32035);
#4386=VERTEX_POINT('',#32037);
#4387=VERTEX_POINT('',#32045);
#4388=VERTEX_POINT('',#32048);
#4389=VERTEX_POINT('',#32055);
#4390=VERTEX_POINT('',#32056);
#4391=VERTEX_POINT('',#32058);
#4392=VERTEX_POINT('',#32069);
#4393=VERTEX_POINT('',#32079);
#4394=VERTEX_POINT('',#32080);
#4395=VERTEX_POINT('',#32127);
#4396=VERTEX_POINT('',#32128);
#4397=VERTEX_POINT('',#32175);
#4398=VERTEX_POINT('',#32176);
#4399=VERTEX_POINT('',#32223);
#4400=VERTEX_POINT('',#32224);
#4401=VERTEX_POINT('',#32277);
#4402=VERTEX_POINT('',#32278);
#4403=VERTEX_POINT('',#32325);
#4404=VERTEX_POINT('',#32326);
#4405=VERTEX_POINT('',#32373);
#4406=VERTEX_POINT('',#32374);
#4407=VERTEX_POINT('',#32427);
#4408=VERTEX_POINT('',#32428);
#4409=VERTEX_POINT('',#32475);
#4410=VERTEX_POINT('',#32476);
#4411=VERTEX_POINT('',#32523);
#4412=VERTEX_POINT('',#32524);
#4413=VERTEX_POINT('',#32526);
#4414=VERTEX_POINT('',#32537);
#4415=VERTEX_POINT('',#32549);
#4416=VERTEX_POINT('',#32550);
#4417=VERTEX_POINT('',#32573);
#4418=VERTEX_POINT('',#32574);
#4419=VERTEX_POINT('',#32597);
#4420=VERTEX_POINT('',#32598);
#4421=VERTEX_POINT('',#32622);
#4422=VERTEX_POINT('',#32623);
#4423=VERTEX_POINT('',#32647);
#4424=VERTEX_POINT('',#32648);
#4425=VERTEX_POINT('',#32671);
#4426=VERTEX_POINT('',#32672);
#4427=VERTEX_POINT('',#32696);
#4428=VERTEX_POINT('',#32697);
#4429=VERTEX_POINT('',#32721);
#4430=VERTEX_POINT('',#32722);
#4431=VERTEX_POINT('',#32745);
#4432=VERTEX_POINT('',#32746);
#4433=VERTEX_POINT('',#32769);
#4434=VERTEX_POINT('',#32894);
#4435=VERTEX_POINT('',#32932);
#4436=VERTEX_POINT('',#32950);
#4437=VERTEX_POINT('',#33233);
#4438=VERTEX_POINT('',#33311);
#4439=VERTEX_POINT('',#33686);
#4440=VERTEX_POINT('',#33687);
#4441=VERTEX_POINT('',#33689);
#4442=VERTEX_POINT('',#33691);
#4443=VERTEX_POINT('',#33695);
#4444=VERTEX_POINT('',#33697);
#4445=VERTEX_POINT('',#33701);
#4446=VERTEX_POINT('',#33703);
#4447=VERTEX_POINT('',#33707);
#4448=VERTEX_POINT('',#33709);
#4449=VERTEX_POINT('',#33713);
#4450=VERTEX_POINT('',#33715);
#4451=VERTEX_POINT('',#33723);
#4452=VERTEX_POINT('',#33726);
#4453=VERTEX_POINT('',#33733);
#4454=VERTEX_POINT('',#33734);
#4455=VERTEX_POINT('',#33736);
#4456=VERTEX_POINT('',#33747);
#4457=VERTEX_POINT('',#33757);
#4458=VERTEX_POINT('',#33758);
#4459=VERTEX_POINT('',#33805);
#4460=VERTEX_POINT('',#33806);
#4461=VERTEX_POINT('',#33853);
#4462=VERTEX_POINT('',#33854);
#4463=VERTEX_POINT('',#33907);
#4464=VERTEX_POINT('',#33908);
#4465=VERTEX_POINT('',#33955);
#4466=VERTEX_POINT('',#33956);
#4467=VERTEX_POINT('',#34003);
#4468=VERTEX_POINT('',#34004);
#4469=VERTEX_POINT('',#34057);
#4470=VERTEX_POINT('',#34058);
#4471=VERTEX_POINT('',#34105);
#4472=VERTEX_POINT('',#34106);
#4473=VERTEX_POINT('',#34153);
#4474=VERTEX_POINT('',#34154);
#4475=VERTEX_POINT('',#34207);
#4476=VERTEX_POINT('',#34208);
#4477=VERTEX_POINT('',#34255);
#4478=VERTEX_POINT('',#34256);
#4479=VERTEX_POINT('',#34303);
#4480=VERTEX_POINT('',#34304);
#4481=VERTEX_POINT('',#34357);
#4482=VERTEX_POINT('',#34358);
#4483=VERTEX_POINT('',#34405);
#4484=VERTEX_POINT('',#34406);
#4485=VERTEX_POINT('',#34453);
#4486=VERTEX_POINT('',#34454);
#4487=VERTEX_POINT('',#34504);
#4488=VERTEX_POINT('',#34505);
#4489=VERTEX_POINT('',#34552);
#4490=VERTEX_POINT('',#34553);
#4491=VERTEX_POINT('',#34600);
#4492=VERTEX_POINT('',#34601);
#4493=VERTEX_POINT('',#34603);
#4494=VERTEX_POINT('',#34614);
#4495=VERTEX_POINT('',#34626);
#4496=VERTEX_POINT('',#34627);
#4497=VERTEX_POINT('',#34650);
#4498=VERTEX_POINT('',#34651);
#4499=VERTEX_POINT('',#34674);
#4500=VERTEX_POINT('',#34675);
#4501=VERTEX_POINT('',#34700);
#4502=VERTEX_POINT('',#34701);
#4503=VERTEX_POINT('',#34724);
#4504=VERTEX_POINT('',#34725);
#4505=VERTEX_POINT('',#34748);
#4506=VERTEX_POINT('',#34749);
#4507=VERTEX_POINT('',#34773);
#4508=VERTEX_POINT('',#34774);
#4509=VERTEX_POINT('',#34798);
#4510=VERTEX_POINT('',#34799);
#4511=VERTEX_POINT('',#34822);
#4512=VERTEX_POINT('',#34823);
#4513=VERTEX_POINT('',#34847);
#4514=VERTEX_POINT('',#34848);
#4515=VERTEX_POINT('',#34872);
#4516=VERTEX_POINT('',#34873);
#4517=VERTEX_POINT('',#34896);
#4518=VERTEX_POINT('',#34897);
#4519=VERTEX_POINT('',#34921);
#4520=VERTEX_POINT('',#34922);
#4521=VERTEX_POINT('',#34946);
#4522=VERTEX_POINT('',#34947);
#4523=VERTEX_POINT('',#34970);
#4524=VERTEX_POINT('',#34971);
#4525=VERTEX_POINT('',#34995);
#4526=VERTEX_POINT('',#34996);
#4527=VERTEX_POINT('',#35020);
#4528=VERTEX_POINT('',#35021);
#4529=VERTEX_POINT('',#35044);
#4530=VERTEX_POINT('',#35166);
#4531=VERTEX_POINT('',#35201);
#4532=VERTEX_POINT('',#35219);
#4533=VERTEX_POINT('',#35706);
#4534=VERTEX_POINT('',#35790);
#4535=VERTEX_POINT('',#36369);
#4536=VERTEX_POINT('',#36370);
#4537=VERTEX_POINT('',#36372);
#4538=VERTEX_POINT('',#36374);
#4539=VERTEX_POINT('',#36378);
#4540=VERTEX_POINT('',#36380);
#4541=VERTEX_POINT('',#36384);
#4542=VERTEX_POINT('',#36386);
#4543=VERTEX_POINT('',#36390);
#4544=VERTEX_POINT('',#36392);
#4545=VERTEX_POINT('',#36396);
#4546=VERTEX_POINT('',#36398);
#4547=VERTEX_POINT('',#36406);
#4548=VERTEX_POINT('',#36409);
#4549=EDGE_CURVE('',#3593,#3594,#2445,.T.);
#4550=EDGE_CURVE('',#3594,#3595,#1738,.T.);
#4551=EDGE_CURVE('',#3595,#3596,#1582,.T.);
#4552=EDGE_CURVE('',#3596,#3597,#1739,.T.);
#4553=EDGE_CURVE('',#3597,#3598,#2446,.T.);
#4554=EDGE_CURVE('',#3598,#3598,#1583,.F.);
#4555=EDGE_CURVE('',#3597,#3593,#1740,.T.);
#4556=EDGE_CURVE('',#3599,#3600,#2447,.T.);
#4557=EDGE_CURVE('',#3600,#3594,#1741,.T.);
#4558=EDGE_CURVE('',#3593,#3599,#1742,.T.);
#4559=EDGE_CURVE('',#3601,#3602,#2448,.T.);
#4560=EDGE_CURVE('',#3602,#3600,#1743,.T.);
#4561=EDGE_CURVE('',#3599,#3601,#1744,.T.);
#4562=EDGE_CURVE('',#3603,#3604,#2449,.T.);
#4563=EDGE_CURVE('',#3604,#3602,#1745,.T.);
#4564=EDGE_CURVE('',#3601,#3603,#1746,.T.);
#4565=EDGE_CURVE('',#3605,#3606,#2450,.T.);
#4566=EDGE_CURVE('',#3606,#3604,#1747,.T.);
#4567=EDGE_CURVE('',#3603,#3605,#1748,.T.);
#4568=EDGE_CURVE('',#3607,#3608,#2451,.T.);
#4569=EDGE_CURVE('',#3608,#3606,#1749,.T.);
#4570=EDGE_CURVE('',#3605,#3607,#1750,.T.);
#4571=EDGE_CURVE('',#3609,#3610,#2452,.T.);
#4572=EDGE_CURVE('',#3610,#3608,#1751,.T.);
#4573=EDGE_CURVE('',#3607,#3609,#1752,.T.);
#4574=EDGE_CURVE('',#3611,#3612,#2453,.T.);
#4575=EDGE_CURVE('',#3612,#3610,#1753,.T.);
#4576=EDGE_CURVE('',#3609,#3611,#1754,.T.);
#4577=EDGE_CURVE('',#3613,#3614,#2454,.T.);
#4578=EDGE_CURVE('',#3614,#3612,#1755,.T.);
#4579=EDGE_CURVE('',#3611,#3613,#1756,.T.);
#4580=EDGE_CURVE('',#3615,#3616,#2455,.T.);
#4581=EDGE_CURVE('',#3616,#3614,#1757,.T.);
#4582=EDGE_CURVE('',#3613,#3615,#1758,.T.);
#4583=EDGE_CURVE('',#3617,#3618,#2456,.T.);
#4584=EDGE_CURVE('',#3618,#3616,#1759,.T.);
#4585=EDGE_CURVE('',#3615,#3617,#1760,.T.);
#4586=EDGE_CURVE('',#3619,#3620,#2457,.T.);
#4587=EDGE_CURVE('',#3619,#3621,#1761,.T.);
#4588=EDGE_CURVE('',#3622,#3621,#1584,.T.);
#4589=EDGE_CURVE('',#3622,#3620,#1762,.T.);
#4590=EDGE_CURVE('',#3623,#3624,#2458,.T.);
#4591=EDGE_CURVE('',#3624,#3625,#1763,.T.);
#4592=EDGE_CURVE('',#3626,#3625,#1585,.T.);
#4593=EDGE_CURVE('',#3623,#3626,#1764,.T.);
#4594=EDGE_CURVE('',#3627,#3628,#2459,.T.);
#4595=EDGE_CURVE('',#3628,#3624,#1765,.T.);
#4596=EDGE_CURVE('',#3627,#3623,#1766,.T.);
#4597=EDGE_CURVE('',#3629,#3630,#2460,.T.);
#4598=EDGE_CURVE('',#3630,#3628,#1767,.T.);
#4599=EDGE_CURVE('',#3629,#3627,#1768,.T.);
#4600=EDGE_CURVE('',#3631,#3632,#2461,.T.);
#4601=EDGE_CURVE('',#3632,#3630,#1769,.T.);
#4602=EDGE_CURVE('',#3631,#3629,#1770,.T.);
#4603=EDGE_CURVE('',#3633,#3634,#2462,.T.);
#4604=EDGE_CURVE('',#3634,#3632,#1771,.T.);
#4605=EDGE_CURVE('',#3633,#3631,#1772,.T.);
#4606=EDGE_CURVE('',#3635,#3636,#2463,.T.);
#4607=EDGE_CURVE('',#3636,#3634,#1773,.T.);
#4608=EDGE_CURVE('',#3635,#3633,#1774,.T.);
#4609=EDGE_CURVE('',#3637,#3638,#2464,.T.);
#4610=EDGE_CURVE('',#3638,#3636,#1775,.T.);
#4611=EDGE_CURVE('',#3637,#3635,#1776,.T.);
#4612=EDGE_CURVE('',#3639,#3640,#2465,.T.);
#4613=EDGE_CURVE('',#3640,#3638,#1777,.T.);
#4614=EDGE_CURVE('',#3639,#3637,#1778,.T.);
#4615=EDGE_CURVE('',#3641,#3642,#2466,.T.);
#4616=EDGE_CURVE('',#3642,#3640,#1779,.T.);
#4617=EDGE_CURVE('',#3641,#3639,#1780,.T.);
#4618=EDGE_CURVE('',#3643,#3644,#2467,.T.);
#4619=EDGE_CURVE('',#3644,#3642,#1781,.T.);
#4620=EDGE_CURVE('',#3643,#3641,#1782,.T.);
#4621=EDGE_CURVE('',#3645,#3646,#2468,.T.);
#4622=EDGE_CURVE('',#3646,#3644,#1783,.T.);
#4623=EDGE_CURVE('',#3645,#3643,#1784,.T.);
#4624=EDGE_CURVE('',#3647,#3648,#2469,.T.);
#4625=EDGE_CURVE('',#3648,#3646,#1785,.T.);
#4626=EDGE_CURVE('',#3647,#3645,#1786,.T.);
#4627=EDGE_CURVE('',#3649,#3650,#2470,.T.);
#4628=EDGE_CURVE('',#3651,#3649,#1787,.T.);
#4629=EDGE_CURVE('',#3652,#3651,#1586,.T.);
#4630=EDGE_CURVE('',#3652,#3650,#1788,.T.);
#4631=EDGE_CURVE('',#3653,#3654,#2471,.T.);
#4632=EDGE_CURVE('',#3654,#3655,#1789,.T.);
#4633=EDGE_CURVE('',#3655,#3656,#1587,.T.);
#4634=EDGE_CURVE('',#3656,#3657,#1790,.T.);
#4635=EDGE_CURVE('',#3657,#3658,#2472,.T.);
#4636=EDGE_CURVE('',#3658,#3658,#1588,.F.);
#4637=EDGE_CURVE('',#3657,#3653,#1791,.T.);
#4638=EDGE_CURVE('',#3659,#3660,#2473,.T.);
#4639=EDGE_CURVE('',#3660,#3654,#1792,.T.);
#4640=EDGE_CURVE('',#3653,#3659,#1793,.T.);
#4641=EDGE_CURVE('',#3661,#3662,#2474,.T.);
#4642=EDGE_CURVE('',#3662,#3660,#1794,.T.);
#4643=EDGE_CURVE('',#3659,#3661,#1795,.T.);
#4644=EDGE_CURVE('',#3663,#3664,#2475,.T.);
#4645=EDGE_CURVE('',#3664,#3662,#1796,.T.);
#4646=EDGE_CURVE('',#3661,#3663,#1797,.T.);
#4647=EDGE_CURVE('',#3665,#3666,#2476,.T.);
#4648=EDGE_CURVE('',#3666,#3664,#1798,.T.);
#4649=EDGE_CURVE('',#3663,#3665,#1799,.T.);
#4650=EDGE_CURVE('',#3667,#3668,#2477,.T.);
#4651=EDGE_CURVE('',#3668,#3666,#1800,.T.);
#4652=EDGE_CURVE('',#3665,#3667,#1801,.T.);
#4653=EDGE_CURVE('',#3669,#3670,#2478,.T.);
#4654=EDGE_CURVE('',#3670,#3668,#1802,.T.);
#4655=EDGE_CURVE('',#3667,#3669,#1803,.T.);
#4656=EDGE_CURVE('',#3671,#3672,#2479,.T.);
#4657=EDGE_CURVE('',#3672,#3670,#1804,.T.);
#4658=EDGE_CURVE('',#3669,#3671,#1805,.T.);
#4659=EDGE_CURVE('',#3673,#3674,#2480,.T.);
#4660=EDGE_CURVE('',#3674,#3672,#1806,.T.);
#4661=EDGE_CURVE('',#3671,#3673,#1807,.T.);
#4662=EDGE_CURVE('',#3675,#3676,#2481,.T.);
#4663=EDGE_CURVE('',#3676,#3674,#1808,.T.);
#4664=EDGE_CURVE('',#3673,#3675,#1809,.T.);
#4665=EDGE_CURVE('',#3677,#3678,#2482,.T.);
#4666=EDGE_CURVE('',#3678,#3676,#1810,.T.);
#4667=EDGE_CURVE('',#3675,#3677,#1811,.T.);
#4668=EDGE_CURVE('',#3679,#3680,#2483,.T.);
#4669=EDGE_CURVE('',#3679,#3681,#1812,.T.);
#4670=EDGE_CURVE('',#3682,#3681,#1589,.T.);
#4671=EDGE_CURVE('',#3682,#3680,#1813,.T.);
#4672=EDGE_CURVE('',#3683,#3684,#2484,.T.);
#4673=EDGE_CURVE('',#3684,#3685,#1814,.T.);
#4674=EDGE_CURVE('',#3686,#3685,#1590,.T.);
#4675=EDGE_CURVE('',#3683,#3686,#1815,.T.);
#4676=EDGE_CURVE('',#3687,#3688,#2485,.T.);
#4677=EDGE_CURVE('',#3688,#3684,#1816,.T.);
#4678=EDGE_CURVE('',#3687,#3683,#1817,.T.);
#4679=EDGE_CURVE('',#3689,#3690,#2486,.T.);
#4680=EDGE_CURVE('',#3690,#3688,#1818,.T.);
#4681=EDGE_CURVE('',#3689,#3687,#1819,.T.);
#4682=EDGE_CURVE('',#3691,#3692,#2487,.T.);
#4683=EDGE_CURVE('',#3692,#3690,#1820,.T.);
#4684=EDGE_CURVE('',#3691,#3689,#1821,.T.);
#4685=EDGE_CURVE('',#3693,#3694,#2488,.T.);
#4686=EDGE_CURVE('',#3694,#3692,#1822,.T.);
#4687=EDGE_CURVE('',#3693,#3691,#1823,.T.);
#4688=EDGE_CURVE('',#3695,#3696,#2489,.T.);
#4689=EDGE_CURVE('',#3696,#3694,#1824,.T.);
#4690=EDGE_CURVE('',#3695,#3693,#1825,.T.);
#4691=EDGE_CURVE('',#3697,#3698,#2490,.T.);
#4692=EDGE_CURVE('',#3698,#3696,#1826,.T.);
#4693=EDGE_CURVE('',#3697,#3695,#1827,.T.);
#4694=EDGE_CURVE('',#3699,#3700,#2491,.T.);
#4695=EDGE_CURVE('',#3700,#3698,#1828,.T.);
#4696=EDGE_CURVE('',#3699,#3697,#1829,.T.);
#4697=EDGE_CURVE('',#3701,#3702,#2492,.T.);
#4698=EDGE_CURVE('',#3702,#3700,#1830,.T.);
#4699=EDGE_CURVE('',#3701,#3699,#1831,.T.);
#4700=EDGE_CURVE('',#3703,#3704,#2493,.T.);
#4701=EDGE_CURVE('',#3704,#3702,#1832,.T.);
#4702=EDGE_CURVE('',#3703,#3701,#1833,.T.);
#4703=EDGE_CURVE('',#3705,#3706,#2494,.T.);
#4704=EDGE_CURVE('',#3706,#3704,#1834,.T.);
#4705=EDGE_CURVE('',#3705,#3703,#1835,.T.);
#4706=EDGE_CURVE('',#3707,#3708,#2495,.T.);
#4707=EDGE_CURVE('',#3708,#3706,#1836,.T.);
#4708=EDGE_CURVE('',#3707,#3705,#1837,.T.);
#4709=EDGE_CURVE('',#3709,#3710,#2496,.T.);
#4710=EDGE_CURVE('',#3711,#3709,#1838,.T.);
#4711=EDGE_CURVE('',#3712,#3711,#1591,.T.);
#4712=EDGE_CURVE('',#3712,#3710,#1839,.T.);
#4713=EDGE_CURVE('',#3713,#3714,#2497,.T.);
#4714=EDGE_CURVE('',#3714,#3715,#1840,.T.);
#4715=EDGE_CURVE('',#3715,#3716,#1592,.T.);
#4716=EDGE_CURVE('',#3716,#3717,#1841,.T.);
#4717=EDGE_CURVE('',#3717,#3718,#2498,.T.);
#4718=EDGE_CURVE('',#3718,#3718,#1593,.F.);
#4719=EDGE_CURVE('',#3717,#3713,#1842,.T.);
#4720=EDGE_CURVE('',#3719,#3720,#2499,.T.);
#4721=EDGE_CURVE('',#3720,#3714,#1843,.T.);
#4722=EDGE_CURVE('',#3713,#3719,#1844,.T.);
#4723=EDGE_CURVE('',#3721,#3722,#2500,.T.);
#4724=EDGE_CURVE('',#3722,#3720,#1845,.T.);
#4725=EDGE_CURVE('',#3719,#3721,#1846,.T.);
#4726=EDGE_CURVE('',#3723,#3724,#2501,.T.);
#4727=EDGE_CURVE('',#3724,#3722,#1847,.T.);
#4728=EDGE_CURVE('',#3721,#3723,#1848,.T.);
#4729=EDGE_CURVE('',#3725,#3726,#2502,.T.);
#4730=EDGE_CURVE('',#3726,#3724,#1849,.T.);
#4731=EDGE_CURVE('',#3723,#3725,#1850,.T.);
#4732=EDGE_CURVE('',#3727,#3728,#2503,.T.);
#4733=EDGE_CURVE('',#3728,#3726,#1851,.T.);
#4734=EDGE_CURVE('',#3725,#3727,#1852,.T.);
#4735=EDGE_CURVE('',#3729,#3730,#2504,.T.);
#4736=EDGE_CURVE('',#3730,#3728,#1853,.T.);
#4737=EDGE_CURVE('',#3727,#3729,#1854,.T.);
#4738=EDGE_CURVE('',#3731,#3732,#2505,.T.);
#4739=EDGE_CURVE('',#3732,#3730,#1855,.T.);
#4740=EDGE_CURVE('',#3729,#3731,#1856,.T.);
#4741=EDGE_CURVE('',#3733,#3734,#2506,.T.);
#4742=EDGE_CURVE('',#3734,#3732,#1857,.T.);
#4743=EDGE_CURVE('',#3731,#3733,#1858,.T.);
#4744=EDGE_CURVE('',#3735,#3736,#2507,.T.);
#4745=EDGE_CURVE('',#3736,#3734,#1859,.T.);
#4746=EDGE_CURVE('',#3733,#3735,#1860,.T.);
#4747=EDGE_CURVE('',#3737,#3738,#2508,.T.);
#4748=EDGE_CURVE('',#3738,#3736,#1861,.T.);
#4749=EDGE_CURVE('',#3735,#3737,#1862,.T.);
#4750=EDGE_CURVE('',#3739,#3740,#2509,.T.);
#4751=EDGE_CURVE('',#3739,#3741,#1863,.T.);
#4752=EDGE_CURVE('',#3742,#3741,#1594,.T.);
#4753=EDGE_CURVE('',#3742,#3740,#1864,.T.);
#4754=EDGE_CURVE('',#3743,#3744,#2510,.T.);
#4755=EDGE_CURVE('',#3744,#3745,#1865,.T.);
#4756=EDGE_CURVE('',#3746,#3745,#1595,.T.);
#4757=EDGE_CURVE('',#3743,#3746,#1866,.T.);
#4758=EDGE_CURVE('',#3747,#3748,#2511,.T.);
#4759=EDGE_CURVE('',#3748,#3744,#1867,.T.);
#4760=EDGE_CURVE('',#3747,#3743,#1868,.T.);
#4761=EDGE_CURVE('',#3749,#3750,#2512,.T.);
#4762=EDGE_CURVE('',#3750,#3748,#1869,.T.);
#4763=EDGE_CURVE('',#3749,#3747,#1870,.T.);
#4764=EDGE_CURVE('',#3751,#3752,#2513,.T.);
#4765=EDGE_CURVE('',#3752,#3750,#1871,.T.);
#4766=EDGE_CURVE('',#3751,#3749,#1872,.T.);
#4767=EDGE_CURVE('',#3753,#3754,#2514,.T.);
#4768=EDGE_CURVE('',#3754,#3752,#1873,.T.);
#4769=EDGE_CURVE('',#3753,#3751,#1874,.T.);
#4770=EDGE_CURVE('',#3755,#3756,#2515,.T.);
#4771=EDGE_CURVE('',#3756,#3754,#1875,.T.);
#4772=EDGE_CURVE('',#3755,#3753,#1876,.T.);
#4773=EDGE_CURVE('',#3757,#3758,#2516,.T.);
#4774=EDGE_CURVE('',#3758,#3756,#1877,.T.);
#4775=EDGE_CURVE('',#3757,#3755,#1878,.T.);
#4776=EDGE_CURVE('',#3759,#3760,#2517,.T.);
#4777=EDGE_CURVE('',#3760,#3758,#1879,.T.);
#4778=EDGE_CURVE('',#3759,#3757,#1880,.T.);
#4779=EDGE_CURVE('',#3761,#3762,#2518,.T.);
#4780=EDGE_CURVE('',#3762,#3760,#1881,.T.);
#4781=EDGE_CURVE('',#3761,#3759,#1882,.T.);
#4782=EDGE_CURVE('',#3763,#3764,#2519,.T.);
#4783=EDGE_CURVE('',#3764,#3762,#1883,.T.);
#4784=EDGE_CURVE('',#3763,#3761,#1884,.T.);
#4785=EDGE_CURVE('',#3765,#3766,#2520,.T.);
#4786=EDGE_CURVE('',#3766,#3764,#1885,.T.);
#4787=EDGE_CURVE('',#3765,#3763,#1886,.T.);
#4788=EDGE_CURVE('',#3767,#3768,#2521,.T.);
#4789=EDGE_CURVE('',#3768,#3766,#1887,.T.);
#4790=EDGE_CURVE('',#3767,#3765,#1888,.T.);
#4791=EDGE_CURVE('',#3769,#3770,#2522,.T.);
#4792=EDGE_CURVE('',#3771,#3769,#1889,.T.);
#4793=EDGE_CURVE('',#3772,#3771,#1596,.T.);
#4794=EDGE_CURVE('',#3772,#3770,#1890,.T.);
#4795=EDGE_CURVE('',#3773,#3774,#2523,.T.);
#4796=EDGE_CURVE('',#3774,#3775,#1891,.T.);
#4797=EDGE_CURVE('',#3775,#3776,#1597,.T.);
#4798=EDGE_CURVE('',#3776,#3777,#1892,.T.);
#4799=EDGE_CURVE('',#3777,#3778,#2524,.T.);
#4800=EDGE_CURVE('',#3778,#3778,#1598,.F.);
#4801=EDGE_CURVE('',#3777,#3773,#1893,.T.);
#4802=EDGE_CURVE('',#3779,#3780,#2525,.T.);
#4803=EDGE_CURVE('',#3780,#3774,#1894,.T.);
#4804=EDGE_CURVE('',#3773,#3779,#1895,.T.);
#4805=EDGE_CURVE('',#3781,#3782,#2526,.T.);
#4806=EDGE_CURVE('',#3782,#3780,#1896,.T.);
#4807=EDGE_CURVE('',#3779,#3781,#1897,.T.);
#4808=EDGE_CURVE('',#3783,#3784,#2527,.T.);
#4809=EDGE_CURVE('',#3784,#3782,#1898,.T.);
#4810=EDGE_CURVE('',#3781,#3783,#1899,.T.);
#4811=EDGE_CURVE('',#3785,#3786,#2528,.T.);
#4812=EDGE_CURVE('',#3786,#3784,#1900,.T.);
#4813=EDGE_CURVE('',#3783,#3785,#1901,.T.);
#4814=EDGE_CURVE('',#3787,#3788,#2529,.T.);
#4815=EDGE_CURVE('',#3788,#3786,#1902,.T.);
#4816=EDGE_CURVE('',#3785,#3787,#1903,.T.);
#4817=EDGE_CURVE('',#3789,#3790,#2530,.T.);
#4818=EDGE_CURVE('',#3790,#3788,#1904,.T.);
#4819=EDGE_CURVE('',#3787,#3789,#1905,.T.);
#4820=EDGE_CURVE('',#3791,#3792,#2531,.T.);
#4821=EDGE_CURVE('',#3792,#3790,#1906,.T.);
#4822=EDGE_CURVE('',#3789,#3791,#1907,.T.);
#4823=EDGE_CURVE('',#3793,#3794,#2532,.T.);
#4824=EDGE_CURVE('',#3794,#3792,#1908,.T.);
#4825=EDGE_CURVE('',#3791,#3793,#1909,.T.);
#4826=EDGE_CURVE('',#3795,#3796,#2533,.T.);
#4827=EDGE_CURVE('',#3796,#3794,#1910,.T.);
#4828=EDGE_CURVE('',#3793,#3795,#1911,.T.);
#4829=EDGE_CURVE('',#3797,#3798,#2534,.T.);
#4830=EDGE_CURVE('',#3798,#3796,#1912,.T.);
#4831=EDGE_CURVE('',#3795,#3797,#1913,.T.);
#4832=EDGE_CURVE('',#3799,#3800,#2535,.T.);
#4833=EDGE_CURVE('',#3799,#3801,#1914,.T.);
#4834=EDGE_CURVE('',#3802,#3801,#1599,.T.);
#4835=EDGE_CURVE('',#3802,#3800,#1915,.T.);
#4836=EDGE_CURVE('',#3803,#3804,#2536,.T.);
#4837=EDGE_CURVE('',#3804,#3805,#1916,.T.);
#4838=EDGE_CURVE('',#3806,#3805,#1600,.T.);
#4839=EDGE_CURVE('',#3803,#3806,#1917,.T.);
#4840=EDGE_CURVE('',#3807,#3808,#2537,.T.);
#4841=EDGE_CURVE('',#3808,#3804,#1918,.T.);
#4842=EDGE_CURVE('',#3807,#3803,#1919,.T.);
#4843=EDGE_CURVE('',#3809,#3810,#2538,.T.);
#4844=EDGE_CURVE('',#3810,#3808,#1920,.T.);
#4845=EDGE_CURVE('',#3809,#3807,#1921,.T.);
#4846=EDGE_CURVE('',#3811,#3812,#2539,.T.);
#4847=EDGE_CURVE('',#3812,#3810,#1922,.T.);
#4848=EDGE_CURVE('',#3811,#3809,#1923,.T.);
#4849=EDGE_CURVE('',#3813,#3814,#2540,.T.);
#4850=EDGE_CURVE('',#3814,#3812,#1924,.T.);
#4851=EDGE_CURVE('',#3813,#3811,#1925,.T.);
#4852=EDGE_CURVE('',#3815,#3816,#2541,.T.);
#4853=EDGE_CURVE('',#3816,#3814,#1926,.T.);
#4854=EDGE_CURVE('',#3815,#3813,#1927,.T.);
#4855=EDGE_CURVE('',#3817,#3818,#2542,.T.);
#4856=EDGE_CURVE('',#3818,#3816,#1928,.T.);
#4857=EDGE_CURVE('',#3817,#3815,#1929,.T.);
#4858=EDGE_CURVE('',#3819,#3820,#2543,.T.);
#4859=EDGE_CURVE('',#3820,#3818,#1930,.T.);
#4860=EDGE_CURVE('',#3819,#3817,#1931,.T.);
#4861=EDGE_CURVE('',#3821,#3822,#2544,.T.);
#4862=EDGE_CURVE('',#3822,#3820,#1932,.T.);
#4863=EDGE_CURVE('',#3821,#3819,#1933,.T.);
#4864=EDGE_CURVE('',#3823,#3824,#2545,.T.);
#4865=EDGE_CURVE('',#3824,#3822,#1934,.T.);
#4866=EDGE_CURVE('',#3823,#3821,#1935,.T.);
#4867=EDGE_CURVE('',#3825,#3826,#2546,.T.);
#4868=EDGE_CURVE('',#3826,#3824,#1936,.T.);
#4869=EDGE_CURVE('',#3825,#3823,#1937,.T.);
#4870=EDGE_CURVE('',#3827,#3828,#2547,.T.);
#4871=EDGE_CURVE('',#3828,#3826,#1938,.T.);
#4872=EDGE_CURVE('',#3827,#3825,#1939,.T.);
#4873=EDGE_CURVE('',#3829,#3830,#2548,.T.);
#4874=EDGE_CURVE('',#3831,#3829,#1940,.T.);
#4875=EDGE_CURVE('',#3832,#3831,#1601,.T.);
#4876=EDGE_CURVE('',#3832,#3830,#1941,.T.);
#4877=EDGE_CURVE('',#3833,#3834,#1602,.T.);
#4878=EDGE_CURVE('',#3833,#3835,#2549,.T.);
#4879=EDGE_CURVE('',#3835,#3836,#1603,.T.);
#4880=EDGE_CURVE('',#3836,#3834,#2550,.T.);
#4881=EDGE_CURVE('',#3833,#3837,#2551,.T.);
#4882=EDGE_CURVE('',#3838,#3837,#2552,.T.);
#4883=EDGE_CURVE('',#3835,#3838,#2553,.T.);
#4884=EDGE_CURVE('',#3839,#3837,#1604,.T.);
#4885=EDGE_CURVE('',#3839,#3840,#2554,.T.);
#4886=EDGE_CURVE('',#3840,#3838,#1605,.T.);
#4887=EDGE_CURVE('',#3839,#3841,#2555,.T.);
#4888=EDGE_CURVE('',#3842,#3841,#2556,.T.);
#4889=EDGE_CURVE('',#3840,#3842,#2557,.T.);
#4890=EDGE_CURVE('',#3843,#3844,#1606,.T.);
#4891=EDGE_CURVE('',#3843,#3845,#2558,.T.);
#4892=EDGE_CURVE('',#3845,#3846,#1607,.T.);
#4893=EDGE_CURVE('',#3846,#3844,#2559,.T.);
#4894=EDGE_CURVE('',#3843,#3834,#2560,.T.);
#4895=EDGE_CURVE('',#3847,#3844,#2561,.T.);
#4896=EDGE_CURVE('',#3847,#3841,#1608,.T.);
#4897=EDGE_CURVE('',#3848,#3848,#1609,.T.);
#4898=EDGE_CURVE('',#3849,#3849,#1610,.T.);
#4899=EDGE_CURVE('',#3850,#3850,#1611,.T.);
#4900=EDGE_CURVE('',#3851,#3846,#2562,.T.);
#4901=EDGE_CURVE('',#3847,#3851,#2563,.T.);
#4902=EDGE_CURVE('',#3852,#3852,#1612,.T.);
#4903=EDGE_CURVE('',#3851,#3842,#1613,.T.);
#4904=EDGE_CURVE('',#3853,#3853,#1614,.T.);
#4905=EDGE_CURVE('',#3853,#3852,#2564,.T.);
#4906=EDGE_CURVE('',#3854,#3854,#1615,.T.);
#4907=EDGE_CURVE('',#3855,#3855,#1616,.T.);
#4908=EDGE_CURVE('',#3856,#3856,#1617,.T.);
#4909=EDGE_CURVE('',#3856,#3854,#2565,.T.);
#4910=EDGE_CURVE('',#3855,#3850,#2566,.T.);
#4911=EDGE_CURVE('',#3857,#3857,#1618,.T.);
#4912=EDGE_CURVE('',#3858,#3858,#1619,.T.);
#4913=EDGE_CURVE('',#3859,#3859,#1620,.T.);
#4914=EDGE_CURVE('',#3859,#3857,#2567,.T.);
#4915=EDGE_CURVE('',#3858,#3849,#2568,.T.);
#4916=EDGE_CURVE('',#3775,#3806,#1942,.T.);
#4917=EDGE_CURVE('',#3805,#3776,#1943,.T.);
#4918=EDGE_CURVE('',#3830,#3828,#1944,.T.);
#4919=EDGE_CURVE('',#3829,#3827,#1945,.T.);
#4920=EDGE_CURVE('',#3801,#3832,#1946,.T.);
#4921=EDGE_CURVE('',#3797,#3799,#1947,.T.);
#4922=EDGE_CURVE('',#3800,#3798,#1948,.T.);
#4923=EDGE_CURVE('',#3831,#3802,#1949,.T.);
#4924=EDGE_CURVE('',#3715,#3746,#1950,.T.);
#4925=EDGE_CURVE('',#3745,#3716,#1951,.T.);
#4926=EDGE_CURVE('',#3770,#3768,#1952,.T.);
#4927=EDGE_CURVE('',#3769,#3767,#1953,.T.);
#4928=EDGE_CURVE('',#3741,#3772,#1954,.T.);
#4929=EDGE_CURVE('',#3737,#3739,#1955,.T.);
#4930=EDGE_CURVE('',#3740,#3738,#1956,.T.);
#4931=EDGE_CURVE('',#3771,#3742,#1957,.T.);
#4932=EDGE_CURVE('',#3655,#3686,#1958,.T.);
#4933=EDGE_CURVE('',#3685,#3656,#1959,.T.);
#4934=EDGE_CURVE('',#3710,#3708,#1960,.T.);
#4935=EDGE_CURVE('',#3709,#3707,#1961,.T.);
#4936=EDGE_CURVE('',#3681,#3712,#1962,.T.);
#4937=EDGE_CURVE('',#3677,#3679,#1963,.T.);
#4938=EDGE_CURVE('',#3680,#3678,#1964,.T.);
#4939=EDGE_CURVE('',#3711,#3682,#1965,.T.);
#4940=EDGE_CURVE('',#3595,#3626,#1966,.T.);
#4941=EDGE_CURVE('',#3625,#3596,#1967,.T.);
#4942=EDGE_CURVE('',#3650,#3648,#1968,.T.);
#4943=EDGE_CURVE('',#3649,#3647,#1969,.T.);
#4944=EDGE_CURVE('',#3621,#3652,#1970,.T.);
#4945=EDGE_CURVE('',#3617,#3619,#1971,.T.);
#4946=EDGE_CURVE('',#3620,#3618,#1972,.T.);
#4947=EDGE_CURVE('',#3651,#3622,#1973,.T.);
#4948=EDGE_CURVE('',#3860,#3860,#1621,.T.);
#4949=EDGE_CURVE('',#3860,#3861,#2569,.T.);
#4950=EDGE_CURVE('',#3861,#3861,#1622,.T.);
#4951=EDGE_CURVE('',#3862,#3862,#1623,.T.);
#4952=EDGE_CURVE('',#3862,#3863,#2570,.T.);
#4953=EDGE_CURVE('',#3863,#3863,#1624,.T.);
#4954=EDGE_CURVE('',#3864,#3865,#2571,.T.);
#4955=EDGE_CURVE('',#3866,#3865,#2572,.T.);
#4956=EDGE_CURVE('',#3867,#3866,#2573,.T.);
#4957=EDGE_CURVE('',#3864,#3867,#2574,.T.);
#4958=EDGE_CURVE('',#3868,#3864,#2575,.T.);
#4959=EDGE_CURVE('',#3869,#3867,#2576,.T.);
#4960=EDGE_CURVE('',#3868,#3869,#2577,.T.);
#4961=EDGE_CURVE('',#3870,#3868,#2578,.T.);
#4962=EDGE_CURVE('',#3871,#3869,#2579,.T.);
#4963=EDGE_CURVE('',#3870,#3871,#2580,.T.);
#4964=EDGE_CURVE('',#3871,#3866,#2581,.T.);
#4965=EDGE_CURVE('',#3872,#3873,#2582,.T.);
#4966=EDGE_CURVE('',#3873,#3874,#2583,.T.);
#4967=EDGE_CURVE('',#3875,#3874,#2584,.T.);
#4968=EDGE_CURVE('',#3872,#3875,#2585,.T.);
#4969=EDGE_CURVE('',#3876,#3877,#2586,.T.);
#4970=EDGE_CURVE('',#3878,#3877,#2587,.T.);
#4971=EDGE_CURVE('',#3879,#3878,#2588,.T.);
#4972=EDGE_CURVE('',#3876,#3879,#2589,.T.);
#4973=EDGE_CURVE('',#3873,#3876,#2590,.T.);
#4974=EDGE_CURVE('',#3874,#3879,#2591,.T.);
#4975=EDGE_CURVE('',#3875,#3878,#2592,.T.);
#4976=EDGE_CURVE('',#3880,#3880,#1625,.T.);
#4977=EDGE_CURVE('',#3880,#3881,#2593,.T.);
#4978=EDGE_CURVE('',#3881,#3881,#1626,.T.);
#4979=EDGE_CURVE('',#3882,#3882,#1627,.T.);
#4980=EDGE_CURVE('',#3882,#3848,#2594,.T.);
#4981=EDGE_CURVE('',#3845,#3836,#2595,.T.);
#4982=EDGE_CURVE('',#3883,#3884,#2596,.T.);
#4983=EDGE_CURVE('',#3884,#3885,#2597,.T.);
#4984=EDGE_CURVE('',#3886,#3885,#2598,.T.);
#4985=EDGE_CURVE('',#3883,#3886,#2599,.T.);
#4986=EDGE_CURVE('',#3865,#3883,#2600,.T.);
#4987=EDGE_CURVE('',#3887,#3886,#2601,.T.);
#4988=EDGE_CURVE('',#3888,#3887,#2602,.T.);
#4989=EDGE_CURVE('',#3888,#3870,#2603,.T.);
#4990=EDGE_CURVE('',#3889,#3888,#2604,.T.);
#4991=EDGE_CURVE('',#3890,#3887,#2605,.T.);
#4992=EDGE_CURVE('',#3889,#3890,#2606,.T.);
#4993=EDGE_CURVE('',#3877,#3889,#2607,.T.);
#4994=EDGE_CURVE('',#3885,#3890,#2608,.T.);
#4995=EDGE_CURVE('',#3884,#3872,#2609,.T.);
#4996=EDGE_CURVE('',#3891,#3891,#1628,.T.);
#4997=EDGE_CURVE('',#3891,#3892,#2610,.T.);
#4998=EDGE_CURVE('',#3892,#3892,#1629,.T.);
#4999=EDGE_CURVE('',#3893,#3893,#1630,.T.);
#5000=EDGE_CURVE('',#3893,#3894,#2611,.T.);
#5001=EDGE_CURVE('',#3894,#3894,#1631,.T.);
#5002=EDGE_CURVE('',#3895,#3895,#1632,.T.);
#5003=EDGE_CURVE('',#3895,#3896,#2612,.T.);
#5004=EDGE_CURVE('',#3896,#3896,#1633,.T.);
#5005=EDGE_CURVE('',#3897,#3897,#1634,.T.);
#5006=EDGE_CURVE('',#3897,#3898,#2613,.T.);
#5007=EDGE_CURVE('',#3898,#3898,#1635,.T.);
#5008=EDGE_CURVE('',#3899,#3899,#1636,.T.);
#5009=EDGE_CURVE('',#3899,#3900,#2614,.T.);
#5010=EDGE_CURVE('',#3900,#3900,#1637,.T.);
#5011=EDGE_CURVE('',#3901,#3902,#2615,.T.);
#5012=EDGE_CURVE('',#3902,#3903,#2616,.T.);
#5013=EDGE_CURVE('',#3904,#3903,#2617,.T.);
#5014=EDGE_CURVE('',#3901,#3904,#2618,.T.);
#5015=EDGE_CURVE('',#3905,#3901,#2619,.T.);
#5016=EDGE_CURVE('',#3906,#3904,#2620,.T.);
#5017=EDGE_CURVE('',#3905,#3906,#2621,.T.);
#5018=EDGE_CURVE('',#3907,#3905,#2622,.T.);
#5019=EDGE_CURVE('',#3908,#3906,#2623,.T.);
#5020=EDGE_CURVE('',#3907,#3908,#2624,.T.);
#5021=EDGE_CURVE('',#3902,#3907,#2625,.T.);
#5022=EDGE_CURVE('',#3903,#3908,#2626,.T.);
#5023=EDGE_CURVE('',#3909,#3909,#1638,.T.);
#5024=EDGE_CURVE('',#3910,#3910,#1639,.T.);
#5025=EDGE_CURVE('',#3909,#3911,#2627,.T.);
#5026=EDGE_CURVE('',#3911,#3911,#1640,.T.);
#5027=EDGE_CURVE('',#3912,#3912,#1641,.T.);
#5028=EDGE_CURVE('',#3913,#3913,#1642,.T.);
#5029=EDGE_CURVE('',#3913,#3912,#2628,.T.);
#5030=EDGE_CURVE('',#3914,#3914,#1643,.T.);
#5031=EDGE_CURVE('',#3914,#3910,#2629,.T.);
#5032=EDGE_CURVE('',#3915,#3916,#2630,.T.);
#5033=EDGE_CURVE('',#3916,#3917,#1974,.T.);
#5034=EDGE_CURVE('',#3918,#3917,#1644,.F.);
#5035=EDGE_CURVE('',#3918,#3915,#1975,.T.);
#5036=EDGE_CURVE('',#3919,#3920,#2631,.T.);
#5037=EDGE_CURVE('',#3920,#3916,#1976,.T.);
#5038=EDGE_CURVE('',#3915,#3919,#1977,.T.);
#5039=EDGE_CURVE('',#3921,#3922,#2632,.T.);
#5040=EDGE_CURVE('',#3922,#3920,#1978,.T.);
#5041=EDGE_CURVE('',#3919,#3921,#1979,.T.);
#5042=EDGE_CURVE('',#3923,#3924,#2633,.T.);
#5043=EDGE_CURVE('',#3924,#3922,#1980,.T.);
#5044=EDGE_CURVE('',#3921,#3923,#1981,.T.);
#5045=EDGE_CURVE('',#3925,#3926,#2634,.T.);
#5046=EDGE_CURVE('',#3926,#3924,#1982,.T.);
#5047=EDGE_CURVE('',#3923,#3925,#1983,.T.);
#5048=EDGE_CURVE('',#3927,#3928,#2635,.T.);
#5049=EDGE_CURVE('',#3928,#3926,#1984,.T.);
#5050=EDGE_CURVE('',#3925,#3927,#1985,.T.);
#5051=EDGE_CURVE('',#3929,#3930,#2636,.T.);
#5052=EDGE_CURVE('',#3930,#3928,#1986,.T.);
#5053=EDGE_CURVE('',#3927,#3929,#1987,.T.);
#5054=EDGE_CURVE('',#3931,#3932,#2637,.T.);
#5055=EDGE_CURVE('',#3931,#3933,#1988,.T.);
#5056=EDGE_CURVE('',#3934,#3933,#1645,.T.);
#5057=EDGE_CURVE('',#3934,#3932,#1989,.T.);
#5058=EDGE_CURVE('',#3935,#3936,#2638,.T.);
#5059=EDGE_CURVE('',#3936,#3937,#1990,.T.);
#5060=EDGE_CURVE('',#3938,#3937,#1646,.F.);
#5061=EDGE_CURVE('',#3938,#3935,#1991,.T.);
#5062=EDGE_CURVE('',#3939,#3940,#2639,.T.);
#5063=EDGE_CURVE('',#3940,#3936,#1992,.T.);
#5064=EDGE_CURVE('',#3935,#3939,#1993,.T.);
#5065=EDGE_CURVE('',#3941,#3942,#2640,.T.);
#5066=EDGE_CURVE('',#3942,#3940,#1994,.T.);
#5067=EDGE_CURVE('',#3939,#3941,#1995,.T.);
#5068=EDGE_CURVE('',#3943,#3944,#2641,.T.);
#5069=EDGE_CURVE('',#3944,#3942,#1996,.T.);
#5070=EDGE_CURVE('',#3941,#3943,#1997,.T.);
#5071=EDGE_CURVE('',#3945,#3946,#2642,.T.);
#5072=EDGE_CURVE('',#3946,#3944,#1998,.T.);
#5073=EDGE_CURVE('',#3943,#3945,#1999,.T.);
#5074=EDGE_CURVE('',#3947,#3948,#2643,.T.);
#5075=EDGE_CURVE('',#3948,#3946,#2000,.T.);
#5076=EDGE_CURVE('',#3945,#3947,#2001,.T.);
#5077=EDGE_CURVE('',#3949,#3950,#2644,.T.);
#5078=EDGE_CURVE('',#3950,#3948,#2002,.T.);
#5079=EDGE_CURVE('',#3947,#3949,#2003,.T.);
#5080=EDGE_CURVE('',#3951,#3952,#2645,.T.);
#5081=EDGE_CURVE('',#3951,#3953,#2004,.T.);
#5082=EDGE_CURVE('',#3954,#3953,#1647,.T.);
#5083=EDGE_CURVE('',#3954,#3952,#2005,.T.);
#5084=EDGE_CURVE('',#3955,#3956,#2646,.T.);
#5085=EDGE_CURVE('',#3956,#3957,#2006,.T.);
#5086=EDGE_CURVE('',#3958,#3957,#1648,.T.);
#5087=EDGE_CURVE('',#3955,#3958,#2007,.T.);
#5088=EDGE_CURVE('',#3959,#3960,#2647,.T.);
#5089=EDGE_CURVE('',#3960,#3956,#2008,.T.);
#5090=EDGE_CURVE('',#3959,#3955,#2009,.T.);
#5091=EDGE_CURVE('',#3961,#3962,#2648,.T.);
#5092=EDGE_CURVE('',#3962,#3960,#2010,.T.);
#5093=EDGE_CURVE('',#3961,#3959,#2011,.T.);
#5094=EDGE_CURVE('',#3963,#3964,#2649,.T.);
#5095=EDGE_CURVE('',#3964,#3962,#2012,.T.);
#5096=EDGE_CURVE('',#3963,#3961,#2013,.T.);
#5097=EDGE_CURVE('',#3965,#3966,#2650,.T.);
#5098=EDGE_CURVE('',#3966,#3964,#2014,.T.);
#5099=EDGE_CURVE('',#3965,#3963,#2015,.T.);
#5100=EDGE_CURVE('',#3967,#3968,#2651,.T.);
#5101=EDGE_CURVE('',#3968,#3966,#2016,.T.);
#5102=EDGE_CURVE('',#3967,#3965,#2017,.T.);
#5103=EDGE_CURVE('',#3969,#3970,#2652,.T.);
#5104=EDGE_CURVE('',#3970,#3968,#2018,.T.);
#5105=EDGE_CURVE('',#3969,#3967,#2019,.T.);
#5106=EDGE_CURVE('',#3971,#3972,#2653,.T.);
#5107=EDGE_CURVE('',#3973,#3971,#2020,.T.);
#5108=EDGE_CURVE('',#3974,#3973,#1649,.T.);
#5109=EDGE_CURVE('',#3974,#3972,#2021,.T.);
#5110=EDGE_CURVE('',#3975,#3976,#2654,.T.);
#5111=EDGE_CURVE('',#3976,#3977,#2022,.T.);
#5112=EDGE_CURVE('',#3978,#3977,#1650,.T.);
#5113=EDGE_CURVE('',#3975,#3978,#2023,.T.);
#5114=EDGE_CURVE('',#3979,#3980,#2655,.T.);
#5115=EDGE_CURVE('',#3980,#3976,#2024,.T.);
#5116=EDGE_CURVE('',#3979,#3975,#2025,.T.);
#5117=EDGE_CURVE('',#3981,#3982,#2656,.T.);
#5118=EDGE_CURVE('',#3982,#3980,#2026,.T.);
#5119=EDGE_CURVE('',#3981,#3979,#2027,.T.);
#5120=EDGE_CURVE('',#3983,#3984,#2657,.T.);
#5121=EDGE_CURVE('',#3984,#3982,#2028,.T.);
#5122=EDGE_CURVE('',#3983,#3981,#2029,.T.);
#5123=EDGE_CURVE('',#3985,#3986,#2658,.T.);
#5124=EDGE_CURVE('',#3986,#3984,#2030,.T.);
#5125=EDGE_CURVE('',#3985,#3983,#2031,.T.);
#5126=EDGE_CURVE('',#3987,#3988,#2659,.T.);
#5127=EDGE_CURVE('',#3988,#3986,#2032,.T.);
#5128=EDGE_CURVE('',#3987,#3985,#2033,.T.);
#5129=EDGE_CURVE('',#3989,#3990,#2660,.T.);
#5130=EDGE_CURVE('',#3990,#3988,#2034,.T.);
#5131=EDGE_CURVE('',#3989,#3987,#2035,.T.);
#5132=EDGE_CURVE('',#3991,#3992,#2661,.T.);
#5133=EDGE_CURVE('',#3993,#3991,#2036,.T.);
#5134=EDGE_CURVE('',#3994,#3993,#1651,.T.);
#5135=EDGE_CURVE('',#3994,#3992,#2037,.T.);
#5136=EDGE_CURVE('',#3992,#3990,#2038,.T.);
#5137=EDGE_CURVE('',#3991,#3989,#2039,.T.);
#5138=EDGE_CURVE('',#3977,#3938,#2040,.T.);
#5139=EDGE_CURVE('',#3953,#3994,#2041,.T.);
#5140=EDGE_CURVE('',#3949,#3951,#2042,.T.);
#5141=EDGE_CURVE('',#3937,#3978,#2043,.T.);
#5142=EDGE_CURVE('',#3952,#3950,#2044,.T.);
#5143=EDGE_CURVE('',#3993,#3954,#2045,.T.);
#5144=EDGE_CURVE('',#3995,#3996,#1652,.T.);
#5145=EDGE_CURVE('',#3997,#3995,#2662,.T.);
#5146=EDGE_CURVE('',#3998,#3997,#2663,.T.);
#5147=EDGE_CURVE('',#3999,#3998,#2664,.T.);
#5148=EDGE_CURVE('',#4000,#3999,#2665,.T.);
#5149=EDGE_CURVE('',#3996,#4000,#2666,.T.);
#5150=EDGE_CURVE('',#3917,#3958,#2046,.T.);
#5151=EDGE_CURVE('',#3957,#3918,#2047,.T.);
#5152=EDGE_CURVE('',#3972,#3970,#2048,.T.);
#5153=EDGE_CURVE('',#3971,#3969,#2049,.T.);
#5154=EDGE_CURVE('',#3933,#3974,#2050,.T.);
#5155=EDGE_CURVE('',#3929,#3931,#2051,.T.);
#5156=EDGE_CURVE('',#3932,#3930,#2052,.T.);
#5157=EDGE_CURVE('',#3973,#3934,#2053,.T.);
#5158=EDGE_CURVE('',#4001,#4001,#1653,.T.);
#5159=EDGE_CURVE('',#4001,#4002,#2667,.T.);
#5160=EDGE_CURVE('',#4002,#4002,#1654,.T.);
#5161=EDGE_CURVE('',#4003,#4003,#1655,.T.);
#5162=EDGE_CURVE('',#4003,#4004,#2668,.T.);
#5163=EDGE_CURVE('',#4004,#4004,#1656,.T.);
#5164=EDGE_CURVE('',#4005,#4006,#2669,.T.);
#5165=EDGE_CURVE('',#4005,#4007,#2670,.T.);
#5166=EDGE_CURVE('',#4008,#4007,#2671,.T.);
#5167=EDGE_CURVE('',#4006,#4008,#2672,.T.);
#5168=EDGE_CURVE('',#4007,#4009,#2673,.T.);
#5169=EDGE_CURVE('',#4009,#4010,#2674,.T.);
#5170=EDGE_CURVE('',#4010,#4008,#2675,.T.);
#5171=EDGE_CURVE('',#4011,#4009,#2676,.T.);
#5172=EDGE_CURVE('',#4012,#4005,#2677,.T.);
#5173=EDGE_CURVE('',#4012,#4013,#2678,.T.);
#5174=EDGE_CURVE('',#4014,#4013,#2679,.T.);
#5175=EDGE_CURVE('',#4015,#4014,#2680,.T.);
#5176=EDGE_CURVE('',#4015,#4016,#2681,.T.);
#5177=EDGE_CURVE('',#4016,#4011,#2682,.T.);
#5178=EDGE_CURVE('',#4006,#4017,#2683,.T.);
#5179=EDGE_CURVE('',#4017,#4012,#2684,.T.);
#5180=EDGE_CURVE('',#4017,#4018,#2685,.T.);
#5181=EDGE_CURVE('',#4013,#4018,#2686,.T.);
#5182=EDGE_CURVE('',#4019,#4014,#2687,.T.);
#5183=EDGE_CURVE('',#4018,#4019,#2688,.T.);
#5184=EDGE_CURVE('',#4020,#4016,#1657,.T.);
#5185=EDGE_CURVE('',#4021,#4020,#2689,.T.);
#5186=EDGE_CURVE('',#4011,#4021,#2690,.T.);
#5187=EDGE_CURVE('',#4016,#4022,#1658,.T.);
#5188=EDGE_CURVE('',#4023,#4015,#2691,.T.);
#5189=EDGE_CURVE('',#4020,#4023,#2692,.T.);
#5190=EDGE_CURVE('',#4022,#4020,#1659,.T.);
#5191=EDGE_CURVE('',#4021,#4010,#2693,.T.);
#5192=EDGE_CURVE('',#4023,#4019,#2694,.T.);
#5193=EDGE_CURVE('',#3996,#4024,#2695,.T.);
#5194=EDGE_CURVE('',#4000,#4025,#2696,.T.);
#5195=EDGE_CURVE('',#4024,#4025,#2697,.T.);
#5196=EDGE_CURVE('',#3998,#4026,#2698,.T.);
#5197=EDGE_CURVE('',#4027,#4026,#2699,.T.);
#5198=EDGE_CURVE('',#3999,#4027,#2700,.T.);
#5199=EDGE_CURVE('',#4025,#4027,#2701,.T.);
#5200=EDGE_CURVE('',#4028,#3995,#2702,.T.);
#5201=EDGE_CURVE('',#4029,#4028,#2703,.T.);
#5202=EDGE_CURVE('',#3997,#4029,#2704,.T.);
#5203=EDGE_CURVE('',#4026,#4029,#2705,.T.);
#5204=EDGE_CURVE('',#4028,#4024,#1660,.T.);
#5205=EDGE_CURVE('',#4022,#4030,#2706,.T.);
#5206=EDGE_CURVE('',#4030,#4030,#1661,.T.);
#5207=EDGE_CURVE('',#4031,#4031,#1662,.T.);
#5208=EDGE_CURVE('',#4031,#4032,#2707,.T.);
#5209=EDGE_CURVE('',#4032,#4032,#1663,.T.);
#5210=EDGE_CURVE('',#4033,#4033,#1664,.T.);
#5211=EDGE_CURVE('',#4033,#4034,#2708,.T.);
#5212=EDGE_CURVE('',#4034,#4034,#1665,.T.);
#5213=EDGE_CURVE('',#4035,#4036,#2709,.T.);
#5214=EDGE_CURVE('',#4036,#4037,#2710,.T.);
#5215=EDGE_CURVE('',#4038,#4037,#2711,.T.);
#5216=EDGE_CURVE('',#4035,#4038,#2712,.T.);
#5217=EDGE_CURVE('',#4039,#4035,#2713,.T.);
#5218=EDGE_CURVE('',#4040,#4038,#2714,.T.);
#5219=EDGE_CURVE('',#4039,#4040,#2715,.T.);
#5220=EDGE_CURVE('',#4041,#4039,#2716,.T.);
#5221=EDGE_CURVE('',#4042,#4040,#2717,.T.);
#5222=EDGE_CURVE('',#4041,#4042,#2718,.T.);
#5223=EDGE_CURVE('',#4036,#4041,#2719,.T.);
#5224=EDGE_CURVE('',#4037,#4042,#2720,.T.);
#5225=EDGE_CURVE('',#4043,#4043,#1666,.T.);
#5226=EDGE_CURVE('',#4043,#4044,#2721,.T.);
#5227=EDGE_CURVE('',#4044,#4044,#1667,.T.);
#5228=EDGE_CURVE('',#4045,#4045,#1668,.T.);
#5229=EDGE_CURVE('',#4045,#4043,#2722,.T.);
#5230=EDGE_CURVE('',#4046,#4046,#1669,.T.);
#5231=EDGE_CURVE('',#4047,#4047,#1670,.T.);
#5232=EDGE_CURVE('',#4047,#4045,#2723,.T.);
#5233=EDGE_CURVE('',#4048,#4048,#1671,.T.);
#5234=EDGE_CURVE('',#4049,#4049,#1672,.T.);
#5235=EDGE_CURVE('',#4049,#4046,#2724,.T.);
#5236=EDGE_CURVE('',#4050,#4050,#1673,.T.);
#5237=EDGE_CURVE('',#4050,#4049,#2725,.T.);
#5238=EDGE_CURVE('',#4048,#4050,#2726,.T.);
#5239=EDGE_CURVE('',#4051,#4052,#2727,.T.);
#5240=EDGE_CURVE('',#4052,#4053,#2054,.T.);
#5241=EDGE_CURVE('',#4053,#4054,#1674,.T.);
#5242=EDGE_CURVE('',#4054,#4055,#2055,.T.);
#5243=EDGE_CURVE('',#4055,#4056,#2728,.T.);
#5244=EDGE_CURVE('',#4056,#4056,#1675,.F.);
#5245=EDGE_CURVE('',#4055,#4051,#2056,.T.);
#5246=EDGE_CURVE('',#4057,#4058,#2729,.T.);
#5247=EDGE_CURVE('',#4058,#4052,#2057,.T.);
#5248=EDGE_CURVE('',#4051,#4057,#2058,.T.);
#5249=EDGE_CURVE('',#4059,#4060,#2730,.T.);
#5250=EDGE_CURVE('',#4060,#4058,#2059,.T.);
#5251=EDGE_CURVE('',#4057,#4059,#2060,.T.);
#5252=EDGE_CURVE('',#4061,#4062,#2731,.T.);
#5253=EDGE_CURVE('',#4062,#4060,#2061,.T.);
#5254=EDGE_CURVE('',#4059,#4061,#2062,.T.);
#5255=EDGE_CURVE('',#4063,#4064,#2732,.T.);
#5256=EDGE_CURVE('',#4064,#4062,#2063,.T.);
#5257=EDGE_CURVE('',#4061,#4063,#2064,.T.);
#5258=EDGE_CURVE('',#4065,#4066,#2733,.T.);
#5259=EDGE_CURVE('',#4066,#4064,#2065,.T.);
#5260=EDGE_CURVE('',#4063,#4065,#2066,.T.);
#5261=EDGE_CURVE('',#4067,#4068,#2734,.T.);
#5262=EDGE_CURVE('',#4068,#4066,#2067,.T.);
#5263=EDGE_CURVE('',#4065,#4067,#2068,.T.);
#5264=EDGE_CURVE('',#4069,#4070,#2735,.T.);
#5265=EDGE_CURVE('',#4070,#4068,#2069,.T.);
#5266=EDGE_CURVE('',#4067,#4069,#2070,.T.);
#5267=EDGE_CURVE('',#4071,#4072,#2736,.T.);
#5268=EDGE_CURVE('',#4072,#4070,#2071,.T.);
#5269=EDGE_CURVE('',#4069,#4071,#2072,.T.);
#5270=EDGE_CURVE('',#4073,#4074,#2737,.T.);
#5271=EDGE_CURVE('',#4074,#4072,#2073,.T.);
#5272=EDGE_CURVE('',#4071,#4073,#2074,.T.);
#5273=EDGE_CURVE('',#4075,#4076,#2738,.T.);
#5274=EDGE_CURVE('',#4076,#4074,#2075,.T.);
#5275=EDGE_CURVE('',#4073,#4075,#2076,.T.);
#5276=EDGE_CURVE('',#4077,#4078,#2739,.T.);
#5277=EDGE_CURVE('',#4077,#4079,#2077,.T.);
#5278=EDGE_CURVE('',#4080,#4079,#1676,.F.);
#5279=EDGE_CURVE('',#4080,#4078,#2078,.T.);
#5280=EDGE_CURVE('',#4081,#4082,#2740,.T.);
#5281=EDGE_CURVE('',#4082,#4083,#2079,.T.);
#5282=EDGE_CURVE('',#4084,#4083,#1677,.T.);
#5283=EDGE_CURVE('',#4081,#4084,#2080,.T.);
#5284=EDGE_CURVE('',#4085,#4086,#2741,.T.);
#5285=EDGE_CURVE('',#4086,#4082,#2081,.T.);
#5286=EDGE_CURVE('',#4085,#4081,#2082,.T.);
#5287=EDGE_CURVE('',#4087,#4088,#2742,.T.);
#5288=EDGE_CURVE('',#4088,#4086,#2083,.T.);
#5289=EDGE_CURVE('',#4087,#4085,#2084,.T.);
#5290=EDGE_CURVE('',#4089,#4090,#2743,.T.);
#5291=EDGE_CURVE('',#4090,#4088,#2085,.T.);
#5292=EDGE_CURVE('',#4089,#4087,#2086,.T.);
#5293=EDGE_CURVE('',#4091,#4092,#2744,.T.);
#5294=EDGE_CURVE('',#4092,#4090,#2087,.T.);
#5295=EDGE_CURVE('',#4091,#4089,#2088,.T.);
#5296=EDGE_CURVE('',#4093,#4094,#2745,.T.);
#5297=EDGE_CURVE('',#4094,#4092,#2089,.T.);
#5298=EDGE_CURVE('',#4093,#4091,#2090,.T.);
#5299=EDGE_CURVE('',#4095,#4096,#2746,.T.);
#5300=EDGE_CURVE('',#4096,#4094,#2091,.T.);
#5301=EDGE_CURVE('',#4095,#4093,#2092,.T.);
#5302=EDGE_CURVE('',#4097,#4098,#2747,.T.);
#5303=EDGE_CURVE('',#4098,#4096,#2093,.T.);
#5304=EDGE_CURVE('',#4097,#4095,#2094,.T.);
#5305=EDGE_CURVE('',#4099,#4100,#2748,.T.);
#5306=EDGE_CURVE('',#4100,#4098,#2095,.T.);
#5307=EDGE_CURVE('',#4099,#4097,#2096,.T.);
#5308=EDGE_CURVE('',#4101,#4102,#2749,.T.);
#5309=EDGE_CURVE('',#4102,#4100,#2097,.T.);
#5310=EDGE_CURVE('',#4101,#4099,#2098,.T.);
#5311=EDGE_CURVE('',#4103,#4104,#2750,.T.);
#5312=EDGE_CURVE('',#4104,#4102,#2099,.T.);
#5313=EDGE_CURVE('',#4103,#4101,#2100,.T.);
#5314=EDGE_CURVE('',#4105,#4106,#2751,.T.);
#5315=EDGE_CURVE('',#4106,#4104,#2101,.T.);
#5316=EDGE_CURVE('',#4105,#4103,#2102,.T.);
#5317=EDGE_CURVE('',#4107,#4108,#2752,.T.);
#5318=EDGE_CURVE('',#4109,#4107,#2103,.T.);
#5319=EDGE_CURVE('',#4110,#4109,#1678,.T.);
#5320=EDGE_CURVE('',#4110,#4108,#2104,.T.);
#5321=EDGE_CURVE('',#4111,#4112,#2753,.T.);
#5322=EDGE_CURVE('',#4112,#4113,#2105,.T.);
#5323=EDGE_CURVE('',#4113,#4114,#1679,.T.);
#5324=EDGE_CURVE('',#4114,#4115,#2754,.T.);
#5325=EDGE_CURVE('',#4115,#4115,#1680,.F.);
#5326=EDGE_CURVE('',#4114,#4116,#1681,.T.);
#5327=EDGE_CURVE('',#4116,#4111,#2106,.T.);
#5328=EDGE_CURVE('',#4117,#4118,#2755,.T.);
#5329=EDGE_CURVE('',#4118,#4112,#2107,.T.);
#5330=EDGE_CURVE('',#4111,#4117,#2108,.T.);
#5331=EDGE_CURVE('',#4119,#4120,#2756,.T.);
#5332=EDGE_CURVE('',#4120,#4118,#2109,.T.);
#5333=EDGE_CURVE('',#4117,#4119,#2110,.T.);
#5334=EDGE_CURVE('',#4121,#4122,#2757,.T.);
#5335=EDGE_CURVE('',#4122,#4120,#2111,.T.);
#5336=EDGE_CURVE('',#4119,#4121,#2112,.T.);
#5337=EDGE_CURVE('',#4123,#4124,#2758,.T.);
#5338=EDGE_CURVE('',#4124,#4122,#2113,.T.);
#5339=EDGE_CURVE('',#4121,#4123,#2114,.T.);
#5340=EDGE_CURVE('',#4125,#4126,#2759,.T.);
#5341=EDGE_CURVE('',#4126,#4124,#2115,.T.);
#5342=EDGE_CURVE('',#4123,#4125,#2116,.T.);
#5343=EDGE_CURVE('',#4127,#4128,#2760,.T.);
#5344=EDGE_CURVE('',#4128,#4126,#2117,.T.);
#5345=EDGE_CURVE('',#4125,#4127,#2118,.T.);
#5346=EDGE_CURVE('',#4129,#4130,#2761,.T.);
#5347=EDGE_CURVE('',#4130,#4128,#2119,.T.);
#5348=EDGE_CURVE('',#4127,#4129,#2120,.T.);
#5349=EDGE_CURVE('',#4131,#4132,#2762,.T.);
#5350=EDGE_CURVE('',#4132,#4130,#2121,.T.);
#5351=EDGE_CURVE('',#4129,#4131,#2122,.T.);
#5352=EDGE_CURVE('',#4133,#4134,#2763,.T.);
#5353=EDGE_CURVE('',#4134,#4132,#2123,.T.);
#5354=EDGE_CURVE('',#4131,#4133,#2124,.T.);
#5355=EDGE_CURVE('',#4135,#4136,#2764,.T.);
#5356=EDGE_CURVE('',#4136,#4134,#2125,.T.);
#5357=EDGE_CURVE('',#4133,#4135,#2126,.T.);
#5358=EDGE_CURVE('',#4137,#4138,#2765,.T.);
#5359=EDGE_CURVE('',#4138,#4136,#2127,.T.);
#5360=EDGE_CURVE('',#4135,#4137,#2128,.T.);
#5361=EDGE_CURVE('',#4139,#4140,#2766,.T.);
#5362=EDGE_CURVE('',#4140,#4138,#2129,.T.);
#5363=EDGE_CURVE('',#4137,#4139,#2130,.T.);
#5364=EDGE_CURVE('',#4141,#4142,#2767,.T.);
#5365=EDGE_CURVE('',#4142,#4140,#2131,.T.);
#5366=EDGE_CURVE('',#4139,#4141,#2132,.T.);
#5367=EDGE_CURVE('',#4143,#4144,#2768,.T.);
#5368=EDGE_CURVE('',#4144,#4142,#2133,.T.);
#5369=EDGE_CURVE('',#4141,#4143,#2134,.T.);
#5370=EDGE_CURVE('',#4145,#4146,#2769,.T.);
#5371=EDGE_CURVE('',#4146,#4144,#2135,.T.);
#5372=EDGE_CURVE('',#4143,#4145,#2136,.T.);
#5373=EDGE_CURVE('',#4147,#4148,#2770,.T.);
#5374=EDGE_CURVE('',#4148,#4146,#2137,.T.);
#5375=EDGE_CURVE('',#4145,#4147,#2138,.T.);
#5376=EDGE_CURVE('',#4149,#4150,#2771,.T.);
#5377=EDGE_CURVE('',#4149,#4151,#2139,.T.);
#5378=EDGE_CURVE('',#4152,#4151,#1682,.T.);
#5379=EDGE_CURVE('',#4152,#4150,#2140,.T.);
#5380=EDGE_CURVE('',#4153,#4154,#2772,.T.);
#5381=EDGE_CURVE('',#4154,#4155,#2141,.T.);
#5382=EDGE_CURVE('',#4156,#4155,#1683,.T.);
#5383=EDGE_CURVE('',#4153,#4156,#2142,.T.);
#5384=EDGE_CURVE('',#4157,#4158,#2773,.T.);
#5385=EDGE_CURVE('',#4158,#4154,#2143,.T.);
#5386=EDGE_CURVE('',#4157,#4153,#2144,.T.);
#5387=EDGE_CURVE('',#4159,#4160,#2774,.T.);
#5388=EDGE_CURVE('',#4160,#4158,#2145,.T.);
#5389=EDGE_CURVE('',#4159,#4157,#2146,.T.);
#5390=EDGE_CURVE('',#4161,#4162,#2775,.T.);
#5391=EDGE_CURVE('',#4162,#4160,#2147,.T.);
#5392=EDGE_CURVE('',#4161,#4159,#2148,.T.);
#5393=EDGE_CURVE('',#4163,#4164,#2776,.T.);
#5394=EDGE_CURVE('',#4164,#4162,#2149,.T.);
#5395=EDGE_CURVE('',#4163,#4161,#2150,.T.);
#5396=EDGE_CURVE('',#4165,#4166,#2777,.T.);
#5397=EDGE_CURVE('',#4166,#4164,#2151,.T.);
#5398=EDGE_CURVE('',#4165,#4163,#2152,.T.);
#5399=EDGE_CURVE('',#4167,#4168,#2778,.T.);
#5400=EDGE_CURVE('',#4168,#4166,#2153,.T.);
#5401=EDGE_CURVE('',#4167,#4165,#2154,.T.);
#5402=EDGE_CURVE('',#4169,#4170,#2779,.T.);
#5403=EDGE_CURVE('',#4170,#4168,#2155,.T.);
#5404=EDGE_CURVE('',#4169,#4167,#2156,.T.);
#5405=EDGE_CURVE('',#4171,#4172,#2780,.T.);
#5406=EDGE_CURVE('',#4172,#4170,#2157,.T.);
#5407=EDGE_CURVE('',#4171,#4169,#2158,.T.);
#5408=EDGE_CURVE('',#4173,#4174,#2781,.T.);
#5409=EDGE_CURVE('',#4174,#4172,#2159,.T.);
#5410=EDGE_CURVE('',#4173,#4171,#2160,.T.);
#5411=EDGE_CURVE('',#4175,#4176,#2782,.T.);
#5412=EDGE_CURVE('',#4176,#4174,#2161,.T.);
#5413=EDGE_CURVE('',#4175,#4173,#2162,.T.);
#5414=EDGE_CURVE('',#4177,#4178,#2783,.T.);
#5415=EDGE_CURVE('',#4178,#4176,#2163,.T.);
#5416=EDGE_CURVE('',#4177,#4175,#2164,.T.);
#5417=EDGE_CURVE('',#4179,#4180,#2784,.T.);
#5418=EDGE_CURVE('',#4180,#4178,#2165,.T.);
#5419=EDGE_CURVE('',#4179,#4177,#2166,.T.);
#5420=EDGE_CURVE('',#4181,#4182,#2785,.T.);
#5421=EDGE_CURVE('',#4182,#4180,#2167,.T.);
#5422=EDGE_CURVE('',#4181,#4179,#2168,.T.);
#5423=EDGE_CURVE('',#4183,#4184,#2786,.T.);
#5424=EDGE_CURVE('',#4184,#4182,#2169,.T.);
#5425=EDGE_CURVE('',#4183,#4181,#2170,.T.);
#5426=EDGE_CURVE('',#4185,#4186,#2787,.T.);
#5427=EDGE_CURVE('',#4186,#4184,#2171,.T.);
#5428=EDGE_CURVE('',#4185,#4183,#2172,.T.);
#5429=EDGE_CURVE('',#4187,#4188,#2788,.T.);
#5430=EDGE_CURVE('',#4188,#4186,#2173,.T.);
#5431=EDGE_CURVE('',#4187,#4185,#2174,.T.);
#5432=EDGE_CURVE('',#4189,#4190,#2789,.T.);
#5433=EDGE_CURVE('',#4191,#4189,#2175,.T.);
#5434=EDGE_CURVE('',#4192,#4191,#1684,.T.);
#5435=EDGE_CURVE('',#4192,#4190,#2176,.T.);
#5436=EDGE_CURVE('',#4113,#4156,#2177,.T.);
#5437=EDGE_CURVE('',#4155,#4116,#2178,.T.);
#5438=EDGE_CURVE('',#4190,#4188,#2179,.T.);
#5439=EDGE_CURVE('',#4189,#4187,#2180,.T.);
#5440=EDGE_CURVE('',#4151,#4192,#2181,.T.);
#5441=EDGE_CURVE('',#4147,#4149,#2182,.T.);
#5442=EDGE_CURVE('',#4150,#4148,#2183,.T.);
#5443=EDGE_CURVE('',#4191,#4152,#2184,.T.);
#5444=EDGE_CURVE('',#4053,#4084,#2185,.T.);
#5445=EDGE_CURVE('',#4083,#4054,#2186,.T.);
#5446=EDGE_CURVE('',#4108,#4106,#2187,.T.);
#5447=EDGE_CURVE('',#4107,#4105,#2188,.T.);
#5448=EDGE_CURVE('',#4079,#4110,#2189,.T.);
#5449=EDGE_CURVE('',#4075,#4077,#2190,.T.);
#5450=EDGE_CURVE('',#4078,#4076,#2191,.T.);
#5451=EDGE_CURVE('',#4109,#4080,#2192,.T.);
#5452=EDGE_CURVE('',#4193,#4194,#2790,.T.);
#5453=EDGE_CURVE('',#4194,#4195,#2791,.T.);
#5454=EDGE_CURVE('',#4196,#4195,#2792,.T.);
#5455=EDGE_CURVE('',#4193,#4196,#2793,.T.);
#5456=EDGE_CURVE('',#4197,#4193,#2794,.T.);
#5457=EDGE_CURVE('',#4198,#4196,#2795,.T.);
#5458=EDGE_CURVE('',#4197,#4198,#2796,.T.);
#5459=EDGE_CURVE('',#4199,#4197,#2797,.T.);
#5460=EDGE_CURVE('',#4200,#4198,#2798,.T.);
#5461=EDGE_CURVE('',#4199,#4200,#2799,.T.);
#5462=EDGE_CURVE('',#4194,#4199,#2800,.T.);
#5463=EDGE_CURVE('',#4195,#4200,#2801,.T.);
#5464=EDGE_CURVE('',#4201,#4202,#2802,.T.);
#5465=EDGE_CURVE('',#4202,#4203,#2193,.T.);
#5466=EDGE_CURVE('',#4203,#4204,#1685,.T.);
#5467=EDGE_CURVE('',#4204,#4205,#2803,.T.);
#5468=EDGE_CURVE('',#4205,#4205,#1686,.F.);
#5469=EDGE_CURVE('',#4204,#4206,#1687,.T.);
#5470=EDGE_CURVE('',#4206,#4201,#2194,.T.);
#5471=EDGE_CURVE('',#4207,#4208,#2804,.T.);
#5472=EDGE_CURVE('',#4208,#4202,#2195,.T.);
#5473=EDGE_CURVE('',#4201,#4207,#2196,.T.);
#5474=EDGE_CURVE('',#4209,#4210,#2805,.T.);
#5475=EDGE_CURVE('',#4210,#4208,#2197,.T.);
#5476=EDGE_CURVE('',#4207,#4209,#2198,.T.);
#5477=EDGE_CURVE('',#4211,#4212,#2806,.T.);
#5478=EDGE_CURVE('',#4212,#4210,#2199,.T.);
#5479=EDGE_CURVE('',#4209,#4211,#2200,.T.);
#5480=EDGE_CURVE('',#4213,#4214,#2807,.T.);
#5481=EDGE_CURVE('',#4214,#4212,#2201,.T.);
#5482=EDGE_CURVE('',#4211,#4213,#2202,.T.);
#5483=EDGE_CURVE('',#4215,#4216,#2808,.T.);
#5484=EDGE_CURVE('',#4216,#4214,#2203,.T.);
#5485=EDGE_CURVE('',#4213,#4215,#2204,.T.);
#5486=EDGE_CURVE('',#4217,#4218,#2809,.T.);
#5487=EDGE_CURVE('',#4218,#4216,#2205,.T.);
#5488=EDGE_CURVE('',#4215,#4217,#2206,.T.);
#5489=EDGE_CURVE('',#4219,#4220,#2810,.T.);
#5490=EDGE_CURVE('',#4220,#4218,#2207,.T.);
#5491=EDGE_CURVE('',#4217,#4219,#2208,.T.);
#5492=EDGE_CURVE('',#4221,#4222,#2811,.T.);
#5493=EDGE_CURVE('',#4222,#4220,#2209,.T.);
#5494=EDGE_CURVE('',#4219,#4221,#2210,.T.);
#5495=EDGE_CURVE('',#4223,#4224,#2812,.T.);
#5496=EDGE_CURVE('',#4223,#4225,#2211,.T.);
#5497=EDGE_CURVE('',#4226,#4225,#1688,.T.);
#5498=EDGE_CURVE('',#4226,#4224,#2212,.T.);
#5499=EDGE_CURVE('',#4227,#4228,#2813,.T.);
#5500=EDGE_CURVE('',#4228,#4229,#2213,.T.);
#5501=EDGE_CURVE('',#4230,#4229,#1689,.T.);
#5502=EDGE_CURVE('',#4227,#4230,#2214,.T.);
#5503=EDGE_CURVE('',#4231,#4232,#2814,.T.);
#5504=EDGE_CURVE('',#4232,#4228,#2215,.T.);
#5505=EDGE_CURVE('',#4231,#4227,#2216,.T.);
#5506=EDGE_CURVE('',#4233,#4234,#2815,.T.);
#5507=EDGE_CURVE('',#4234,#4232,#2217,.T.);
#5508=EDGE_CURVE('',#4233,#4231,#2218,.T.);
#5509=EDGE_CURVE('',#4235,#4236,#2816,.T.);
#5510=EDGE_CURVE('',#4236,#4234,#2219,.T.);
#5511=EDGE_CURVE('',#4235,#4233,#2220,.T.);
#5512=EDGE_CURVE('',#4237,#4238,#2817,.T.);
#5513=EDGE_CURVE('',#4238,#4236,#2221,.T.);
#5514=EDGE_CURVE('',#4237,#4235,#2222,.T.);
#5515=EDGE_CURVE('',#4239,#4240,#2818,.T.);
#5516=EDGE_CURVE('',#4240,#4238,#2223,.T.);
#5517=EDGE_CURVE('',#4239,#4237,#2224,.T.);
#5518=EDGE_CURVE('',#4241,#4242,#2819,.T.);
#5519=EDGE_CURVE('',#4242,#4240,#2225,.T.);
#5520=EDGE_CURVE('',#4241,#4239,#2226,.T.);
#5521=EDGE_CURVE('',#4243,#4244,#2820,.T.);
#5522=EDGE_CURVE('',#4244,#4242,#2227,.T.);
#5523=EDGE_CURVE('',#4243,#4241,#2228,.T.);
#5524=EDGE_CURVE('',#4245,#4246,#2821,.T.);
#5525=EDGE_CURVE('',#4246,#4244,#2229,.T.);
#5526=EDGE_CURVE('',#4245,#4243,#2230,.T.);
#5527=EDGE_CURVE('',#4247,#4248,#2822,.T.);
#5528=EDGE_CURVE('',#4249,#4247,#2231,.T.);
#5529=EDGE_CURVE('',#4250,#4249,#1690,.T.);
#5530=EDGE_CURVE('',#4250,#4248,#2232,.T.);
#5531=EDGE_CURVE('',#4203,#4230,#2233,.T.);
#5532=EDGE_CURVE('',#4229,#4206,#2234,.T.);
#5533=EDGE_CURVE('',#4248,#4246,#2235,.T.);
#5534=EDGE_CURVE('',#4247,#4245,#2236,.T.);
#5535=EDGE_CURVE('',#4225,#4250,#2237,.T.);
#5536=EDGE_CURVE('',#4221,#4223,#2238,.T.);
#5537=EDGE_CURVE('',#4224,#4222,#2239,.T.);
#5538=EDGE_CURVE('',#4249,#4226,#2240,.T.);
#5539=EDGE_CURVE('',#4251,#4251,#1691,.T.);
#5540=EDGE_CURVE('',#4251,#4252,#2823,.T.);
#5541=EDGE_CURVE('',#4252,#4252,#1692,.T.);
#5542=EDGE_CURVE('',#4253,#4254,#2824,.T.);
#5543=EDGE_CURVE('',#4254,#4255,#2825,.T.);
#5544=EDGE_CURVE('',#4256,#4255,#2826,.T.);
#5545=EDGE_CURVE('',#4253,#4256,#2827,.T.);
#5546=EDGE_CURVE('',#4257,#4258,#2828,.T.);
#5547=EDGE_CURVE('',#4254,#4257,#2829,.T.);
#5548=EDGE_CURVE('',#4258,#4253,#2830,.T.);
#5549=EDGE_CURVE('',#4255,#4259,#2831,.T.);
#5550=EDGE_CURVE('',#4260,#4257,#2832,.T.);
#5551=EDGE_CURVE('',#4260,#4261,#2833,.T.);
#5552=EDGE_CURVE('',#4261,#4259,#2834,.T.);
#5553=EDGE_CURVE('',#4262,#4258,#2835,.T.);
#5554=EDGE_CURVE('',#4262,#4260,#2836,.T.);
#5555=EDGE_CURVE('',#4263,#4256,#2837,.T.);
#5556=EDGE_CURVE('',#4264,#4263,#2838,.T.);
#5557=EDGE_CURVE('',#4264,#4262,#2839,.T.);
#5558=EDGE_CURVE('',#4261,#4264,#2840,.T.);
#5559=EDGE_CURVE('',#4259,#4263,#2841,.T.);
#5560=EDGE_CURVE('',#4265,#4265,#1693,.T.);
#5561=EDGE_CURVE('',#4265,#4266,#2842,.T.);
#5562=EDGE_CURVE('',#4266,#4266,#1694,.T.);
#5563=EDGE_CURVE('',#4267,#4268,#2843,.T.);
#5564=EDGE_CURVE('',#4268,#4269,#2844,.T.);
#5565=EDGE_CURVE('',#4270,#4269,#2845,.T.);
#5566=EDGE_CURVE('',#4267,#4270,#2846,.T.);
#5567=EDGE_CURVE('',#4271,#4267,#2847,.T.);
#5568=EDGE_CURVE('',#4272,#4270,#2848,.T.);
#5569=EDGE_CURVE('',#4271,#4272,#2849,.T.);
#5570=EDGE_CURVE('',#4273,#4271,#2850,.T.);
#5571=EDGE_CURVE('',#4274,#4272,#2851,.T.);
#5572=EDGE_CURVE('',#4273,#4274,#2852,.T.);
#5573=EDGE_CURVE('',#4268,#4273,#2853,.T.);
#5574=EDGE_CURVE('',#4269,#4274,#2854,.T.);
#5575=EDGE_CURVE('',#4275,#4275,#1695,.T.);
#5576=EDGE_CURVE('',#4275,#4276,#2855,.T.);
#5577=EDGE_CURVE('',#4276,#4276,#1696,.T.);
#5578=EDGE_CURVE('',#4277,#4277,#1697,.T.);
#5579=EDGE_CURVE('',#4277,#4278,#2856,.T.);
#5580=EDGE_CURVE('',#4278,#4278,#1698,.T.);
#5581=EDGE_CURVE('',#4279,#4279,#1699,.T.);
#5582=EDGE_CURVE('',#4279,#4280,#2857,.T.);
#5583=EDGE_CURVE('',#4280,#4280,#1700,.T.);
#5584=EDGE_CURVE('',#4281,#4281,#1701,.T.);
#5585=EDGE_CURVE('',#4282,#4282,#1702,.T.);
#5586=EDGE_CURVE('',#4283,#4283,#1703,.T.);
#5587=EDGE_CURVE('',#4283,#4282,#2858,.T.);
#5588=EDGE_CURVE('',#4284,#4284,#1704,.T.);
#5589=EDGE_CURVE('',#4285,#4285,#1705,.T.);
#5590=EDGE_CURVE('',#4284,#4286,#2859,.T.);
#5591=EDGE_CURVE('',#4286,#4286,#1706,.T.);
#5592=EDGE_CURVE('',#4281,#4285,#2860,.T.);
#5593=EDGE_CURVE('',#4287,#4288,#2861,.T.);
#5594=EDGE_CURVE('',#4289,#4287,#2862,.T.);
#5595=EDGE_CURVE('',#4290,#4289,#2863,.T.);
#5596=EDGE_CURVE('',#4288,#4290,#2864,.T.);
#5597=EDGE_CURVE('',#4291,#4292,#2865,.T.);
#5598=EDGE_CURVE('',#4293,#4291,#2866,.T.);
#5599=EDGE_CURVE('',#4294,#4293,#2867,.T.);
#5600=EDGE_CURVE('',#4292,#4294,#2868,.T.);
#5601=EDGE_CURVE('',#4289,#4294,#1707,.T.);
#5602=EDGE_CURVE('',#4292,#4287,#1708,.T.);
#5603=EDGE_CURVE('',#4291,#4288,#1709,.T.);
#5604=EDGE_CURVE('',#4290,#4293,#1710,.T.);
#5605=EDGE_CURVE('',#4295,#4295,#1711,.T.);
#5606=EDGE_CURVE('',#4295,#4296,#2241,.T.);
#5607=EDGE_CURVE('',#4296,#4296,#1712,.T.);
#5608=EDGE_CURVE('',#4297,#4297,#1713,.T.);
#5609=EDGE_CURVE('',#4297,#4298,#2869,.T.);
#5610=EDGE_CURVE('',#4298,#4298,#1714,.T.);
#5611=EDGE_CURVE('',#4299,#4299,#1715,.T.);
#5612=EDGE_CURVE('',#4299,#4300,#2870,.T.);
#5613=EDGE_CURVE('',#4300,#4300,#1716,.T.);
#5614=EDGE_CURVE('',#4301,#4302,#2871,.T.);
#5615=EDGE_CURVE('',#4301,#4303,#2242,.T.);
#5616=EDGE_CURVE('',#4303,#4304,#1717,.F.);
#5617=EDGE_CURVE('',#4304,#4302,#2243,.T.);
#5618=EDGE_CURVE('',#4305,#4306,#2872,.T.);
#5619=EDGE_CURVE('',#4305,#4301,#2244,.T.);
#5620=EDGE_CURVE('',#4302,#4306,#2245,.T.);
#5621=EDGE_CURVE('',#4307,#4308,#2873,.T.);
#5622=EDGE_CURVE('',#4307,#4305,#2246,.T.);
#5623=EDGE_CURVE('',#4306,#4308,#2247,.T.);
#5624=EDGE_CURVE('',#4309,#4310,#2874,.T.);
#5625=EDGE_CURVE('',#4309,#4307,#2248,.T.);
#5626=EDGE_CURVE('',#4308,#4310,#2249,.T.);
#5627=EDGE_CURVE('',#4311,#4312,#2875,.T.);
#5628=EDGE_CURVE('',#4311,#4309,#2250,.T.);
#5629=EDGE_CURVE('',#4310,#4312,#2251,.T.);
#5630=EDGE_CURVE('',#4313,#4314,#2876,.T.);
#5631=EDGE_CURVE('',#4313,#4311,#2252,.T.);
#5632=EDGE_CURVE('',#4312,#4314,#2253,.T.);
#5633=EDGE_CURVE('',#4315,#4316,#2877,.T.);
#5634=EDGE_CURVE('',#4315,#4313,#2254,.T.);
#5635=EDGE_CURVE('',#4314,#4316,#2255,.T.);
#5636=EDGE_CURVE('',#4317,#4318,#2878,.T.);
#5637=EDGE_CURVE('',#4317,#4315,#2256,.T.);
#5638=EDGE_CURVE('',#4316,#4318,#2257,.T.);
#5639=EDGE_CURVE('',#4319,#4320,#2879,.T.);
#5640=EDGE_CURVE('',#4319,#4317,#2258,.T.);
#5641=EDGE_CURVE('',#4318,#4320,#2259,.T.);
#5642=EDGE_CURVE('',#4321,#4322,#2880,.T.);
#5643=EDGE_CURVE('',#4321,#4319,#2260,.T.);
#5644=EDGE_CURVE('',#4320,#4322,#2261,.T.);
#5645=EDGE_CURVE('',#4323,#4324,#2881,.T.);
#5646=EDGE_CURVE('',#4323,#4321,#2262,.T.);
#5647=EDGE_CURVE('',#4322,#4324,#2263,.T.);
#5648=EDGE_CURVE('',#4325,#4326,#2882,.T.);
#5649=EDGE_CURVE('',#4325,#4323,#2264,.T.);
#5650=EDGE_CURVE('',#4324,#4326,#2265,.T.);
#5651=EDGE_CURVE('',#4327,#4328,#2883,.T.);
#5652=EDGE_CURVE('',#4327,#4325,#2266,.T.);
#5653=EDGE_CURVE('',#4326,#4328,#2267,.T.);
#5654=EDGE_CURVE('',#4329,#4330,#2884,.T.);
#5655=EDGE_CURVE('',#4329,#4327,#2268,.T.);
#5656=EDGE_CURVE('',#4328,#4330,#2269,.T.);
#5657=EDGE_CURVE('',#4331,#4332,#2885,.T.);
#5658=EDGE_CURVE('',#4331,#4329,#2270,.T.);
#5659=EDGE_CURVE('',#4330,#4332,#2271,.T.);
#5660=EDGE_CURVE('',#4333,#4334,#2886,.T.);
#5661=EDGE_CURVE('',#4333,#4331,#2272,.T.);
#5662=EDGE_CURVE('',#4332,#4334,#2273,.T.);
#5663=EDGE_CURVE('',#4335,#4336,#2887,.T.);
#5664=EDGE_CURVE('',#4335,#4337,#2274,.T.);
#5665=EDGE_CURVE('',#4337,#4338,#1718,.T.);
#5666=EDGE_CURVE('',#4336,#4338,#2275,.T.);
#5667=EDGE_CURVE('',#4339,#4340,#2888,.T.);
#5668=EDGE_CURVE('',#4339,#4335,#2276,.T.);
#5669=EDGE_CURVE('',#4340,#4336,#2277,.T.);
#5670=EDGE_CURVE('',#4341,#4342,#2889,.T.);
#5671=EDGE_CURVE('',#4341,#4339,#2278,.T.);
#5672=EDGE_CURVE('',#4342,#4340,#2279,.T.);
#5673=EDGE_CURVE('',#4343,#4344,#2890,.T.);
#5674=EDGE_CURVE('',#4343,#4341,#2280,.T.);
#5675=EDGE_CURVE('',#4344,#4342,#2281,.T.);
#5676=EDGE_CURVE('',#4345,#4346,#2891,.T.);
#5677=EDGE_CURVE('',#4345,#4343,#2282,.T.);
#5678=EDGE_CURVE('',#4346,#4344,#2283,.T.);
#5679=EDGE_CURVE('',#4347,#4348,#2892,.T.);
#5680=EDGE_CURVE('',#4347,#4345,#2284,.T.);
#5681=EDGE_CURVE('',#4348,#4346,#2285,.T.);
#5682=EDGE_CURVE('',#4349,#4350,#2893,.T.);
#5683=EDGE_CURVE('',#4349,#4347,#2286,.T.);
#5684=EDGE_CURVE('',#4350,#4348,#2287,.T.);
#5685=EDGE_CURVE('',#4351,#4352,#2894,.T.);
#5686=EDGE_CURVE('',#4351,#4349,#2288,.T.);
#5687=EDGE_CURVE('',#4352,#4350,#2289,.T.);
#5688=EDGE_CURVE('',#4353,#4354,#2895,.T.);
#5689=EDGE_CURVE('',#4353,#4351,#2290,.T.);
#5690=EDGE_CURVE('',#4354,#4352,#2291,.T.);
#5691=EDGE_CURVE('',#4355,#4356,#2896,.T.);
#5692=EDGE_CURVE('',#4355,#4353,#2292,.T.);
#5693=EDGE_CURVE('',#4356,#4354,#2293,.T.);
#5694=EDGE_CURVE('',#4357,#4358,#2897,.T.);
#5695=EDGE_CURVE('',#4357,#4355,#2294,.T.);
#5696=EDGE_CURVE('',#4358,#4356,#2295,.T.);
#5697=EDGE_CURVE('',#4359,#4360,#2898,.T.);
#5698=EDGE_CURVE('',#4359,#4357,#2296,.T.);
#5699=EDGE_CURVE('',#4360,#4358,#2297,.T.);
#5700=EDGE_CURVE('',#4361,#4362,#2899,.T.);
#5701=EDGE_CURVE('',#4361,#4359,#2298,.T.);
#5702=EDGE_CURVE('',#4362,#4360,#2299,.T.);
#5703=EDGE_CURVE('',#4363,#4364,#2900,.T.);
#5704=EDGE_CURVE('',#4363,#4361,#2300,.T.);
#5705=EDGE_CURVE('',#4364,#4362,#2301,.T.);
#5706=EDGE_CURVE('',#4365,#4366,#2901,.T.);
#5707=EDGE_CURVE('',#4365,#4363,#2302,.T.);
#5708=EDGE_CURVE('',#4366,#4364,#2303,.T.);
#5709=EDGE_CURVE('',#4367,#4368,#2902,.T.);
#5710=EDGE_CURVE('',#4367,#4365,#2304,.T.);
#5711=EDGE_CURVE('',#4368,#4366,#2305,.T.);
#5712=EDGE_CURVE('',#4338,#4369,#2306,.T.);
#5713=EDGE_CURVE('',#4370,#4337,#2307,.T.);
#5714=EDGE_CURVE('',#4371,#4370,#1719,.T.);
#5715=EDGE_CURVE('',#4369,#4371,#2308,.T.);
#5716=EDGE_CURVE('',#4369,#4372,#2903,.T.);
#5717=EDGE_CURVE('',#4372,#4372,#1720,.T.);
#5718=EDGE_CURVE('',#4373,#4367,#2309,.T.);
#5719=EDGE_CURVE('',#4303,#4373,#2310,.T.);
#5720=EDGE_CURVE('',#4370,#4333,#2311,.T.);
#5721=EDGE_CURVE('',#4374,#4368,#2312,.T.);
#5722=EDGE_CURVE('',#4373,#4374,#1721,.T.);
#5723=EDGE_CURVE('',#4334,#4371,#2313,.T.);
#5724=EDGE_CURVE('',#4374,#4304,#2314,.T.);
#5725=EDGE_CURVE('',#4375,#4376,#2904,.T.);
#5726=EDGE_CURVE('',#4375,#4377,#2905,.T.);
#5727=EDGE_CURVE('',#4377,#4378,#2906,.T.);
#5728=EDGE_CURVE('',#4376,#4378,#2907,.T.);
#5729=EDGE_CURVE('',#4379,#4375,#2908,.T.);
#5730=EDGE_CURVE('',#4379,#4380,#2909,.T.);
#5731=EDGE_CURVE('',#4380,#4377,#2910,.T.);
#5732=EDGE_CURVE('',#4381,#4379,#2911,.T.);
#5733=EDGE_CURVE('',#4381,#4382,#2912,.T.);
#5734=EDGE_CURVE('',#4382,#4380,#2913,.T.);
#5735=EDGE_CURVE('',#4383,#4381,#2914,.T.);
#5736=EDGE_CURVE('',#4383,#4384,#2915,.T.);
#5737=EDGE_CURVE('',#4384,#4382,#2916,.T.);
#5738=EDGE_CURVE('',#4385,#4383,#2917,.T.);
#5739=EDGE_CURVE('',#4385,#4386,#2918,.T.);
#5740=EDGE_CURVE('',#4386,#4384,#2919,.T.);
#5741=EDGE_CURVE('',#4376,#4385,#2920,.T.);
#5742=EDGE_CURVE('',#4378,#4386,#2921,.T.);
#5743=EDGE_CURVE('',#4387,#4387,#1722,.T.);
#5744=EDGE_CURVE('',#4387,#4388,#2922,.T.);
#5745=EDGE_CURVE('',#4388,#4388,#1723,.T.);
#5746=EDGE_CURVE('',#4389,#4390,#2923,.T.);
#5747=EDGE_CURVE('',#4389,#4391,#2315,.T.);
#5748=EDGE_CURVE('',#4391,#4392,#1724,.F.);
#5749=EDGE_CURVE('',#4392,#4390,#2316,.T.);
#5750=EDGE_CURVE('',#4393,#4394,#2924,.T.);
#5751=EDGE_CURVE('',#4393,#4389,#2317,.T.);
#5752=EDGE_CURVE('',#4390,#4394,#2318,.T.);
#5753=EDGE_CURVE('',#4395,#4396,#2925,.T.);
#5754=EDGE_CURVE('',#4395,#4393,#2319,.T.);
#5755=EDGE_CURVE('',#4394,#4396,#2320,.T.);
#5756=EDGE_CURVE('',#4397,#4398,#2926,.T.);
#5757=EDGE_CURVE('',#4397,#4395,#2321,.T.);
#5758=EDGE_CURVE('',#4396,#4398,#2322,.T.);
#5759=EDGE_CURVE('',#4399,#4400,#2927,.T.);
#5760=EDGE_CURVE('',#4399,#4397,#2323,.T.);
#5761=EDGE_CURVE('',#4398,#4400,#2324,.T.);
#5762=EDGE_CURVE('',#4401,#4402,#2928,.T.);
#5763=EDGE_CURVE('',#4401,#4399,#2325,.T.);
#5764=EDGE_CURVE('',#4400,#4402,#2326,.T.);
#5765=EDGE_CURVE('',#4403,#4404,#2929,.T.);
#5766=EDGE_CURVE('',#4403,#4401,#2327,.T.);
#5767=EDGE_CURVE('',#4402,#4404,#2328,.T.);
#5768=EDGE_CURVE('',#4405,#4406,#2930,.T.);
#5769=EDGE_CURVE('',#4405,#4403,#2329,.T.);
#5770=EDGE_CURVE('',#4404,#4406,#2330,.T.);
#5771=EDGE_CURVE('',#4407,#4408,#2931,.T.);
#5772=EDGE_CURVE('',#4407,#4405,#2331,.T.);
#5773=EDGE_CURVE('',#4406,#4408,#2332,.T.);
#5774=EDGE_CURVE('',#4409,#4410,#2932,.T.);
#5775=EDGE_CURVE('',#4409,#4407,#2333,.T.);
#5776=EDGE_CURVE('',#4408,#4410,#2334,.T.);
#5777=EDGE_CURVE('',#4411,#4412,#2933,.T.);
#5778=EDGE_CURVE('',#4411,#4413,#2335,.T.);
#5779=EDGE_CURVE('',#4413,#4414,#1725,.T.);
#5780=EDGE_CURVE('',#4412,#4414,#2336,.T.);
#5781=EDGE_CURVE('',#4415,#4416,#2934,.T.);
#5782=EDGE_CURVE('',#4415,#4411,#2337,.T.);
#5783=EDGE_CURVE('',#4416,#4412,#2338,.T.);
#5784=EDGE_CURVE('',#4417,#4418,#2935,.T.);
#5785=EDGE_CURVE('',#4417,#4415,#2339,.T.);
#5786=EDGE_CURVE('',#4418,#4416,#2340,.T.);
#5787=EDGE_CURVE('',#4419,#4420,#2936,.T.);
#5788=EDGE_CURVE('',#4419,#4417,#2341,.T.);
#5789=EDGE_CURVE('',#4420,#4418,#2342,.T.);
#5790=EDGE_CURVE('',#4421,#4422,#2937,.T.);
#5791=EDGE_CURVE('',#4421,#4419,#2343,.T.);
#5792=EDGE_CURVE('',#4422,#4420,#2344,.T.);
#5793=EDGE_CURVE('',#4423,#4424,#2938,.T.);
#5794=EDGE_CURVE('',#4423,#4421,#2345,.T.);
#5795=EDGE_CURVE('',#4424,#4422,#2346,.T.);
#5796=EDGE_CURVE('',#4425,#4426,#2939,.T.);
#5797=EDGE_CURVE('',#4425,#4423,#2347,.T.);
#5798=EDGE_CURVE('',#4426,#4424,#2348,.T.);
#5799=EDGE_CURVE('',#4427,#4428,#2940,.T.);
#5800=EDGE_CURVE('',#4427,#4425,#2349,.T.);
#5801=EDGE_CURVE('',#4428,#4426,#2350,.T.);
#5802=EDGE_CURVE('',#4429,#4430,#2941,.T.);
#5803=EDGE_CURVE('',#4429,#4427,#2351,.T.);
#5804=EDGE_CURVE('',#4430,#4428,#2352,.T.);
#5805=EDGE_CURVE('',#4431,#4432,#2942,.T.);
#5806=EDGE_CURVE('',#4431,#4429,#2353,.T.);
#5807=EDGE_CURVE('',#4432,#4430,#2354,.T.);
#5808=EDGE_CURVE('',#4414,#4433,#2355,.T.);
#5809=EDGE_CURVE('',#4434,#4413,#2356,.T.);
#5810=EDGE_CURVE('',#4435,#4434,#1726,.T.);
#5811=EDGE_CURVE('',#4433,#4435,#2357,.T.);
#5812=EDGE_CURVE('',#4433,#4436,#2943,.T.);
#5813=EDGE_CURVE('',#4436,#4436,#1727,.T.);
#5814=EDGE_CURVE('',#4437,#4431,#2358,.T.);
#5815=EDGE_CURVE('',#4391,#4437,#2359,.T.);
#5816=EDGE_CURVE('',#4434,#4409,#2360,.T.);
#5817=EDGE_CURVE('',#4438,#4432,#2361,.T.);
#5818=EDGE_CURVE('',#4437,#4438,#1728,.T.);
#5819=EDGE_CURVE('',#4410,#4435,#2362,.T.);
#5820=EDGE_CURVE('',#4438,#4392,#2363,.T.);
#5821=EDGE_CURVE('',#4439,#4440,#2944,.T.);
#5822=EDGE_CURVE('',#4439,#4441,#2945,.T.);
#5823=EDGE_CURVE('',#4441,#4442,#2946,.T.);
#5824=EDGE_CURVE('',#4440,#4442,#2947,.T.);
#5825=EDGE_CURVE('',#4443,#4439,#2948,.T.);
#5826=EDGE_CURVE('',#4443,#4444,#2949,.T.);
#5827=EDGE_CURVE('',#4444,#4441,#2950,.T.);
#5828=EDGE_CURVE('',#4445,#4443,#2951,.T.);
#5829=EDGE_CURVE('',#4445,#4446,#2952,.T.);
#5830=EDGE_CURVE('',#4446,#4444,#2953,.T.);
#5831=EDGE_CURVE('',#4447,#4445,#2954,.T.);
#5832=EDGE_CURVE('',#4447,#4448,#2955,.T.);
#5833=EDGE_CURVE('',#4448,#4446,#2956,.T.);
#5834=EDGE_CURVE('',#4449,#4447,#2957,.T.);
#5835=EDGE_CURVE('',#4449,#4450,#2958,.T.);
#5836=EDGE_CURVE('',#4450,#4448,#2959,.T.);
#5837=EDGE_CURVE('',#4440,#4449,#2960,.T.);
#5838=EDGE_CURVE('',#4442,#4450,#2961,.T.);
#5839=EDGE_CURVE('',#4451,#4451,#1729,.T.);
#5840=EDGE_CURVE('',#4451,#4452,#2962,.T.);
#5841=EDGE_CURVE('',#4452,#4452,#1730,.T.);
#5842=EDGE_CURVE('',#4453,#4454,#2963,.T.);
#5843=EDGE_CURVE('',#4453,#4455,#2364,.T.);
#5844=EDGE_CURVE('',#4455,#4456,#1731,.F.);
#5845=EDGE_CURVE('',#4456,#4454,#2365,.T.);
#5846=EDGE_CURVE('',#4457,#4458,#2964,.T.);
#5847=EDGE_CURVE('',#4457,#4453,#2366,.T.);
#5848=EDGE_CURVE('',#4454,#4458,#2367,.T.);
#5849=EDGE_CURVE('',#4459,#4460,#2965,.T.);
#5850=EDGE_CURVE('',#4459,#4457,#2368,.T.);
#5851=EDGE_CURVE('',#4458,#4460,#2369,.T.);
#5852=EDGE_CURVE('',#4461,#4462,#2966,.T.);
#5853=EDGE_CURVE('',#4461,#4459,#2370,.T.);
#5854=EDGE_CURVE('',#4460,#4462,#2371,.T.);
#5855=EDGE_CURVE('',#4463,#4464,#2967,.T.);
#5856=EDGE_CURVE('',#4463,#4461,#2372,.T.);
#5857=EDGE_CURVE('',#4462,#4464,#2373,.T.);
#5858=EDGE_CURVE('',#4465,#4466,#2968,.T.);
#5859=EDGE_CURVE('',#4465,#4463,#2374,.T.);
#5860=EDGE_CURVE('',#4464,#4466,#2375,.T.);
#5861=EDGE_CURVE('',#4467,#4468,#2969,.T.);
#5862=EDGE_CURVE('',#4467,#4465,#2376,.T.);
#5863=EDGE_CURVE('',#4466,#4468,#2377,.T.);
#5864=EDGE_CURVE('',#4469,#4470,#2970,.T.);
#5865=EDGE_CURVE('',#4469,#4467,#2378,.T.);
#5866=EDGE_CURVE('',#4468,#4470,#2379,.T.);
#5867=EDGE_CURVE('',#4471,#4472,#2971,.T.);
#5868=EDGE_CURVE('',#4471,#4469,#2380,.T.);
#5869=EDGE_CURVE('',#4470,#4472,#2381,.T.);
#5870=EDGE_CURVE('',#4473,#4474,#2972,.T.);
#5871=EDGE_CURVE('',#4473,#4471,#2382,.T.);
#5872=EDGE_CURVE('',#4472,#4474,#2383,.T.);
#5873=EDGE_CURVE('',#4475,#4476,#2973,.T.);
#5874=EDGE_CURVE('',#4475,#4473,#2384,.T.);
#5875=EDGE_CURVE('',#4474,#4476,#2385,.T.);
#5876=EDGE_CURVE('',#4477,#4478,#2974,.T.);
#5877=EDGE_CURVE('',#4477,#4475,#2386,.T.);
#5878=EDGE_CURVE('',#4476,#4478,#2387,.T.);
#5879=EDGE_CURVE('',#4479,#4480,#2975,.T.);
#5880=EDGE_CURVE('',#4479,#4477,#2388,.T.);
#5881=EDGE_CURVE('',#4478,#4480,#2389,.T.);
#5882=EDGE_CURVE('',#4481,#4482,#2976,.T.);
#5883=EDGE_CURVE('',#4481,#4479,#2390,.T.);
#5884=EDGE_CURVE('',#4480,#4482,#2391,.T.);
#5885=EDGE_CURVE('',#4483,#4484,#2977,.T.);
#5886=EDGE_CURVE('',#4483,#4481,#2392,.T.);
#5887=EDGE_CURVE('',#4482,#4484,#2393,.T.);
#5888=EDGE_CURVE('',#4485,#4486,#2978,.T.);
#5889=EDGE_CURVE('',#4485,#4483,#2394,.T.);
#5890=EDGE_CURVE('',#4484,#4486,#2395,.T.);
#5891=EDGE_CURVE('',#4487,#4488,#2979,.T.);
#5892=EDGE_CURVE('',#4487,#4485,#2396,.T.);
#5893=EDGE_CURVE('',#4486,#4488,#2397,.T.);
#5894=EDGE_CURVE('',#4489,#4490,#2980,.T.);
#5895=EDGE_CURVE('',#4489,#4487,#2398,.T.);
#5896=EDGE_CURVE('',#4488,#4490,#2399,.T.);
#5897=EDGE_CURVE('',#4491,#4492,#2981,.T.);
#5898=EDGE_CURVE('',#4491,#4493,#2400,.T.);
#5899=EDGE_CURVE('',#4493,#4494,#1732,.T.);
#5900=EDGE_CURVE('',#4492,#4494,#2401,.T.);
#5901=EDGE_CURVE('',#4495,#4496,#2982,.T.);
#5902=EDGE_CURVE('',#4495,#4491,#2402,.T.);
#5903=EDGE_CURVE('',#4496,#4492,#2403,.T.);
#5904=EDGE_CURVE('',#4497,#4498,#2983,.T.);
#5905=EDGE_CURVE('',#4497,#4495,#2404,.T.);
#5906=EDGE_CURVE('',#4498,#4496,#2405,.T.);
#5907=EDGE_CURVE('',#4499,#4500,#2984,.T.);
#5908=EDGE_CURVE('',#4499,#4497,#2406,.T.);
#5909=EDGE_CURVE('',#4500,#4498,#2407,.T.);
#5910=EDGE_CURVE('',#4501,#4502,#2985,.T.);
#5911=EDGE_CURVE('',#4501,#4499,#2408,.T.);
#5912=EDGE_CURVE('',#4502,#4500,#2409,.T.);
#5913=EDGE_CURVE('',#4503,#4504,#2986,.T.);
#5914=EDGE_CURVE('',#4503,#4501,#2410,.T.);
#5915=EDGE_CURVE('',#4504,#4502,#2411,.T.);
#5916=EDGE_CURVE('',#4505,#4506,#2987,.T.);
#5917=EDGE_CURVE('',#4505,#4503,#2412,.T.);
#5918=EDGE_CURVE('',#4506,#4504,#2413,.T.);
#5919=EDGE_CURVE('',#4507,#4508,#2988,.T.);
#5920=EDGE_CURVE('',#4507,#4505,#2414,.T.);
#5921=EDGE_CURVE('',#4508,#4506,#2415,.T.);
#5922=EDGE_CURVE('',#4509,#4510,#2989,.T.);
#5923=EDGE_CURVE('',#4509,#4507,#2416,.T.);
#5924=EDGE_CURVE('',#4510,#4508,#2417,.T.);
#5925=EDGE_CURVE('',#4511,#4512,#2990,.T.);
#5926=EDGE_CURVE('',#4511,#4509,#2418,.T.);
#5927=EDGE_CURVE('',#4512,#4510,#2419,.T.);
#5928=EDGE_CURVE('',#4513,#4514,#2991,.T.);
#5929=EDGE_CURVE('',#4513,#4511,#2420,.T.);
#5930=EDGE_CURVE('',#4514,#4512,#2421,.T.);
#5931=EDGE_CURVE('',#4515,#4516,#2992,.T.);
#5932=EDGE_CURVE('',#4515,#4513,#2422,.T.);
#5933=EDGE_CURVE('',#4516,#4514,#2423,.T.);
#5934=EDGE_CURVE('',#4517,#4518,#2993,.T.);
#5935=EDGE_CURVE('',#4517,#4515,#2424,.T.);
#5936=EDGE_CURVE('',#4518,#4516,#2425,.T.);
#5937=EDGE_CURVE('',#4519,#4520,#2994,.T.);
#5938=EDGE_CURVE('',#4519,#4517,#2426,.T.);
#5939=EDGE_CURVE('',#4520,#4518,#2427,.T.);
#5940=EDGE_CURVE('',#4521,#4522,#2995,.T.);
#5941=EDGE_CURVE('',#4521,#4519,#2428,.T.);
#5942=EDGE_CURVE('',#4522,#4520,#2429,.T.);
#5943=EDGE_CURVE('',#4523,#4524,#2996,.T.);
#5944=EDGE_CURVE('',#4523,#4521,#2430,.T.);
#5945=EDGE_CURVE('',#4524,#4522,#2431,.T.);
#5946=EDGE_CURVE('',#4525,#4526,#2997,.T.);
#5947=EDGE_CURVE('',#4525,#4523,#2432,.T.);
#5948=EDGE_CURVE('',#4526,#4524,#2433,.T.);
#5949=EDGE_CURVE('',#4527,#4528,#2998,.T.);
#5950=EDGE_CURVE('',#4527,#4525,#2434,.T.);
#5951=EDGE_CURVE('',#4528,#4526,#2435,.T.);
#5952=EDGE_CURVE('',#4494,#4529,#2436,.T.);
#5953=EDGE_CURVE('',#4530,#4493,#2437,.T.);
#5954=EDGE_CURVE('',#4531,#4530,#1733,.T.);
#5955=EDGE_CURVE('',#4529,#4531,#2438,.T.);
#5956=EDGE_CURVE('',#4529,#4532,#2999,.T.);
#5957=EDGE_CURVE('',#4532,#4532,#1734,.T.);
#5958=EDGE_CURVE('',#4533,#4527,#2439,.T.);
#5959=EDGE_CURVE('',#4455,#4533,#2440,.T.);
#5960=EDGE_CURVE('',#4530,#4489,#2441,.T.);
#5961=EDGE_CURVE('',#4534,#4528,#2442,.T.);
#5962=EDGE_CURVE('',#4533,#4534,#1735,.T.);
#5963=EDGE_CURVE('',#4490,#4531,#2443,.T.);
#5964=EDGE_CURVE('',#4534,#4456,#2444,.T.);
#5965=EDGE_CURVE('',#4535,#4536,#3000,.T.);
#5966=EDGE_CURVE('',#4535,#4537,#3001,.T.);
#5967=EDGE_CURVE('',#4537,#4538,#3002,.T.);
#5968=EDGE_CURVE('',#4536,#4538,#3003,.T.);
#5969=EDGE_CURVE('',#4539,#4535,#3004,.T.);
#5970=EDGE_CURVE('',#4539,#4540,#3005,.T.);
#5971=EDGE_CURVE('',#4540,#4537,#3006,.T.);
#5972=EDGE_CURVE('',#4541,#4539,#3007,.T.);
#5973=EDGE_CURVE('',#4541,#4542,#3008,.T.);
#5974=EDGE_CURVE('',#4542,#4540,#3009,.T.);
#5975=EDGE_CURVE('',#4543,#4541,#3010,.T.);
#5976=EDGE_CURVE('',#4543,#4544,#3011,.T.);
#5977=EDGE_CURVE('',#4544,#4542,#3012,.T.);
#5978=EDGE_CURVE('',#4545,#4543,#3013,.T.);
#5979=EDGE_CURVE('',#4545,#4546,#3014,.T.);
#5980=EDGE_CURVE('',#4546,#4544,#3015,.T.);
#5981=EDGE_CURVE('',#4536,#4545,#3016,.T.);
#5982=EDGE_CURVE('',#4538,#4546,#3017,.T.);
#5983=EDGE_CURVE('',#4547,#4547,#1736,.T.);
#5984=EDGE_CURVE('',#4547,#4548,#3018,.T.);
#5985=EDGE_CURVE('',#4548,#4548,#1737,.T.);
#5986=ORIENTED_EDGE('',*,*,#4549,.T.);
#5987=ORIENTED_EDGE('',*,*,#4550,.T.);
#5988=ORIENTED_EDGE('',*,*,#4551,.T.);
#5989=ORIENTED_EDGE('',*,*,#4552,.T.);
#5990=ORIENTED_EDGE('',*,*,#4553,.T.);
#5991=ORIENTED_EDGE('',*,*,#4554,.T.);
#5992=ORIENTED_EDGE('',*,*,#4553,.F.);
#5993=ORIENTED_EDGE('',*,*,#4555,.T.);
#5994=ORIENTED_EDGE('',*,*,#4556,.T.);
#5995=ORIENTED_EDGE('',*,*,#4557,.T.);
#5996=ORIENTED_EDGE('',*,*,#4549,.F.);
#5997=ORIENTED_EDGE('',*,*,#4558,.T.);
#5998=ORIENTED_EDGE('',*,*,#4559,.T.);
#5999=ORIENTED_EDGE('',*,*,#4560,.T.);
#6000=ORIENTED_EDGE('',*,*,#4556,.F.);
#6001=ORIENTED_EDGE('',*,*,#4561,.T.);
#6002=ORIENTED_EDGE('',*,*,#4562,.T.);
#6003=ORIENTED_EDGE('',*,*,#4563,.T.);
#6004=ORIENTED_EDGE('',*,*,#4559,.F.);
#6005=ORIENTED_EDGE('',*,*,#4564,.T.);
#6006=ORIENTED_EDGE('',*,*,#4565,.T.);
#6007=ORIENTED_EDGE('',*,*,#4566,.T.);
#6008=ORIENTED_EDGE('',*,*,#4562,.F.);
#6009=ORIENTED_EDGE('',*,*,#4567,.T.);
#6010=ORIENTED_EDGE('',*,*,#4568,.T.);
#6011=ORIENTED_EDGE('',*,*,#4569,.T.);
#6012=ORIENTED_EDGE('',*,*,#4565,.F.);
#6013=ORIENTED_EDGE('',*,*,#4570,.T.);
#6014=ORIENTED_EDGE('',*,*,#4571,.T.);
#6015=ORIENTED_EDGE('',*,*,#4572,.T.);
#6016=ORIENTED_EDGE('',*,*,#4568,.F.);
#6017=ORIENTED_EDGE('',*,*,#4573,.T.);
#6018=ORIENTED_EDGE('',*,*,#4574,.T.);
#6019=ORIENTED_EDGE('',*,*,#4575,.T.);
#6020=ORIENTED_EDGE('',*,*,#4571,.F.);
#6021=ORIENTED_EDGE('',*,*,#4576,.T.);
#6022=ORIENTED_EDGE('',*,*,#4577,.T.);
#6023=ORIENTED_EDGE('',*,*,#4578,.T.);
#6024=ORIENTED_EDGE('',*,*,#4574,.F.);
#6025=ORIENTED_EDGE('',*,*,#4579,.T.);
#6026=ORIENTED_EDGE('',*,*,#4580,.T.);
#6027=ORIENTED_EDGE('',*,*,#4581,.T.);
#6028=ORIENTED_EDGE('',*,*,#4577,.F.);
#6029=ORIENTED_EDGE('',*,*,#4582,.T.);
#6030=ORIENTED_EDGE('',*,*,#4583,.T.);
#6031=ORIENTED_EDGE('',*,*,#4584,.T.);
#6032=ORIENTED_EDGE('',*,*,#4580,.F.);
#6033=ORIENTED_EDGE('',*,*,#4585,.T.);
#6034=ORIENTED_EDGE('',*,*,#4586,.F.);
#6035=ORIENTED_EDGE('',*,*,#4587,.T.);
#6036=ORIENTED_EDGE('',*,*,#4588,.F.);
#6037=ORIENTED_EDGE('',*,*,#4589,.T.);
#6038=ORIENTED_EDGE('',*,*,#4590,.T.);
#6039=ORIENTED_EDGE('',*,*,#4591,.T.);
#6040=ORIENTED_EDGE('',*,*,#4592,.F.);
#6041=ORIENTED_EDGE('',*,*,#4593,.F.);
#6042=ORIENTED_EDGE('',*,*,#4594,.T.);
#6043=ORIENTED_EDGE('',*,*,#4595,.T.);
#6044=ORIENTED_EDGE('',*,*,#4590,.F.);
#6045=ORIENTED_EDGE('',*,*,#4596,.F.);
#6046=ORIENTED_EDGE('',*,*,#4597,.T.);
#6047=ORIENTED_EDGE('',*,*,#4598,.T.);
#6048=ORIENTED_EDGE('',*,*,#4594,.F.);
#6049=ORIENTED_EDGE('',*,*,#4599,.F.);
#6050=ORIENTED_EDGE('',*,*,#4600,.T.);
#6051=ORIENTED_EDGE('',*,*,#4601,.T.);
#6052=ORIENTED_EDGE('',*,*,#4597,.F.);
#6053=ORIENTED_EDGE('',*,*,#4602,.F.);
#6054=ORIENTED_EDGE('',*,*,#4603,.T.);
#6055=ORIENTED_EDGE('',*,*,#4604,.T.);
#6056=ORIENTED_EDGE('',*,*,#4600,.F.);
#6057=ORIENTED_EDGE('',*,*,#4605,.F.);
#6058=ORIENTED_EDGE('',*,*,#4606,.T.);
#6059=ORIENTED_EDGE('',*,*,#4607,.T.);
#6060=ORIENTED_EDGE('',*,*,#4603,.F.);
#6061=ORIENTED_EDGE('',*,*,#4608,.F.);
#6062=ORIENTED_EDGE('',*,*,#4609,.T.);
#6063=ORIENTED_EDGE('',*,*,#4610,.T.);
#6064=ORIENTED_EDGE('',*,*,#4606,.F.);
#6065=ORIENTED_EDGE('',*,*,#4611,.F.);
#6066=ORIENTED_EDGE('',*,*,#4612,.T.);
#6067=ORIENTED_EDGE('',*,*,#4613,.T.);
#6068=ORIENTED_EDGE('',*,*,#4609,.F.);
#6069=ORIENTED_EDGE('',*,*,#4614,.F.);
#6070=ORIENTED_EDGE('',*,*,#4615,.T.);
#6071=ORIENTED_EDGE('',*,*,#4616,.T.);
#6072=ORIENTED_EDGE('',*,*,#4612,.F.);
#6073=ORIENTED_EDGE('',*,*,#4617,.F.);
#6074=ORIENTED_EDGE('',*,*,#4618,.T.);
#6075=ORIENTED_EDGE('',*,*,#4619,.T.);
#6076=ORIENTED_EDGE('',*,*,#4615,.F.);
#6077=ORIENTED_EDGE('',*,*,#4620,.F.);
#6078=ORIENTED_EDGE('',*,*,#4621,.T.);
#6079=ORIENTED_EDGE('',*,*,#4622,.T.);
#6080=ORIENTED_EDGE('',*,*,#4618,.F.);
#6081=ORIENTED_EDGE('',*,*,#4623,.F.);
#6082=ORIENTED_EDGE('',*,*,#4624,.T.);
#6083=ORIENTED_EDGE('',*,*,#4625,.T.);
#6084=ORIENTED_EDGE('',*,*,#4621,.F.);
#6085=ORIENTED_EDGE('',*,*,#4626,.F.);
#6086=ORIENTED_EDGE('',*,*,#4627,.F.);
#6087=ORIENTED_EDGE('',*,*,#4628,.F.);
#6088=ORIENTED_EDGE('',*,*,#4629,.F.);
#6089=ORIENTED_EDGE('',*,*,#4630,.T.);
#6090=ORIENTED_EDGE('',*,*,#4631,.T.);
#6091=ORIENTED_EDGE('',*,*,#4632,.T.);
#6092=ORIENTED_EDGE('',*,*,#4633,.T.);
#6093=ORIENTED_EDGE('',*,*,#4634,.T.);
#6094=ORIENTED_EDGE('',*,*,#4635,.T.);
#6095=ORIENTED_EDGE('',*,*,#4636,.T.);
#6096=ORIENTED_EDGE('',*,*,#4635,.F.);
#6097=ORIENTED_EDGE('',*,*,#4637,.T.);
#6098=ORIENTED_EDGE('',*,*,#4638,.T.);
#6099=ORIENTED_EDGE('',*,*,#4639,.T.);
#6100=ORIENTED_EDGE('',*,*,#4631,.F.);
#6101=ORIENTED_EDGE('',*,*,#4640,.T.);
#6102=ORIENTED_EDGE('',*,*,#4641,.T.);
#6103=ORIENTED_EDGE('',*,*,#4642,.T.);
#6104=ORIENTED_EDGE('',*,*,#4638,.F.);
#6105=ORIENTED_EDGE('',*,*,#4643,.T.);
#6106=ORIENTED_EDGE('',*,*,#4644,.T.);
#6107=ORIENTED_EDGE('',*,*,#4645,.T.);
#6108=ORIENTED_EDGE('',*,*,#4641,.F.);
#6109=ORIENTED_EDGE('',*,*,#4646,.T.);
#6110=ORIENTED_EDGE('',*,*,#4647,.T.);
#6111=ORIENTED_EDGE('',*,*,#4648,.T.);
#6112=ORIENTED_EDGE('',*,*,#4644,.F.);
#6113=ORIENTED_EDGE('',*,*,#4649,.T.);
#6114=ORIENTED_EDGE('',*,*,#4650,.T.);
#6115=ORIENTED_EDGE('',*,*,#4651,.T.);
#6116=ORIENTED_EDGE('',*,*,#4647,.F.);
#6117=ORIENTED_EDGE('',*,*,#4652,.T.);
#6118=ORIENTED_EDGE('',*,*,#4653,.T.);
#6119=ORIENTED_EDGE('',*,*,#4654,.T.);
#6120=ORIENTED_EDGE('',*,*,#4650,.F.);
#6121=ORIENTED_EDGE('',*,*,#4655,.T.);
#6122=ORIENTED_EDGE('',*,*,#4656,.T.);
#6123=ORIENTED_EDGE('',*,*,#4657,.T.);
#6124=ORIENTED_EDGE('',*,*,#4653,.F.);
#6125=ORIENTED_EDGE('',*,*,#4658,.T.);
#6126=ORIENTED_EDGE('',*,*,#4659,.T.);
#6127=ORIENTED_EDGE('',*,*,#4660,.T.);
#6128=ORIENTED_EDGE('',*,*,#4656,.F.);
#6129=ORIENTED_EDGE('',*,*,#4661,.T.);
#6130=ORIENTED_EDGE('',*,*,#4662,.T.);
#6131=ORIENTED_EDGE('',*,*,#4663,.T.);
#6132=ORIENTED_EDGE('',*,*,#4659,.F.);
#6133=ORIENTED_EDGE('',*,*,#4664,.T.);
#6134=ORIENTED_EDGE('',*,*,#4665,.T.);
#6135=ORIENTED_EDGE('',*,*,#4666,.T.);
#6136=ORIENTED_EDGE('',*,*,#4662,.F.);
#6137=ORIENTED_EDGE('',*,*,#4667,.T.);
#6138=ORIENTED_EDGE('',*,*,#4668,.F.);
#6139=ORIENTED_EDGE('',*,*,#4669,.T.);
#6140=ORIENTED_EDGE('',*,*,#4670,.F.);
#6141=ORIENTED_EDGE('',*,*,#4671,.T.);
#6142=ORIENTED_EDGE('',*,*,#4672,.T.);
#6143=ORIENTED_EDGE('',*,*,#4673,.T.);
#6144=ORIENTED_EDGE('',*,*,#4674,.F.);
#6145=ORIENTED_EDGE('',*,*,#4675,.F.);
#6146=ORIENTED_EDGE('',*,*,#4676,.T.);
#6147=ORIENTED_EDGE('',*,*,#4677,.T.);
#6148=ORIENTED_EDGE('',*,*,#4672,.F.);
#6149=ORIENTED_EDGE('',*,*,#4678,.F.);
#6150=ORIENTED_EDGE('',*,*,#4679,.T.);
#6151=ORIENTED_EDGE('',*,*,#4680,.T.);
#6152=ORIENTED_EDGE('',*,*,#4676,.F.);
#6153=ORIENTED_EDGE('',*,*,#4681,.F.);
#6154=ORIENTED_EDGE('',*,*,#4682,.T.);
#6155=ORIENTED_EDGE('',*,*,#4683,.T.);
#6156=ORIENTED_EDGE('',*,*,#4679,.F.);
#6157=ORIENTED_EDGE('',*,*,#4684,.F.);
#6158=ORIENTED_EDGE('',*,*,#4685,.T.);
#6159=ORIENTED_EDGE('',*,*,#4686,.T.);
#6160=ORIENTED_EDGE('',*,*,#4682,.F.);
#6161=ORIENTED_EDGE('',*,*,#4687,.F.);
#6162=ORIENTED_EDGE('',*,*,#4688,.T.);
#6163=ORIENTED_EDGE('',*,*,#4689,.T.);
#6164=ORIENTED_EDGE('',*,*,#4685,.F.);
#6165=ORIENTED_EDGE('',*,*,#4690,.F.);
#6166=ORIENTED_EDGE('',*,*,#4691,.T.);
#6167=ORIENTED_EDGE('',*,*,#4692,.T.);
#6168=ORIENTED_EDGE('',*,*,#4688,.F.);
#6169=ORIENTED_EDGE('',*,*,#4693,.F.);
#6170=ORIENTED_EDGE('',*,*,#4694,.T.);
#6171=ORIENTED_EDGE('',*,*,#4695,.T.);
#6172=ORIENTED_EDGE('',*,*,#4691,.F.);
#6173=ORIENTED_EDGE('',*,*,#4696,.F.);
#6174=ORIENTED_EDGE('',*,*,#4697,.T.);
#6175=ORIENTED_EDGE('',*,*,#4698,.T.);
#6176=ORIENTED_EDGE('',*,*,#4694,.F.);
#6177=ORIENTED_EDGE('',*,*,#4699,.F.);
#6178=ORIENTED_EDGE('',*,*,#4700,.T.);
#6179=ORIENTED_EDGE('',*,*,#4701,.T.);
#6180=ORIENTED_EDGE('',*,*,#4697,.F.);
#6181=ORIENTED_EDGE('',*,*,#4702,.F.);
#6182=ORIENTED_EDGE('',*,*,#4703,.T.);
#6183=ORIENTED_EDGE('',*,*,#4704,.T.);
#6184=ORIENTED_EDGE('',*,*,#4700,.F.);
#6185=ORIENTED_EDGE('',*,*,#4705,.F.);
#6186=ORIENTED_EDGE('',*,*,#4706,.T.);
#6187=ORIENTED_EDGE('',*,*,#4707,.T.);
#6188=ORIENTED_EDGE('',*,*,#4703,.F.);
#6189=ORIENTED_EDGE('',*,*,#4708,.F.);
#6190=ORIENTED_EDGE('',*,*,#4709,.F.);
#6191=ORIENTED_EDGE('',*,*,#4710,.F.);
#6192=ORIENTED_EDGE('',*,*,#4711,.F.);
#6193=ORIENTED_EDGE('',*,*,#4712,.T.);
#6194=ORIENTED_EDGE('',*,*,#4713,.T.);
#6195=ORIENTED_EDGE('',*,*,#4714,.T.);
#6196=ORIENTED_EDGE('',*,*,#4715,.T.);
#6197=ORIENTED_EDGE('',*,*,#4716,.T.);
#6198=ORIENTED_EDGE('',*,*,#4717,.T.);
#6199=ORIENTED_EDGE('',*,*,#4718,.T.);
#6200=ORIENTED_EDGE('',*,*,#4717,.F.);
#6201=ORIENTED_EDGE('',*,*,#4719,.T.);
#6202=ORIENTED_EDGE('',*,*,#4720,.T.);
#6203=ORIENTED_EDGE('',*,*,#4721,.T.);
#6204=ORIENTED_EDGE('',*,*,#4713,.F.);
#6205=ORIENTED_EDGE('',*,*,#4722,.T.);
#6206=ORIENTED_EDGE('',*,*,#4723,.T.);
#6207=ORIENTED_EDGE('',*,*,#4724,.T.);
#6208=ORIENTED_EDGE('',*,*,#4720,.F.);
#6209=ORIENTED_EDGE('',*,*,#4725,.T.);
#6210=ORIENTED_EDGE('',*,*,#4726,.T.);
#6211=ORIENTED_EDGE('',*,*,#4727,.T.);
#6212=ORIENTED_EDGE('',*,*,#4723,.F.);
#6213=ORIENTED_EDGE('',*,*,#4728,.T.);
#6214=ORIENTED_EDGE('',*,*,#4729,.T.);
#6215=ORIENTED_EDGE('',*,*,#4730,.T.);
#6216=ORIENTED_EDGE('',*,*,#4726,.F.);
#6217=ORIENTED_EDGE('',*,*,#4731,.T.);
#6218=ORIENTED_EDGE('',*,*,#4732,.T.);
#6219=ORIENTED_EDGE('',*,*,#4733,.T.);
#6220=ORIENTED_EDGE('',*,*,#4729,.F.);
#6221=ORIENTED_EDGE('',*,*,#4734,.T.);
#6222=ORIENTED_EDGE('',*,*,#4735,.T.);
#6223=ORIENTED_EDGE('',*,*,#4736,.T.);
#6224=ORIENTED_EDGE('',*,*,#4732,.F.);
#6225=ORIENTED_EDGE('',*,*,#4737,.T.);
#6226=ORIENTED_EDGE('',*,*,#4738,.T.);
#6227=ORIENTED_EDGE('',*,*,#4739,.T.);
#6228=ORIENTED_EDGE('',*,*,#4735,.F.);
#6229=ORIENTED_EDGE('',*,*,#4740,.T.);
#6230=ORIENTED_EDGE('',*,*,#4741,.T.);
#6231=ORIENTED_EDGE('',*,*,#4742,.T.);
#6232=ORIENTED_EDGE('',*,*,#4738,.F.);
#6233=ORIENTED_EDGE('',*,*,#4743,.T.);
#6234=ORIENTED_EDGE('',*,*,#4744,.T.);
#6235=ORIENTED_EDGE('',*,*,#4745,.T.);
#6236=ORIENTED_EDGE('',*,*,#4741,.F.);
#6237=ORIENTED_EDGE('',*,*,#4746,.T.);
#6238=ORIENTED_EDGE('',*,*,#4747,.T.);
#6239=ORIENTED_EDGE('',*,*,#4748,.T.);
#6240=ORIENTED_EDGE('',*,*,#4744,.F.);
#6241=ORIENTED_EDGE('',*,*,#4749,.T.);
#6242=ORIENTED_EDGE('',*,*,#4750,.F.);
#6243=ORIENTED_EDGE('',*,*,#4751,.T.);
#6244=ORIENTED_EDGE('',*,*,#4752,.F.);
#6245=ORIENTED_EDGE('',*,*,#4753,.T.);
#6246=ORIENTED_EDGE('',*,*,#4754,.T.);
#6247=ORIENTED_EDGE('',*,*,#4755,.T.);
#6248=ORIENTED_EDGE('',*,*,#4756,.F.);
#6249=ORIENTED_EDGE('',*,*,#4757,.F.);
#6250=ORIENTED_EDGE('',*,*,#4758,.T.);
#6251=ORIENTED_EDGE('',*,*,#4759,.T.);
#6252=ORIENTED_EDGE('',*,*,#4754,.F.);
#6253=ORIENTED_EDGE('',*,*,#4760,.F.);
#6254=ORIENTED_EDGE('',*,*,#4761,.T.);
#6255=ORIENTED_EDGE('',*,*,#4762,.T.);
#6256=ORIENTED_EDGE('',*,*,#4758,.F.);
#6257=ORIENTED_EDGE('',*,*,#4763,.F.);
#6258=ORIENTED_EDGE('',*,*,#4764,.T.);
#6259=ORIENTED_EDGE('',*,*,#4765,.T.);
#6260=ORIENTED_EDGE('',*,*,#4761,.F.);
#6261=ORIENTED_EDGE('',*,*,#4766,.F.);
#6262=ORIENTED_EDGE('',*,*,#4767,.T.);
#6263=ORIENTED_EDGE('',*,*,#4768,.T.);
#6264=ORIENTED_EDGE('',*,*,#4764,.F.);
#6265=ORIENTED_EDGE('',*,*,#4769,.F.);
#6266=ORIENTED_EDGE('',*,*,#4770,.T.);
#6267=ORIENTED_EDGE('',*,*,#4771,.T.);
#6268=ORIENTED_EDGE('',*,*,#4767,.F.);
#6269=ORIENTED_EDGE('',*,*,#4772,.F.);
#6270=ORIENTED_EDGE('',*,*,#4773,.T.);
#6271=ORIENTED_EDGE('',*,*,#4774,.T.);
#6272=ORIENTED_EDGE('',*,*,#4770,.F.);
#6273=ORIENTED_EDGE('',*,*,#4775,.F.);
#6274=ORIENTED_EDGE('',*,*,#4776,.T.);
#6275=ORIENTED_EDGE('',*,*,#4777,.T.);
#6276=ORIENTED_EDGE('',*,*,#4773,.F.);
#6277=ORIENTED_EDGE('',*,*,#4778,.F.);
#6278=ORIENTED_EDGE('',*,*,#4779,.T.);
#6279=ORIENTED_EDGE('',*,*,#4780,.T.);
#6280=ORIENTED_EDGE('',*,*,#4776,.F.);
#6281=ORIENTED_EDGE('',*,*,#4781,.F.);
#6282=ORIENTED_EDGE('',*,*,#4782,.T.);
#6283=ORIENTED_EDGE('',*,*,#4783,.T.);
#6284=ORIENTED_EDGE('',*,*,#4779,.F.);
#6285=ORIENTED_EDGE('',*,*,#4784,.F.);
#6286=ORIENTED_EDGE('',*,*,#4785,.T.);
#6287=ORIENTED_EDGE('',*,*,#4786,.T.);
#6288=ORIENTED_EDGE('',*,*,#4782,.F.);
#6289=ORIENTED_EDGE('',*,*,#4787,.F.);
#6290=ORIENTED_EDGE('',*,*,#4788,.T.);
#6291=ORIENTED_EDGE('',*,*,#4789,.T.);
#6292=ORIENTED_EDGE('',*,*,#4785,.F.);
#6293=ORIENTED_EDGE('',*,*,#4790,.F.);
#6294=ORIENTED_EDGE('',*,*,#4791,.F.);
#6295=ORIENTED_EDGE('',*,*,#4792,.F.);
#6296=ORIENTED_EDGE('',*,*,#4793,.F.);
#6297=ORIENTED_EDGE('',*,*,#4794,.T.);
#6298=ORIENTED_EDGE('',*,*,#4795,.T.);
#6299=ORIENTED_EDGE('',*,*,#4796,.T.);
#6300=ORIENTED_EDGE('',*,*,#4797,.T.);
#6301=ORIENTED_EDGE('',*,*,#4798,.T.);
#6302=ORIENTED_EDGE('',*,*,#4799,.T.);
#6303=ORIENTED_EDGE('',*,*,#4800,.T.);
#6304=ORIENTED_EDGE('',*,*,#4799,.F.);
#6305=ORIENTED_EDGE('',*,*,#4801,.T.);
#6306=ORIENTED_EDGE('',*,*,#4802,.T.);
#6307=ORIENTED_EDGE('',*,*,#4803,.T.);
#6308=ORIENTED_EDGE('',*,*,#4795,.F.);
#6309=ORIENTED_EDGE('',*,*,#4804,.T.);
#6310=ORIENTED_EDGE('',*,*,#4805,.T.);
#6311=ORIENTED_EDGE('',*,*,#4806,.T.);
#6312=ORIENTED_EDGE('',*,*,#4802,.F.);
#6313=ORIENTED_EDGE('',*,*,#4807,.T.);
#6314=ORIENTED_EDGE('',*,*,#4808,.T.);
#6315=ORIENTED_EDGE('',*,*,#4809,.T.);
#6316=ORIENTED_EDGE('',*,*,#4805,.F.);
#6317=ORIENTED_EDGE('',*,*,#4810,.T.);
#6318=ORIENTED_EDGE('',*,*,#4811,.T.);
#6319=ORIENTED_EDGE('',*,*,#4812,.T.);
#6320=ORIENTED_EDGE('',*,*,#4808,.F.);
#6321=ORIENTED_EDGE('',*,*,#4813,.T.);
#6322=ORIENTED_EDGE('',*,*,#4814,.T.);
#6323=ORIENTED_EDGE('',*,*,#4815,.T.);
#6324=ORIENTED_EDGE('',*,*,#4811,.F.);
#6325=ORIENTED_EDGE('',*,*,#4816,.T.);
#6326=ORIENTED_EDGE('',*,*,#4817,.T.);
#6327=ORIENTED_EDGE('',*,*,#4818,.T.);
#6328=ORIENTED_EDGE('',*,*,#4814,.F.);
#6329=ORIENTED_EDGE('',*,*,#4819,.T.);
#6330=ORIENTED_EDGE('',*,*,#4820,.T.);
#6331=ORIENTED_EDGE('',*,*,#4821,.T.);
#6332=ORIENTED_EDGE('',*,*,#4817,.F.);
#6333=ORIENTED_EDGE('',*,*,#4822,.T.);
#6334=ORIENTED_EDGE('',*,*,#4823,.T.);
#6335=ORIENTED_EDGE('',*,*,#4824,.T.);
#6336=ORIENTED_EDGE('',*,*,#4820,.F.);
#6337=ORIENTED_EDGE('',*,*,#4825,.T.);
#6338=ORIENTED_EDGE('',*,*,#4826,.T.);
#6339=ORIENTED_EDGE('',*,*,#4827,.T.);
#6340=ORIENTED_EDGE('',*,*,#4823,.F.);
#6341=ORIENTED_EDGE('',*,*,#4828,.T.);
#6342=ORIENTED_EDGE('',*,*,#4829,.T.);
#6343=ORIENTED_EDGE('',*,*,#4830,.T.);
#6344=ORIENTED_EDGE('',*,*,#4826,.F.);
#6345=ORIENTED_EDGE('',*,*,#4831,.T.);
#6346=ORIENTED_EDGE('',*,*,#4832,.F.);
#6347=ORIENTED_EDGE('',*,*,#4833,.T.);
#6348=ORIENTED_EDGE('',*,*,#4834,.F.);
#6349=ORIENTED_EDGE('',*,*,#4835,.T.);
#6350=ORIENTED_EDGE('',*,*,#4836,.T.);
#6351=ORIENTED_EDGE('',*,*,#4837,.T.);
#6352=ORIENTED_EDGE('',*,*,#4838,.F.);
#6353=ORIENTED_EDGE('',*,*,#4839,.F.);
#6354=ORIENTED_EDGE('',*,*,#4840,.T.);
#6355=ORIENTED_EDGE('',*,*,#4841,.T.);
#6356=ORIENTED_EDGE('',*,*,#4836,.F.);
#6357=ORIENTED_EDGE('',*,*,#4842,.F.);
#6358=ORIENTED_EDGE('',*,*,#4843,.T.);
#6359=ORIENTED_EDGE('',*,*,#4844,.T.);
#6360=ORIENTED_EDGE('',*,*,#4840,.F.);
#6361=ORIENTED_EDGE('',*,*,#4845,.F.);
#6362=ORIENTED_EDGE('',*,*,#4846,.T.);
#6363=ORIENTED_EDGE('',*,*,#4847,.T.);
#6364=ORIENTED_EDGE('',*,*,#4843,.F.);
#6365=ORIENTED_EDGE('',*,*,#4848,.F.);
#6366=ORIENTED_EDGE('',*,*,#4849,.T.);
#6367=ORIENTED_EDGE('',*,*,#4850,.T.);
#6368=ORIENTED_EDGE('',*,*,#4846,.F.);
#6369=ORIENTED_EDGE('',*,*,#4851,.F.);
#6370=ORIENTED_EDGE('',*,*,#4852,.T.);
#6371=ORIENTED_EDGE('',*,*,#4853,.T.);
#6372=ORIENTED_EDGE('',*,*,#4849,.F.);
#6373=ORIENTED_EDGE('',*,*,#4854,.F.);
#6374=ORIENTED_EDGE('',*,*,#4855,.T.);
#6375=ORIENTED_EDGE('',*,*,#4856,.T.);
#6376=ORIENTED_EDGE('',*,*,#4852,.F.);
#6377=ORIENTED_EDGE('',*,*,#4857,.F.);
#6378=ORIENTED_EDGE('',*,*,#4858,.T.);
#6379=ORIENTED_EDGE('',*,*,#4859,.T.);
#6380=ORIENTED_EDGE('',*,*,#4855,.F.);
#6381=ORIENTED_EDGE('',*,*,#4860,.F.);
#6382=ORIENTED_EDGE('',*,*,#4861,.T.);
#6383=ORIENTED_EDGE('',*,*,#4862,.T.);
#6384=ORIENTED_EDGE('',*,*,#4858,.F.);
#6385=ORIENTED_EDGE('',*,*,#4863,.F.);
#6386=ORIENTED_EDGE('',*,*,#4864,.T.);
#6387=ORIENTED_EDGE('',*,*,#4865,.T.);
#6388=ORIENTED_EDGE('',*,*,#4861,.F.);
#6389=ORIENTED_EDGE('',*,*,#4866,.F.);
#6390=ORIENTED_EDGE('',*,*,#4867,.T.);
#6391=ORIENTED_EDGE('',*,*,#4868,.T.);
#6392=ORIENTED_EDGE('',*,*,#4864,.F.);
#6393=ORIENTED_EDGE('',*,*,#4869,.F.);
#6394=ORIENTED_EDGE('',*,*,#4870,.T.);
#6395=ORIENTED_EDGE('',*,*,#4871,.T.);
#6396=ORIENTED_EDGE('',*,*,#4867,.F.);
#6397=ORIENTED_EDGE('',*,*,#4872,.F.);
#6398=ORIENTED_EDGE('',*,*,#4873,.F.);
#6399=ORIENTED_EDGE('',*,*,#4874,.F.);
#6400=ORIENTED_EDGE('',*,*,#4875,.F.);
#6401=ORIENTED_EDGE('',*,*,#4876,.T.);
#6402=ORIENTED_EDGE('',*,*,#4877,.F.);
#6403=ORIENTED_EDGE('',*,*,#4878,.T.);
#6404=ORIENTED_EDGE('',*,*,#4879,.T.);
#6405=ORIENTED_EDGE('',*,*,#4880,.T.);
#6406=ORIENTED_EDGE('',*,*,#4878,.F.);
#6407=ORIENTED_EDGE('',*,*,#4881,.T.);
#6408=ORIENTED_EDGE('',*,*,#4882,.F.);
#6409=ORIENTED_EDGE('',*,*,#4883,.F.);
#6410=ORIENTED_EDGE('',*,*,#4884,.F.);
#6411=ORIENTED_EDGE('',*,*,#4885,.T.);
#6412=ORIENTED_EDGE('',*,*,#4886,.T.);
#6413=ORIENTED_EDGE('',*,*,#4882,.T.);
#6414=ORIENTED_EDGE('',*,*,#4885,.F.);
#6415=ORIENTED_EDGE('',*,*,#4887,.T.);
#6416=ORIENTED_EDGE('',*,*,#4888,.F.);
#6417=ORIENTED_EDGE('',*,*,#4889,.F.);
#6418=ORIENTED_EDGE('',*,*,#4890,.F.);
#6419=ORIENTED_EDGE('',*,*,#4891,.T.);
#6420=ORIENTED_EDGE('',*,*,#4892,.T.);
#6421=ORIENTED_EDGE('',*,*,#4893,.T.);
#6422=ORIENTED_EDGE('',*,*,#4877,.T.);
#6423=ORIENTED_EDGE('',*,*,#4894,.F.);
#6424=ORIENTED_EDGE('',*,*,#4890,.T.);
#6425=ORIENTED_EDGE('',*,*,#4895,.F.);
#6426=ORIENTED_EDGE('',*,*,#4896,.T.);
#6427=ORIENTED_EDGE('',*,*,#4887,.F.);
#6428=ORIENTED_EDGE('',*,*,#4884,.T.);
#6429=ORIENTED_EDGE('',*,*,#4881,.F.);
#6430=ORIENTED_EDGE('',*,*,#4897,.T.);
#6431=ORIENTED_EDGE('',*,*,#4898,.T.);
#6432=ORIENTED_EDGE('',*,*,#4899,.T.);
#6433=ORIENTED_EDGE('',*,*,#4893,.F.);
#6434=ORIENTED_EDGE('',*,*,#4900,.F.);
#6435=ORIENTED_EDGE('',*,*,#4901,.F.);
#6436=ORIENTED_EDGE('',*,*,#4895,.T.);
#6437=ORIENTED_EDGE('',*,*,#4902,.T.);
#6438=ORIENTED_EDGE('',*,*,#4896,.F.);
#6439=ORIENTED_EDGE('',*,*,#4901,.T.);
#6440=ORIENTED_EDGE('',*,*,#4903,.T.);
#6441=ORIENTED_EDGE('',*,*,#4888,.T.);
#6442=ORIENTED_EDGE('',*,*,#4904,.F.);
#6443=ORIENTED_EDGE('',*,*,#4905,.T.);
#6444=ORIENTED_EDGE('',*,*,#4902,.F.);
#6445=ORIENTED_EDGE('',*,*,#4905,.F.);
#6446=ORIENTED_EDGE('',*,*,#4906,.F.);
#6447=ORIENTED_EDGE('',*,*,#4907,.T.);
#6448=ORIENTED_EDGE('',*,*,#4908,.F.);
#6449=ORIENTED_EDGE('',*,*,#4909,.T.);
#6450=ORIENTED_EDGE('',*,*,#4906,.T.);
#6451=ORIENTED_EDGE('',*,*,#4909,.F.);
#6452=ORIENTED_EDGE('',*,*,#4907,.F.);
#6453=ORIENTED_EDGE('',*,*,#4910,.T.);
#6454=ORIENTED_EDGE('',*,*,#4899,.F.);
#6455=ORIENTED_EDGE('',*,*,#4910,.F.);
#6456=ORIENTED_EDGE('',*,*,#4911,.F.);
#6457=ORIENTED_EDGE('',*,*,#4912,.T.);
#6458=ORIENTED_EDGE('',*,*,#4913,.F.);
#6459=ORIENTED_EDGE('',*,*,#4914,.T.);
#6460=ORIENTED_EDGE('',*,*,#4911,.T.);
#6461=ORIENTED_EDGE('',*,*,#4914,.F.);
#6462=ORIENTED_EDGE('',*,*,#4912,.F.);
#6463=ORIENTED_EDGE('',*,*,#4915,.T.);
#6464=ORIENTED_EDGE('',*,*,#4898,.F.);
#6465=ORIENTED_EDGE('',*,*,#4915,.F.);
#6466=ORIENTED_EDGE('',*,*,#4797,.F.);
#6467=ORIENTED_EDGE('',*,*,#4916,.T.);
#6468=ORIENTED_EDGE('',*,*,#4838,.T.);
#6469=ORIENTED_EDGE('',*,*,#4917,.T.);
#6470=ORIENTED_EDGE('',*,*,#4873,.T.);
#6471=ORIENTED_EDGE('',*,*,#4918,.T.);
#6472=ORIENTED_EDGE('',*,*,#4870,.F.);
#6473=ORIENTED_EDGE('',*,*,#4919,.F.);
#6474=ORIENTED_EDGE('',*,*,#4917,.F.);
#6475=ORIENTED_EDGE('',*,*,#4837,.F.);
#6476=ORIENTED_EDGE('',*,*,#4841,.F.);
#6477=ORIENTED_EDGE('',*,*,#4844,.F.);
#6478=ORIENTED_EDGE('',*,*,#4847,.F.);
#6479=ORIENTED_EDGE('',*,*,#4850,.F.);
#6480=ORIENTED_EDGE('',*,*,#4853,.F.);
#6481=ORIENTED_EDGE('',*,*,#4856,.F.);
#6482=ORIENTED_EDGE('',*,*,#4859,.F.);
#6483=ORIENTED_EDGE('',*,*,#4862,.F.);
#6484=ORIENTED_EDGE('',*,*,#4865,.F.);
#6485=ORIENTED_EDGE('',*,*,#4868,.F.);
#6486=ORIENTED_EDGE('',*,*,#4871,.F.);
#6487=ORIENTED_EDGE('',*,*,#4918,.F.);
#6488=ORIENTED_EDGE('',*,*,#4876,.F.);
#6489=ORIENTED_EDGE('',*,*,#4920,.F.);
#6490=ORIENTED_EDGE('',*,*,#4833,.F.);
#6491=ORIENTED_EDGE('',*,*,#4921,.F.);
#6492=ORIENTED_EDGE('',*,*,#4831,.F.);
#6493=ORIENTED_EDGE('',*,*,#4828,.F.);
#6494=ORIENTED_EDGE('',*,*,#4825,.F.);
#6495=ORIENTED_EDGE('',*,*,#4822,.F.);
#6496=ORIENTED_EDGE('',*,*,#4819,.F.);
#6497=ORIENTED_EDGE('',*,*,#4816,.F.);
#6498=ORIENTED_EDGE('',*,*,#4813,.F.);
#6499=ORIENTED_EDGE('',*,*,#4810,.F.);
#6500=ORIENTED_EDGE('',*,*,#4807,.F.);
#6501=ORIENTED_EDGE('',*,*,#4804,.F.);
#6502=ORIENTED_EDGE('',*,*,#4801,.F.);
#6503=ORIENTED_EDGE('',*,*,#4798,.F.);
#6504=ORIENTED_EDGE('',*,*,#4916,.F.);
#6505=ORIENTED_EDGE('',*,*,#4796,.F.);
#6506=ORIENTED_EDGE('',*,*,#4803,.F.);
#6507=ORIENTED_EDGE('',*,*,#4806,.F.);
#6508=ORIENTED_EDGE('',*,*,#4809,.F.);
#6509=ORIENTED_EDGE('',*,*,#4812,.F.);
#6510=ORIENTED_EDGE('',*,*,#4815,.F.);
#6511=ORIENTED_EDGE('',*,*,#4818,.F.);
#6512=ORIENTED_EDGE('',*,*,#4821,.F.);
#6513=ORIENTED_EDGE('',*,*,#4824,.F.);
#6514=ORIENTED_EDGE('',*,*,#4827,.F.);
#6515=ORIENTED_EDGE('',*,*,#4830,.F.);
#6516=ORIENTED_EDGE('',*,*,#4922,.F.);
#6517=ORIENTED_EDGE('',*,*,#4835,.F.);
#6518=ORIENTED_EDGE('',*,*,#4923,.F.);
#6519=ORIENTED_EDGE('',*,*,#4874,.T.);
#6520=ORIENTED_EDGE('',*,*,#4919,.T.);
#6521=ORIENTED_EDGE('',*,*,#4872,.T.);
#6522=ORIENTED_EDGE('',*,*,#4869,.T.);
#6523=ORIENTED_EDGE('',*,*,#4866,.T.);
#6524=ORIENTED_EDGE('',*,*,#4863,.T.);
#6525=ORIENTED_EDGE('',*,*,#4860,.T.);
#6526=ORIENTED_EDGE('',*,*,#4857,.T.);
#6527=ORIENTED_EDGE('',*,*,#4854,.T.);
#6528=ORIENTED_EDGE('',*,*,#4851,.T.);
#6529=ORIENTED_EDGE('',*,*,#4848,.T.);
#6530=ORIENTED_EDGE('',*,*,#4845,.T.);
#6531=ORIENTED_EDGE('',*,*,#4842,.T.);
#6532=ORIENTED_EDGE('',*,*,#4839,.T.);
#6533=ORIENTED_EDGE('',*,*,#4832,.T.);
#6534=ORIENTED_EDGE('',*,*,#4922,.T.);
#6535=ORIENTED_EDGE('',*,*,#4829,.F.);
#6536=ORIENTED_EDGE('',*,*,#4921,.T.);
#6537=ORIENTED_EDGE('',*,*,#4715,.F.);
#6538=ORIENTED_EDGE('',*,*,#4924,.T.);
#6539=ORIENTED_EDGE('',*,*,#4756,.T.);
#6540=ORIENTED_EDGE('',*,*,#4925,.T.);
#6541=ORIENTED_EDGE('',*,*,#4791,.T.);
#6542=ORIENTED_EDGE('',*,*,#4926,.T.);
#6543=ORIENTED_EDGE('',*,*,#4788,.F.);
#6544=ORIENTED_EDGE('',*,*,#4927,.F.);
#6545=ORIENTED_EDGE('',*,*,#4925,.F.);
#6546=ORIENTED_EDGE('',*,*,#4755,.F.);
#6547=ORIENTED_EDGE('',*,*,#4759,.F.);
#6548=ORIENTED_EDGE('',*,*,#4762,.F.);
#6549=ORIENTED_EDGE('',*,*,#4765,.F.);
#6550=ORIENTED_EDGE('',*,*,#4768,.F.);
#6551=ORIENTED_EDGE('',*,*,#4771,.F.);
#6552=ORIENTED_EDGE('',*,*,#4774,.F.);
#6553=ORIENTED_EDGE('',*,*,#4777,.F.);
#6554=ORIENTED_EDGE('',*,*,#4780,.F.);
#6555=ORIENTED_EDGE('',*,*,#4783,.F.);
#6556=ORIENTED_EDGE('',*,*,#4786,.F.);
#6557=ORIENTED_EDGE('',*,*,#4789,.F.);
#6558=ORIENTED_EDGE('',*,*,#4926,.F.);
#6559=ORIENTED_EDGE('',*,*,#4794,.F.);
#6560=ORIENTED_EDGE('',*,*,#4928,.F.);
#6561=ORIENTED_EDGE('',*,*,#4751,.F.);
#6562=ORIENTED_EDGE('',*,*,#4929,.F.);
#6563=ORIENTED_EDGE('',*,*,#4749,.F.);
#6564=ORIENTED_EDGE('',*,*,#4746,.F.);
#6565=ORIENTED_EDGE('',*,*,#4743,.F.);
#6566=ORIENTED_EDGE('',*,*,#4740,.F.);
#6567=ORIENTED_EDGE('',*,*,#4737,.F.);
#6568=ORIENTED_EDGE('',*,*,#4734,.F.);
#6569=ORIENTED_EDGE('',*,*,#4731,.F.);
#6570=ORIENTED_EDGE('',*,*,#4728,.F.);
#6571=ORIENTED_EDGE('',*,*,#4725,.F.);
#6572=ORIENTED_EDGE('',*,*,#4722,.F.);
#6573=ORIENTED_EDGE('',*,*,#4719,.F.);
#6574=ORIENTED_EDGE('',*,*,#4716,.F.);
#6575=ORIENTED_EDGE('',*,*,#4924,.F.);
#6576=ORIENTED_EDGE('',*,*,#4714,.F.);
#6577=ORIENTED_EDGE('',*,*,#4721,.F.);
#6578=ORIENTED_EDGE('',*,*,#4724,.F.);
#6579=ORIENTED_EDGE('',*,*,#4727,.F.);
#6580=ORIENTED_EDGE('',*,*,#4730,.F.);
#6581=ORIENTED_EDGE('',*,*,#4733,.F.);
#6582=ORIENTED_EDGE('',*,*,#4736,.F.);
#6583=ORIENTED_EDGE('',*,*,#4739,.F.);
#6584=ORIENTED_EDGE('',*,*,#4742,.F.);
#6585=ORIENTED_EDGE('',*,*,#4745,.F.);
#6586=ORIENTED_EDGE('',*,*,#4748,.F.);
#6587=ORIENTED_EDGE('',*,*,#4930,.F.);
#6588=ORIENTED_EDGE('',*,*,#4753,.F.);
#6589=ORIENTED_EDGE('',*,*,#4931,.F.);
#6590=ORIENTED_EDGE('',*,*,#4792,.T.);
#6591=ORIENTED_EDGE('',*,*,#4927,.T.);
#6592=ORIENTED_EDGE('',*,*,#4790,.T.);
#6593=ORIENTED_EDGE('',*,*,#4787,.T.);
#6594=ORIENTED_EDGE('',*,*,#4784,.T.);
#6595=ORIENTED_EDGE('',*,*,#4781,.T.);
#6596=ORIENTED_EDGE('',*,*,#4778,.T.);
#6597=ORIENTED_EDGE('',*,*,#4775,.T.);
#6598=ORIENTED_EDGE('',*,*,#4772,.T.);
#6599=ORIENTED_EDGE('',*,*,#4769,.T.);
#6600=ORIENTED_EDGE('',*,*,#4766,.T.);
#6601=ORIENTED_EDGE('',*,*,#4763,.T.);
#6602=ORIENTED_EDGE('',*,*,#4760,.T.);
#6603=ORIENTED_EDGE('',*,*,#4757,.T.);
#6604=ORIENTED_EDGE('',*,*,#4750,.T.);
#6605=ORIENTED_EDGE('',*,*,#4930,.T.);
#6606=ORIENTED_EDGE('',*,*,#4747,.F.);
#6607=ORIENTED_EDGE('',*,*,#4929,.T.);
#6608=ORIENTED_EDGE('',*,*,#4633,.F.);
#6609=ORIENTED_EDGE('',*,*,#4932,.T.);
#6610=ORIENTED_EDGE('',*,*,#4674,.T.);
#6611=ORIENTED_EDGE('',*,*,#4933,.T.);
#6612=ORIENTED_EDGE('',*,*,#4709,.T.);
#6613=ORIENTED_EDGE('',*,*,#4934,.T.);
#6614=ORIENTED_EDGE('',*,*,#4706,.F.);
#6615=ORIENTED_EDGE('',*,*,#4935,.F.);
#6616=ORIENTED_EDGE('',*,*,#4933,.F.);
#6617=ORIENTED_EDGE('',*,*,#4673,.F.);
#6618=ORIENTED_EDGE('',*,*,#4677,.F.);
#6619=ORIENTED_EDGE('',*,*,#4680,.F.);
#6620=ORIENTED_EDGE('',*,*,#4683,.F.);
#6621=ORIENTED_EDGE('',*,*,#4686,.F.);
#6622=ORIENTED_EDGE('',*,*,#4689,.F.);
#6623=ORIENTED_EDGE('',*,*,#4692,.F.);
#6624=ORIENTED_EDGE('',*,*,#4695,.F.);
#6625=ORIENTED_EDGE('',*,*,#4698,.F.);
#6626=ORIENTED_EDGE('',*,*,#4701,.F.);
#6627=ORIENTED_EDGE('',*,*,#4704,.F.);
#6628=ORIENTED_EDGE('',*,*,#4707,.F.);
#6629=ORIENTED_EDGE('',*,*,#4934,.F.);
#6630=ORIENTED_EDGE('',*,*,#4712,.F.);
#6631=ORIENTED_EDGE('',*,*,#4936,.F.);
#6632=ORIENTED_EDGE('',*,*,#4669,.F.);
#6633=ORIENTED_EDGE('',*,*,#4937,.F.);
#6634=ORIENTED_EDGE('',*,*,#4667,.F.);
#6635=ORIENTED_EDGE('',*,*,#4664,.F.);
#6636=ORIENTED_EDGE('',*,*,#4661,.F.);
#6637=ORIENTED_EDGE('',*,*,#4658,.F.);
#6638=ORIENTED_EDGE('',*,*,#4655,.F.);
#6639=ORIENTED_EDGE('',*,*,#4652,.F.);
#6640=ORIENTED_EDGE('',*,*,#4649,.F.);
#6641=ORIENTED_EDGE('',*,*,#4646,.F.);
#6642=ORIENTED_EDGE('',*,*,#4643,.F.);
#6643=ORIENTED_EDGE('',*,*,#4640,.F.);
#6644=ORIENTED_EDGE('',*,*,#4637,.F.);
#6645=ORIENTED_EDGE('',*,*,#4634,.F.);
#6646=ORIENTED_EDGE('',*,*,#4932,.F.);
#6647=ORIENTED_EDGE('',*,*,#4632,.F.);
#6648=ORIENTED_EDGE('',*,*,#4639,.F.);
#6649=ORIENTED_EDGE('',*,*,#4642,.F.);
#6650=ORIENTED_EDGE('',*,*,#4645,.F.);
#6651=ORIENTED_EDGE('',*,*,#4648,.F.);
#6652=ORIENTED_EDGE('',*,*,#4651,.F.);
#6653=ORIENTED_EDGE('',*,*,#4654,.F.);
#6654=ORIENTED_EDGE('',*,*,#4657,.F.);
#6655=ORIENTED_EDGE('',*,*,#4660,.F.);
#6656=ORIENTED_EDGE('',*,*,#4663,.F.);
#6657=ORIENTED_EDGE('',*,*,#4666,.F.);
#6658=ORIENTED_EDGE('',*,*,#4938,.F.);
#6659=ORIENTED_EDGE('',*,*,#4671,.F.);
#6660=ORIENTED_EDGE('',*,*,#4939,.F.);
#6661=ORIENTED_EDGE('',*,*,#4710,.T.);
#6662=ORIENTED_EDGE('',*,*,#4935,.T.);
#6663=ORIENTED_EDGE('',*,*,#4708,.T.);
#6664=ORIENTED_EDGE('',*,*,#4705,.T.);
#6665=ORIENTED_EDGE('',*,*,#4702,.T.);
#6666=ORIENTED_EDGE('',*,*,#4699,.T.);
#6667=ORIENTED_EDGE('',*,*,#4696,.T.);
#6668=ORIENTED_EDGE('',*,*,#4693,.T.);
#6669=ORIENTED_EDGE('',*,*,#4690,.T.);
#6670=ORIENTED_EDGE('',*,*,#4687,.T.);
#6671=ORIENTED_EDGE('',*,*,#4684,.T.);
#6672=ORIENTED_EDGE('',*,*,#4681,.T.);
#6673=ORIENTED_EDGE('',*,*,#4678,.T.);
#6674=ORIENTED_EDGE('',*,*,#4675,.T.);
#6675=ORIENTED_EDGE('',*,*,#4668,.T.);
#6676=ORIENTED_EDGE('',*,*,#4938,.T.);
#6677=ORIENTED_EDGE('',*,*,#4665,.F.);
#6678=ORIENTED_EDGE('',*,*,#4937,.T.);
#6679=ORIENTED_EDGE('',*,*,#4551,.F.);
#6680=ORIENTED_EDGE('',*,*,#4940,.T.);
#6681=ORIENTED_EDGE('',*,*,#4592,.T.);
#6682=ORIENTED_EDGE('',*,*,#4941,.T.);
#6683=ORIENTED_EDGE('',*,*,#4627,.T.);
#6684=ORIENTED_EDGE('',*,*,#4942,.T.);
#6685=ORIENTED_EDGE('',*,*,#4624,.F.);
#6686=ORIENTED_EDGE('',*,*,#4943,.F.);
#6687=ORIENTED_EDGE('',*,*,#4941,.F.);
#6688=ORIENTED_EDGE('',*,*,#4591,.F.);
#6689=ORIENTED_EDGE('',*,*,#4595,.F.);
#6690=ORIENTED_EDGE('',*,*,#4598,.F.);
#6691=ORIENTED_EDGE('',*,*,#4601,.F.);
#6692=ORIENTED_EDGE('',*,*,#4604,.F.);
#6693=ORIENTED_EDGE('',*,*,#4607,.F.);
#6694=ORIENTED_EDGE('',*,*,#4610,.F.);
#6695=ORIENTED_EDGE('',*,*,#4613,.F.);
#6696=ORIENTED_EDGE('',*,*,#4616,.F.);
#6697=ORIENTED_EDGE('',*,*,#4619,.F.);
#6698=ORIENTED_EDGE('',*,*,#4622,.F.);
#6699=ORIENTED_EDGE('',*,*,#4625,.F.);
#6700=ORIENTED_EDGE('',*,*,#4942,.F.);
#6701=ORIENTED_EDGE('',*,*,#4630,.F.);
#6702=ORIENTED_EDGE('',*,*,#4944,.F.);
#6703=ORIENTED_EDGE('',*,*,#4587,.F.);
#6704=ORIENTED_EDGE('',*,*,#4945,.F.);
#6705=ORIENTED_EDGE('',*,*,#4585,.F.);
#6706=ORIENTED_EDGE('',*,*,#4582,.F.);
#6707=ORIENTED_EDGE('',*,*,#4579,.F.);
#6708=ORIENTED_EDGE('',*,*,#4576,.F.);
#6709=ORIENTED_EDGE('',*,*,#4573,.F.);
#6710=ORIENTED_EDGE('',*,*,#4570,.F.);
#6711=ORIENTED_EDGE('',*,*,#4567,.F.);
#6712=ORIENTED_EDGE('',*,*,#4564,.F.);
#6713=ORIENTED_EDGE('',*,*,#4561,.F.);
#6714=ORIENTED_EDGE('',*,*,#4558,.F.);
#6715=ORIENTED_EDGE('',*,*,#4555,.F.);
#6716=ORIENTED_EDGE('',*,*,#4552,.F.);
#6717=ORIENTED_EDGE('',*,*,#4940,.F.);
#6718=ORIENTED_EDGE('',*,*,#4550,.F.);
#6719=ORIENTED_EDGE('',*,*,#4557,.F.);
#6720=ORIENTED_EDGE('',*,*,#4560,.F.);
#6721=ORIENTED_EDGE('',*,*,#4563,.F.);
#6722=ORIENTED_EDGE('',*,*,#4566,.F.);
#6723=ORIENTED_EDGE('',*,*,#4569,.F.);
#6724=ORIENTED_EDGE('',*,*,#4572,.F.);
#6725=ORIENTED_EDGE('',*,*,#4575,.F.);
#6726=ORIENTED_EDGE('',*,*,#4578,.F.);
#6727=ORIENTED_EDGE('',*,*,#4581,.F.);
#6728=ORIENTED_EDGE('',*,*,#4584,.F.);
#6729=ORIENTED_EDGE('',*,*,#4946,.F.);
#6730=ORIENTED_EDGE('',*,*,#4589,.F.);
#6731=ORIENTED_EDGE('',*,*,#4947,.F.);
#6732=ORIENTED_EDGE('',*,*,#4628,.T.);
#6733=ORIENTED_EDGE('',*,*,#4943,.T.);
#6734=ORIENTED_EDGE('',*,*,#4626,.T.);
#6735=ORIENTED_EDGE('',*,*,#4623,.T.);
#6736=ORIENTED_EDGE('',*,*,#4620,.T.);
#6737=ORIENTED_EDGE('',*,*,#4617,.T.);
#6738=ORIENTED_EDGE('',*,*,#4614,.T.);
#6739=ORIENTED_EDGE('',*,*,#4611,.T.);
#6740=ORIENTED_EDGE('',*,*,#4608,.T.);
#6741=ORIENTED_EDGE('',*,*,#4605,.T.);
#6742=ORIENTED_EDGE('',*,*,#4602,.T.);
#6743=ORIENTED_EDGE('',*,*,#4599,.T.);
#6744=ORIENTED_EDGE('',*,*,#4596,.T.);
#6745=ORIENTED_EDGE('',*,*,#4593,.T.);
#6746=ORIENTED_EDGE('',*,*,#4586,.T.);
#6747=ORIENTED_EDGE('',*,*,#4946,.T.);
#6748=ORIENTED_EDGE('',*,*,#4583,.F.);
#6749=ORIENTED_EDGE('',*,*,#4945,.T.);
#6750=ORIENTED_EDGE('',*,*,#4636,.F.);
#6751=ORIENTED_EDGE('',*,*,#4718,.F.);
#6752=ORIENTED_EDGE('',*,*,#4800,.F.);
#6753=ORIENTED_EDGE('',*,*,#4554,.F.);
#6754=ORIENTED_EDGE('',*,*,#4948,.F.);
#6755=ORIENTED_EDGE('',*,*,#4949,.T.);
#6756=ORIENTED_EDGE('',*,*,#4950,.F.);
#6757=ORIENTED_EDGE('',*,*,#4949,.F.);
#6758=ORIENTED_EDGE('',*,*,#4951,.F.);
#6759=ORIENTED_EDGE('',*,*,#4952,.T.);
#6760=ORIENTED_EDGE('',*,*,#4953,.F.);
#6761=ORIENTED_EDGE('',*,*,#4952,.F.);
#6762=ORIENTED_EDGE('',*,*,#4954,.T.);
#6763=ORIENTED_EDGE('',*,*,#4955,.F.);
#6764=ORIENTED_EDGE('',*,*,#4956,.F.);
#6765=ORIENTED_EDGE('',*,*,#4957,.F.);
#6766=ORIENTED_EDGE('',*,*,#4958,.T.);
#6767=ORIENTED_EDGE('',*,*,#4957,.T.);
#6768=ORIENTED_EDGE('',*,*,#4959,.F.);
#6769=ORIENTED_EDGE('',*,*,#4960,.F.);
#6770=ORIENTED_EDGE('',*,*,#4961,.T.);
#6771=ORIENTED_EDGE('',*,*,#4960,.T.);
#6772=ORIENTED_EDGE('',*,*,#4962,.F.);
#6773=ORIENTED_EDGE('',*,*,#4963,.F.);
#6774=ORIENTED_EDGE('',*,*,#4964,.F.);
#6775=ORIENTED_EDGE('',*,*,#4962,.T.);
#6776=ORIENTED_EDGE('',*,*,#4959,.T.);
#6777=ORIENTED_EDGE('',*,*,#4956,.T.);
#6778=ORIENTED_EDGE('',*,*,#4951,.T.);
#6779=ORIENTED_EDGE('',*,*,#4965,.T.);
#6780=ORIENTED_EDGE('',*,*,#4966,.T.);
#6781=ORIENTED_EDGE('',*,*,#4967,.F.);
#6782=ORIENTED_EDGE('',*,*,#4968,.F.);
#6783=ORIENTED_EDGE('',*,*,#4969,.T.);
#6784=ORIENTED_EDGE('',*,*,#4970,.F.);
#6785=ORIENTED_EDGE('',*,*,#4971,.F.);
#6786=ORIENTED_EDGE('',*,*,#4972,.F.);
#6787=ORIENTED_EDGE('',*,*,#4973,.T.);
#6788=ORIENTED_EDGE('',*,*,#4972,.T.);
#6789=ORIENTED_EDGE('',*,*,#4974,.F.);
#6790=ORIENTED_EDGE('',*,*,#4966,.F.);
#6791=ORIENTED_EDGE('',*,*,#4974,.T.);
#6792=ORIENTED_EDGE('',*,*,#4971,.T.);
#6793=ORIENTED_EDGE('',*,*,#4975,.F.);
#6794=ORIENTED_EDGE('',*,*,#4967,.T.);
#6795=ORIENTED_EDGE('',*,*,#4948,.T.);
#6796=ORIENTED_EDGE('',*,*,#4976,.F.);
#6797=ORIENTED_EDGE('',*,*,#4977,.T.);
#6798=ORIENTED_EDGE('',*,*,#4978,.F.);
#6799=ORIENTED_EDGE('',*,*,#4977,.F.);
#6800=ORIENTED_EDGE('',*,*,#4979,.F.);
#6801=ORIENTED_EDGE('',*,*,#4980,.T.);
#6802=ORIENTED_EDGE('',*,*,#4897,.F.);
#6803=ORIENTED_EDGE('',*,*,#4980,.F.);
#6804=ORIENTED_EDGE('',*,*,#4979,.T.);
#6805=ORIENTED_EDGE('',*,*,#4976,.T.);
#6806=ORIENTED_EDGE('',*,*,#4880,.F.);
#6807=ORIENTED_EDGE('',*,*,#4981,.F.);
#6808=ORIENTED_EDGE('',*,*,#4891,.F.);
#6809=ORIENTED_EDGE('',*,*,#4894,.T.);
#6810=ORIENTED_EDGE('',*,*,#4978,.T.);
#6811=ORIENTED_EDGE('',*,*,#4982,.T.);
#6812=ORIENTED_EDGE('',*,*,#4983,.T.);
#6813=ORIENTED_EDGE('',*,*,#4984,.F.);
#6814=ORIENTED_EDGE('',*,*,#4985,.F.);
#6815=ORIENTED_EDGE('',*,*,#4955,.T.);
#6816=ORIENTED_EDGE('',*,*,#4986,.T.);
#6817=ORIENTED_EDGE('',*,*,#4985,.T.);
#6818=ORIENTED_EDGE('',*,*,#4987,.F.);
#6819=ORIENTED_EDGE('',*,*,#4988,.F.);
#6820=ORIENTED_EDGE('',*,*,#4989,.T.);
#6821=ORIENTED_EDGE('',*,*,#4963,.T.);
#6822=ORIENTED_EDGE('',*,*,#4964,.T.);
#6823=ORIENTED_EDGE('',*,*,#4990,.T.);
#6824=ORIENTED_EDGE('',*,*,#4988,.T.);
#6825=ORIENTED_EDGE('',*,*,#4991,.F.);
#6826=ORIENTED_EDGE('',*,*,#4992,.F.);
#6827=ORIENTED_EDGE('',*,*,#4904,.T.);
#6828=ORIENTED_EDGE('',*,*,#4970,.T.);
#6829=ORIENTED_EDGE('',*,*,#4993,.T.);
#6830=ORIENTED_EDGE('',*,*,#4992,.T.);
#6831=ORIENTED_EDGE('',*,*,#4994,.F.);
#6832=ORIENTED_EDGE('',*,*,#4983,.F.);
#6833=ORIENTED_EDGE('',*,*,#4995,.T.);
#6834=ORIENTED_EDGE('',*,*,#4968,.T.);
#6835=ORIENTED_EDGE('',*,*,#4975,.T.);
#6836=ORIENTED_EDGE('',*,*,#4994,.T.);
#6837=ORIENTED_EDGE('',*,*,#4991,.T.);
#6838=ORIENTED_EDGE('',*,*,#4987,.T.);
#6839=ORIENTED_EDGE('',*,*,#4984,.T.);
#6840=ORIENTED_EDGE('',*,*,#4923,.T.);
#6841=ORIENTED_EDGE('',*,*,#4834,.T.);
#6842=ORIENTED_EDGE('',*,*,#4920,.T.);
#6843=ORIENTED_EDGE('',*,*,#4875,.T.);
#6844=ORIENTED_EDGE('',*,*,#4931,.T.);
#6845=ORIENTED_EDGE('',*,*,#4752,.T.);
#6846=ORIENTED_EDGE('',*,*,#4928,.T.);
#6847=ORIENTED_EDGE('',*,*,#4793,.T.);
#6848=ORIENTED_EDGE('',*,*,#4939,.T.);
#6849=ORIENTED_EDGE('',*,*,#4670,.T.);
#6850=ORIENTED_EDGE('',*,*,#4936,.T.);
#6851=ORIENTED_EDGE('',*,*,#4711,.T.);
#6852=ORIENTED_EDGE('',*,*,#4947,.T.);
#6853=ORIENTED_EDGE('',*,*,#4588,.T.);
#6854=ORIENTED_EDGE('',*,*,#4944,.T.);
#6855=ORIENTED_EDGE('',*,*,#4629,.T.);
#6856=ORIENTED_EDGE('',*,*,#4900,.T.);
#6857=ORIENTED_EDGE('',*,*,#4892,.F.);
#6858=ORIENTED_EDGE('',*,*,#4981,.T.);
#6859=ORIENTED_EDGE('',*,*,#4879,.F.);
#6860=ORIENTED_EDGE('',*,*,#4883,.T.);
#6861=ORIENTED_EDGE('',*,*,#4886,.F.);
#6862=ORIENTED_EDGE('',*,*,#4889,.T.);
#6863=ORIENTED_EDGE('',*,*,#4903,.F.);
#6864=ORIENTED_EDGE('',*,*,#4995,.F.);
#6865=ORIENTED_EDGE('',*,*,#4982,.F.);
#6866=ORIENTED_EDGE('',*,*,#4986,.F.);
#6867=ORIENTED_EDGE('',*,*,#4954,.F.);
#6868=ORIENTED_EDGE('',*,*,#4958,.F.);
#6869=ORIENTED_EDGE('',*,*,#4961,.F.);
#6870=ORIENTED_EDGE('',*,*,#4989,.F.);
#6871=ORIENTED_EDGE('',*,*,#4990,.F.);
#6872=ORIENTED_EDGE('',*,*,#4993,.F.);
#6873=ORIENTED_EDGE('',*,*,#4969,.F.);
#6874=ORIENTED_EDGE('',*,*,#4973,.F.);
#6875=ORIENTED_EDGE('',*,*,#4965,.F.);
#6876=ORIENTED_EDGE('',*,*,#4908,.T.);
#6877=ORIENTED_EDGE('',*,*,#4913,.T.);
#6878=ORIENTED_EDGE('',*,*,#4950,.T.);
#6879=ORIENTED_EDGE('',*,*,#4953,.T.);
#6880=ORIENTED_EDGE('',*,*,#4996,.F.);
#6881=ORIENTED_EDGE('',*,*,#4997,.T.);
#6882=ORIENTED_EDGE('',*,*,#4998,.F.);
#6883=ORIENTED_EDGE('',*,*,#4997,.F.);
#6884=ORIENTED_EDGE('',*,*,#4999,.F.);
#6885=ORIENTED_EDGE('',*,*,#5000,.T.);
#6886=ORIENTED_EDGE('',*,*,#5001,.F.);
#6887=ORIENTED_EDGE('',*,*,#5000,.F.);
#6888=ORIENTED_EDGE('',*,*,#5002,.F.);
#6889=ORIENTED_EDGE('',*,*,#5003,.T.);
#6890=ORIENTED_EDGE('',*,*,#5004,.F.);
#6891=ORIENTED_EDGE('',*,*,#5003,.F.);
#6892=ORIENTED_EDGE('',*,*,#5005,.F.);
#6893=ORIENTED_EDGE('',*,*,#5006,.T.);
#6894=ORIENTED_EDGE('',*,*,#5007,.F.);
#6895=ORIENTED_EDGE('',*,*,#5006,.F.);
#6896=ORIENTED_EDGE('',*,*,#5008,.F.);
#6897=ORIENTED_EDGE('',*,*,#5009,.T.);
#6898=ORIENTED_EDGE('',*,*,#5010,.F.);
#6899=ORIENTED_EDGE('',*,*,#5009,.F.);
#6900=ORIENTED_EDGE('',*,*,#5011,.T.);
#6901=ORIENTED_EDGE('',*,*,#5012,.T.);
#6902=ORIENTED_EDGE('',*,*,#5013,.F.);
#6903=ORIENTED_EDGE('',*,*,#5014,.F.);
#6904=ORIENTED_EDGE('',*,*,#5015,.T.);
#6905=ORIENTED_EDGE('',*,*,#5014,.T.);
#6906=ORIENTED_EDGE('',*,*,#5016,.F.);
#6907=ORIENTED_EDGE('',*,*,#5017,.F.);
#6908=ORIENTED_EDGE('',*,*,#5018,.T.);
#6909=ORIENTED_EDGE('',*,*,#5017,.T.);
#6910=ORIENTED_EDGE('',*,*,#5019,.F.);
#6911=ORIENTED_EDGE('',*,*,#5020,.F.);
#6912=ORIENTED_EDGE('',*,*,#5021,.T.);
#6913=ORIENTED_EDGE('',*,*,#5020,.T.);
#6914=ORIENTED_EDGE('',*,*,#5022,.F.);
#6915=ORIENTED_EDGE('',*,*,#5012,.F.);
#6916=ORIENTED_EDGE('',*,*,#5022,.T.);
#6917=ORIENTED_EDGE('',*,*,#5019,.T.);
#6918=ORIENTED_EDGE('',*,*,#5016,.T.);
#6919=ORIENTED_EDGE('',*,*,#5013,.T.);
#6920=ORIENTED_EDGE('',*,*,#5008,.T.);
#6921=ORIENTED_EDGE('',*,*,#5005,.T.);
#6922=ORIENTED_EDGE('',*,*,#5002,.T.);
#6923=ORIENTED_EDGE('',*,*,#4999,.T.);
#6924=ORIENTED_EDGE('',*,*,#4996,.T.);
#6925=ORIENTED_EDGE('',*,*,#5021,.F.);
#6926=ORIENTED_EDGE('',*,*,#5011,.F.);
#6927=ORIENTED_EDGE('',*,*,#5015,.F.);
#6928=ORIENTED_EDGE('',*,*,#5018,.F.);
#6929=ORIENTED_EDGE('',*,*,#5010,.T.);
#6930=ORIENTED_EDGE('',*,*,#5007,.T.);
#6931=ORIENTED_EDGE('',*,*,#5004,.T.);
#6932=ORIENTED_EDGE('',*,*,#5001,.T.);
#6933=ORIENTED_EDGE('',*,*,#4998,.T.);
#6934=ORIENTED_EDGE('',*,*,#5023,.T.);
#6935=ORIENTED_EDGE('',*,*,#5024,.F.);
#6936=ORIENTED_EDGE('',*,*,#5023,.F.);
#6937=ORIENTED_EDGE('',*,*,#5025,.T.);
#6938=ORIENTED_EDGE('',*,*,#5026,.T.);
#6939=ORIENTED_EDGE('',*,*,#5025,.F.);
#6940=ORIENTED_EDGE('',*,*,#5026,.F.);
#6941=ORIENTED_EDGE('',*,*,#5027,.F.);
#6942=ORIENTED_EDGE('',*,*,#5028,.F.);
#6943=ORIENTED_EDGE('',*,*,#5029,.T.);
#6944=ORIENTED_EDGE('',*,*,#5027,.T.);
#6945=ORIENTED_EDGE('',*,*,#5029,.F.);
#6946=ORIENTED_EDGE('',*,*,#5030,.F.);
#6947=ORIENTED_EDGE('',*,*,#5031,.T.);
#6948=ORIENTED_EDGE('',*,*,#5024,.T.);
#6949=ORIENTED_EDGE('',*,*,#5031,.F.);
#6950=ORIENTED_EDGE('',*,*,#5030,.T.);
#6951=ORIENTED_EDGE('',*,*,#5028,.T.);
#6952=ORIENTED_EDGE('',*,*,#5032,.T.);
#6953=ORIENTED_EDGE('',*,*,#5033,.T.);
#6954=ORIENTED_EDGE('',*,*,#5034,.F.);
#6955=ORIENTED_EDGE('',*,*,#5035,.T.);
#6956=ORIENTED_EDGE('',*,*,#5036,.T.);
#6957=ORIENTED_EDGE('',*,*,#5037,.T.);
#6958=ORIENTED_EDGE('',*,*,#5032,.F.);
#6959=ORIENTED_EDGE('',*,*,#5038,.T.);
#6960=ORIENTED_EDGE('',*,*,#5039,.T.);
#6961=ORIENTED_EDGE('',*,*,#5040,.T.);
#6962=ORIENTED_EDGE('',*,*,#5036,.F.);
#6963=ORIENTED_EDGE('',*,*,#5041,.T.);
#6964=ORIENTED_EDGE('',*,*,#5042,.T.);
#6965=ORIENTED_EDGE('',*,*,#5043,.T.);
#6966=ORIENTED_EDGE('',*,*,#5039,.F.);
#6967=ORIENTED_EDGE('',*,*,#5044,.T.);
#6968=ORIENTED_EDGE('',*,*,#5045,.T.);
#6969=ORIENTED_EDGE('',*,*,#5046,.T.);
#6970=ORIENTED_EDGE('',*,*,#5042,.F.);
#6971=ORIENTED_EDGE('',*,*,#5047,.T.);
#6972=ORIENTED_EDGE('',*,*,#5048,.T.);
#6973=ORIENTED_EDGE('',*,*,#5049,.T.);
#6974=ORIENTED_EDGE('',*,*,#5045,.F.);
#6975=ORIENTED_EDGE('',*,*,#5050,.T.);
#6976=ORIENTED_EDGE('',*,*,#5051,.T.);
#6977=ORIENTED_EDGE('',*,*,#5052,.T.);
#6978=ORIENTED_EDGE('',*,*,#5048,.F.);
#6979=ORIENTED_EDGE('',*,*,#5053,.T.);
#6980=ORIENTED_EDGE('',*,*,#5054,.F.);
#6981=ORIENTED_EDGE('',*,*,#5055,.T.);
#6982=ORIENTED_EDGE('',*,*,#5056,.F.);
#6983=ORIENTED_EDGE('',*,*,#5057,.T.);
#6984=ORIENTED_EDGE('',*,*,#5058,.T.);
#6985=ORIENTED_EDGE('',*,*,#5059,.T.);
#6986=ORIENTED_EDGE('',*,*,#5060,.F.);
#6987=ORIENTED_EDGE('',*,*,#5061,.T.);
#6988=ORIENTED_EDGE('',*,*,#5062,.T.);
#6989=ORIENTED_EDGE('',*,*,#5063,.T.);
#6990=ORIENTED_EDGE('',*,*,#5058,.F.);
#6991=ORIENTED_EDGE('',*,*,#5064,.T.);
#6992=ORIENTED_EDGE('',*,*,#5065,.T.);
#6993=ORIENTED_EDGE('',*,*,#5066,.T.);
#6994=ORIENTED_EDGE('',*,*,#5062,.F.);
#6995=ORIENTED_EDGE('',*,*,#5067,.T.);
#6996=ORIENTED_EDGE('',*,*,#5068,.T.);
#6997=ORIENTED_EDGE('',*,*,#5069,.T.);
#6998=ORIENTED_EDGE('',*,*,#5065,.F.);
#6999=ORIENTED_EDGE('',*,*,#5070,.T.);
#7000=ORIENTED_EDGE('',*,*,#5071,.T.);
#7001=ORIENTED_EDGE('',*,*,#5072,.T.);
#7002=ORIENTED_EDGE('',*,*,#5068,.F.);
#7003=ORIENTED_EDGE('',*,*,#5073,.T.);
#7004=ORIENTED_EDGE('',*,*,#5074,.T.);
#7005=ORIENTED_EDGE('',*,*,#5075,.T.);
#7006=ORIENTED_EDGE('',*,*,#5071,.F.);
#7007=ORIENTED_EDGE('',*,*,#5076,.T.);
#7008=ORIENTED_EDGE('',*,*,#5077,.T.);
#7009=ORIENTED_EDGE('',*,*,#5078,.T.);
#7010=ORIENTED_EDGE('',*,*,#5074,.F.);
#7011=ORIENTED_EDGE('',*,*,#5079,.T.);
#7012=ORIENTED_EDGE('',*,*,#5080,.F.);
#7013=ORIENTED_EDGE('',*,*,#5081,.T.);
#7014=ORIENTED_EDGE('',*,*,#5082,.F.);
#7015=ORIENTED_EDGE('',*,*,#5083,.T.);
#7016=ORIENTED_EDGE('',*,*,#5084,.T.);
#7017=ORIENTED_EDGE('',*,*,#5085,.T.);
#7018=ORIENTED_EDGE('',*,*,#5086,.F.);
#7019=ORIENTED_EDGE('',*,*,#5087,.F.);
#7020=ORIENTED_EDGE('',*,*,#5088,.T.);
#7021=ORIENTED_EDGE('',*,*,#5089,.T.);
#7022=ORIENTED_EDGE('',*,*,#5084,.F.);
#7023=ORIENTED_EDGE('',*,*,#5090,.F.);
#7024=ORIENTED_EDGE('',*,*,#5091,.T.);
#7025=ORIENTED_EDGE('',*,*,#5092,.T.);
#7026=ORIENTED_EDGE('',*,*,#5088,.F.);
#7027=ORIENTED_EDGE('',*,*,#5093,.F.);
#7028=ORIENTED_EDGE('',*,*,#5094,.T.);
#7029=ORIENTED_EDGE('',*,*,#5095,.T.);
#7030=ORIENTED_EDGE('',*,*,#5091,.F.);
#7031=ORIENTED_EDGE('',*,*,#5096,.F.);
#7032=ORIENTED_EDGE('',*,*,#5097,.T.);
#7033=ORIENTED_EDGE('',*,*,#5098,.T.);
#7034=ORIENTED_EDGE('',*,*,#5094,.F.);
#7035=ORIENTED_EDGE('',*,*,#5099,.F.);
#7036=ORIENTED_EDGE('',*,*,#5100,.T.);
#7037=ORIENTED_EDGE('',*,*,#5101,.T.);
#7038=ORIENTED_EDGE('',*,*,#5097,.F.);
#7039=ORIENTED_EDGE('',*,*,#5102,.F.);
#7040=ORIENTED_EDGE('',*,*,#5103,.T.);
#7041=ORIENTED_EDGE('',*,*,#5104,.T.);
#7042=ORIENTED_EDGE('',*,*,#5100,.F.);
#7043=ORIENTED_EDGE('',*,*,#5105,.F.);
#7044=ORIENTED_EDGE('',*,*,#5106,.F.);
#7045=ORIENTED_EDGE('',*,*,#5107,.F.);
#7046=ORIENTED_EDGE('',*,*,#5108,.F.);
#7047=ORIENTED_EDGE('',*,*,#5109,.T.);
#7048=ORIENTED_EDGE('',*,*,#5110,.T.);
#7049=ORIENTED_EDGE('',*,*,#5111,.T.);
#7050=ORIENTED_EDGE('',*,*,#5112,.F.);
#7051=ORIENTED_EDGE('',*,*,#5113,.F.);
#7052=ORIENTED_EDGE('',*,*,#5114,.T.);
#7053=ORIENTED_EDGE('',*,*,#5115,.T.);
#7054=ORIENTED_EDGE('',*,*,#5110,.F.);
#7055=ORIENTED_EDGE('',*,*,#5116,.F.);
#7056=ORIENTED_EDGE('',*,*,#5117,.T.);
#7057=ORIENTED_EDGE('',*,*,#5118,.T.);
#7058=ORIENTED_EDGE('',*,*,#5114,.F.);
#7059=ORIENTED_EDGE('',*,*,#5119,.F.);
#7060=ORIENTED_EDGE('',*,*,#5120,.T.);
#7061=ORIENTED_EDGE('',*,*,#5121,.T.);
#7062=ORIENTED_EDGE('',*,*,#5117,.F.);
#7063=ORIENTED_EDGE('',*,*,#5122,.F.);
#7064=ORIENTED_EDGE('',*,*,#5123,.T.);
#7065=ORIENTED_EDGE('',*,*,#5124,.T.);
#7066=ORIENTED_EDGE('',*,*,#5120,.F.);
#7067=ORIENTED_EDGE('',*,*,#5125,.F.);
#7068=ORIENTED_EDGE('',*,*,#5126,.T.);
#7069=ORIENTED_EDGE('',*,*,#5127,.T.);
#7070=ORIENTED_EDGE('',*,*,#5123,.F.);
#7071=ORIENTED_EDGE('',*,*,#5128,.F.);
#7072=ORIENTED_EDGE('',*,*,#5129,.T.);
#7073=ORIENTED_EDGE('',*,*,#5130,.T.);
#7074=ORIENTED_EDGE('',*,*,#5126,.F.);
#7075=ORIENTED_EDGE('',*,*,#5131,.F.);
#7076=ORIENTED_EDGE('',*,*,#5132,.F.);
#7077=ORIENTED_EDGE('',*,*,#5133,.F.);
#7078=ORIENTED_EDGE('',*,*,#5134,.F.);
#7079=ORIENTED_EDGE('',*,*,#5135,.T.);
#7080=ORIENTED_EDGE('',*,*,#5132,.T.);
#7081=ORIENTED_EDGE('',*,*,#5136,.T.);
#7082=ORIENTED_EDGE('',*,*,#5129,.F.);
#7083=ORIENTED_EDGE('',*,*,#5137,.F.);
#7084=ORIENTED_EDGE('',*,*,#5138,.F.);
#7085=ORIENTED_EDGE('',*,*,#5111,.F.);
#7086=ORIENTED_EDGE('',*,*,#5115,.F.);
#7087=ORIENTED_EDGE('',*,*,#5118,.F.);
#7088=ORIENTED_EDGE('',*,*,#5121,.F.);
#7089=ORIENTED_EDGE('',*,*,#5124,.F.);
#7090=ORIENTED_EDGE('',*,*,#5127,.F.);
#7091=ORIENTED_EDGE('',*,*,#5130,.F.);
#7092=ORIENTED_EDGE('',*,*,#5136,.F.);
#7093=ORIENTED_EDGE('',*,*,#5135,.F.);
#7094=ORIENTED_EDGE('',*,*,#5139,.F.);
#7095=ORIENTED_EDGE('',*,*,#5081,.F.);
#7096=ORIENTED_EDGE('',*,*,#5140,.F.);
#7097=ORIENTED_EDGE('',*,*,#5079,.F.);
#7098=ORIENTED_EDGE('',*,*,#5076,.F.);
#7099=ORIENTED_EDGE('',*,*,#5073,.F.);
#7100=ORIENTED_EDGE('',*,*,#5070,.F.);
#7101=ORIENTED_EDGE('',*,*,#5067,.F.);
#7102=ORIENTED_EDGE('',*,*,#5064,.F.);
#7103=ORIENTED_EDGE('',*,*,#5061,.F.);
#7104=ORIENTED_EDGE('',*,*,#5141,.F.);
#7105=ORIENTED_EDGE('',*,*,#5059,.F.);
#7106=ORIENTED_EDGE('',*,*,#5063,.F.);
#7107=ORIENTED_EDGE('',*,*,#5066,.F.);
#7108=ORIENTED_EDGE('',*,*,#5069,.F.);
#7109=ORIENTED_EDGE('',*,*,#5072,.F.);
#7110=ORIENTED_EDGE('',*,*,#5075,.F.);
#7111=ORIENTED_EDGE('',*,*,#5078,.F.);
#7112=ORIENTED_EDGE('',*,*,#5142,.F.);
#7113=ORIENTED_EDGE('',*,*,#5083,.F.);
#7114=ORIENTED_EDGE('',*,*,#5143,.F.);
#7115=ORIENTED_EDGE('',*,*,#5133,.T.);
#7116=ORIENTED_EDGE('',*,*,#5137,.T.);
#7117=ORIENTED_EDGE('',*,*,#5131,.T.);
#7118=ORIENTED_EDGE('',*,*,#5128,.T.);
#7119=ORIENTED_EDGE('',*,*,#5125,.T.);
#7120=ORIENTED_EDGE('',*,*,#5122,.T.);
#7121=ORIENTED_EDGE('',*,*,#5119,.T.);
#7122=ORIENTED_EDGE('',*,*,#5116,.T.);
#7123=ORIENTED_EDGE('',*,*,#5113,.T.);
#7124=ORIENTED_EDGE('',*,*,#5144,.F.);
#7125=ORIENTED_EDGE('',*,*,#5145,.F.);
#7126=ORIENTED_EDGE('',*,*,#5146,.F.);
#7127=ORIENTED_EDGE('',*,*,#5147,.F.);
#7128=ORIENTED_EDGE('',*,*,#5148,.F.);
#7129=ORIENTED_EDGE('',*,*,#5149,.F.);
#7130=ORIENTED_EDGE('',*,*,#5141,.T.);
#7131=ORIENTED_EDGE('',*,*,#5112,.T.);
#7132=ORIENTED_EDGE('',*,*,#5138,.T.);
#7133=ORIENTED_EDGE('',*,*,#5060,.T.);
#7134=ORIENTED_EDGE('',*,*,#5150,.T.);
#7135=ORIENTED_EDGE('',*,*,#5086,.T.);
#7136=ORIENTED_EDGE('',*,*,#5151,.T.);
#7137=ORIENTED_EDGE('',*,*,#5034,.T.);
#7138=ORIENTED_EDGE('',*,*,#5106,.T.);
#7139=ORIENTED_EDGE('',*,*,#5152,.T.);
#7140=ORIENTED_EDGE('',*,*,#5103,.F.);
#7141=ORIENTED_EDGE('',*,*,#5153,.F.);
#7142=ORIENTED_EDGE('',*,*,#5151,.F.);
#7143=ORIENTED_EDGE('',*,*,#5085,.F.);
#7144=ORIENTED_EDGE('',*,*,#5089,.F.);
#7145=ORIENTED_EDGE('',*,*,#5092,.F.);
#7146=ORIENTED_EDGE('',*,*,#5095,.F.);
#7147=ORIENTED_EDGE('',*,*,#5098,.F.);
#7148=ORIENTED_EDGE('',*,*,#5101,.F.);
#7149=ORIENTED_EDGE('',*,*,#5104,.F.);
#7150=ORIENTED_EDGE('',*,*,#5152,.F.);
#7151=ORIENTED_EDGE('',*,*,#5109,.F.);
#7152=ORIENTED_EDGE('',*,*,#5154,.F.);
#7153=ORIENTED_EDGE('',*,*,#5055,.F.);
#7154=ORIENTED_EDGE('',*,*,#5155,.F.);
#7155=ORIENTED_EDGE('',*,*,#5053,.F.);
#7156=ORIENTED_EDGE('',*,*,#5050,.F.);
#7157=ORIENTED_EDGE('',*,*,#5047,.F.);
#7158=ORIENTED_EDGE('',*,*,#5044,.F.);
#7159=ORIENTED_EDGE('',*,*,#5041,.F.);
#7160=ORIENTED_EDGE('',*,*,#5038,.F.);
#7161=ORIENTED_EDGE('',*,*,#5035,.F.);
#7162=ORIENTED_EDGE('',*,*,#5150,.F.);
#7163=ORIENTED_EDGE('',*,*,#5033,.F.);
#7164=ORIENTED_EDGE('',*,*,#5037,.F.);
#7165=ORIENTED_EDGE('',*,*,#5040,.F.);
#7166=ORIENTED_EDGE('',*,*,#5043,.F.);
#7167=ORIENTED_EDGE('',*,*,#5046,.F.);
#7168=ORIENTED_EDGE('',*,*,#5049,.F.);
#7169=ORIENTED_EDGE('',*,*,#5052,.F.);
#7170=ORIENTED_EDGE('',*,*,#5156,.F.);
#7171=ORIENTED_EDGE('',*,*,#5057,.F.);
#7172=ORIENTED_EDGE('',*,*,#5157,.F.);
#7173=ORIENTED_EDGE('',*,*,#5107,.T.);
#7174=ORIENTED_EDGE('',*,*,#5153,.T.);
#7175=ORIENTED_EDGE('',*,*,#5105,.T.);
#7176=ORIENTED_EDGE('',*,*,#5102,.T.);
#7177=ORIENTED_EDGE('',*,*,#5099,.T.);
#7178=ORIENTED_EDGE('',*,*,#5096,.T.);
#7179=ORIENTED_EDGE('',*,*,#5093,.T.);
#7180=ORIENTED_EDGE('',*,*,#5090,.T.);
#7181=ORIENTED_EDGE('',*,*,#5087,.T.);
#7182=ORIENTED_EDGE('',*,*,#5080,.T.);
#7183=ORIENTED_EDGE('',*,*,#5142,.T.);
#7184=ORIENTED_EDGE('',*,*,#5077,.F.);
#7185=ORIENTED_EDGE('',*,*,#5140,.T.);
#7186=ORIENTED_EDGE('',*,*,#5054,.T.);
#7187=ORIENTED_EDGE('',*,*,#5156,.T.);
#7188=ORIENTED_EDGE('',*,*,#5051,.F.);
#7189=ORIENTED_EDGE('',*,*,#5155,.T.);
#7190=ORIENTED_EDGE('',*,*,#5158,.F.);
#7191=ORIENTED_EDGE('',*,*,#5159,.T.);
#7192=ORIENTED_EDGE('',*,*,#5160,.F.);
#7193=ORIENTED_EDGE('',*,*,#5159,.F.);
#7194=ORIENTED_EDGE('',*,*,#5161,.F.);
#7195=ORIENTED_EDGE('',*,*,#5162,.T.);
#7196=ORIENTED_EDGE('',*,*,#5163,.F.);
#7197=ORIENTED_EDGE('',*,*,#5162,.F.);
#7198=ORIENTED_EDGE('',*,*,#5164,.F.);
#7199=ORIENTED_EDGE('',*,*,#5165,.T.);
#7200=ORIENTED_EDGE('',*,*,#5166,.F.);
#7201=ORIENTED_EDGE('',*,*,#5167,.F.);
#7202=ORIENTED_EDGE('',*,*,#5163,.T.);
#7203=ORIENTED_EDGE('',*,*,#5166,.T.);
#7204=ORIENTED_EDGE('',*,*,#5168,.T.);
#7205=ORIENTED_EDGE('',*,*,#5169,.T.);
#7206=ORIENTED_EDGE('',*,*,#5170,.T.);
#7207=ORIENTED_EDGE('',*,*,#5171,.T.);
#7208=ORIENTED_EDGE('',*,*,#5168,.F.);
#7209=ORIENTED_EDGE('',*,*,#5165,.F.);
#7210=ORIENTED_EDGE('',*,*,#5172,.F.);
#7211=ORIENTED_EDGE('',*,*,#5173,.T.);
#7212=ORIENTED_EDGE('',*,*,#5174,.F.);
#7213=ORIENTED_EDGE('',*,*,#5175,.F.);
#7214=ORIENTED_EDGE('',*,*,#5176,.T.);
#7215=ORIENTED_EDGE('',*,*,#5177,.T.);
#7216=ORIENTED_EDGE('',*,*,#5164,.T.);
#7217=ORIENTED_EDGE('',*,*,#5178,.T.);
#7218=ORIENTED_EDGE('',*,*,#5179,.T.);
#7219=ORIENTED_EDGE('',*,*,#5172,.T.);
#7220=ORIENTED_EDGE('',*,*,#5179,.F.);
#7221=ORIENTED_EDGE('',*,*,#5180,.T.);
#7222=ORIENTED_EDGE('',*,*,#5181,.F.);
#7223=ORIENTED_EDGE('',*,*,#5173,.F.);
#7224=ORIENTED_EDGE('',*,*,#5158,.T.);
#7225=ORIENTED_EDGE('',*,*,#5182,.T.);
#7226=ORIENTED_EDGE('',*,*,#5174,.T.);
#7227=ORIENTED_EDGE('',*,*,#5181,.T.);
#7228=ORIENTED_EDGE('',*,*,#5183,.T.);
#7229=ORIENTED_EDGE('',*,*,#5184,.F.);
#7230=ORIENTED_EDGE('',*,*,#5185,.F.);
#7231=ORIENTED_EDGE('',*,*,#5186,.F.);
#7232=ORIENTED_EDGE('',*,*,#5177,.F.);
#7233=ORIENTED_EDGE('',*,*,#5187,.F.);
#7234=ORIENTED_EDGE('',*,*,#5176,.F.);
#7235=ORIENTED_EDGE('',*,*,#5188,.F.);
#7236=ORIENTED_EDGE('',*,*,#5189,.F.);
#7237=ORIENTED_EDGE('',*,*,#5190,.F.);
#7238=ORIENTED_EDGE('',*,*,#5191,.F.);
#7239=ORIENTED_EDGE('',*,*,#5185,.T.);
#7240=ORIENTED_EDGE('',*,*,#5189,.T.);
#7241=ORIENTED_EDGE('',*,*,#5192,.T.);
#7242=ORIENTED_EDGE('',*,*,#5183,.F.);
#7243=ORIENTED_EDGE('',*,*,#5180,.F.);
#7244=ORIENTED_EDGE('',*,*,#5178,.F.);
#7245=ORIENTED_EDGE('',*,*,#5167,.T.);
#7246=ORIENTED_EDGE('',*,*,#5170,.F.);
#7247=ORIENTED_EDGE('',*,*,#5171,.F.);
#7248=ORIENTED_EDGE('',*,*,#5186,.T.);
#7249=ORIENTED_EDGE('',*,*,#5191,.T.);
#7250=ORIENTED_EDGE('',*,*,#5169,.F.);
#7251=ORIENTED_EDGE('',*,*,#5161,.T.);
#7252=ORIENTED_EDGE('',*,*,#5192,.F.);
#7253=ORIENTED_EDGE('',*,*,#5188,.T.);
#7254=ORIENTED_EDGE('',*,*,#5175,.T.);
#7255=ORIENTED_EDGE('',*,*,#5182,.F.);
#7256=ORIENTED_EDGE('',*,*,#5160,.T.);
#7257=ORIENTED_EDGE('',*,*,#5193,.F.);
#7258=ORIENTED_EDGE('',*,*,#5149,.T.);
#7259=ORIENTED_EDGE('',*,*,#5194,.T.);
#7260=ORIENTED_EDGE('',*,*,#5195,.F.);
#7261=ORIENTED_EDGE('',*,*,#5147,.T.);
#7262=ORIENTED_EDGE('',*,*,#5196,.T.);
#7263=ORIENTED_EDGE('',*,*,#5197,.F.);
#7264=ORIENTED_EDGE('',*,*,#5198,.F.);
#7265=ORIENTED_EDGE('',*,*,#5148,.T.);
#7266=ORIENTED_EDGE('',*,*,#5198,.T.);
#7267=ORIENTED_EDGE('',*,*,#5199,.F.);
#7268=ORIENTED_EDGE('',*,*,#5194,.F.);
#7269=ORIENTED_EDGE('',*,*,#5200,.F.);
#7270=ORIENTED_EDGE('',*,*,#5201,.F.);
#7271=ORIENTED_EDGE('',*,*,#5202,.F.);
#7272=ORIENTED_EDGE('',*,*,#5145,.T.);
#7273=ORIENTED_EDGE('',*,*,#5146,.T.);
#7274=ORIENTED_EDGE('',*,*,#5202,.T.);
#7275=ORIENTED_EDGE('',*,*,#5203,.F.);
#7276=ORIENTED_EDGE('',*,*,#5196,.F.);
#7277=ORIENTED_EDGE('',*,*,#5200,.T.);
#7278=ORIENTED_EDGE('',*,*,#5144,.T.);
#7279=ORIENTED_EDGE('',*,*,#5193,.T.);
#7280=ORIENTED_EDGE('',*,*,#5204,.F.);
#7281=ORIENTED_EDGE('',*,*,#5187,.T.);
#7282=ORIENTED_EDGE('',*,*,#5205,.T.);
#7283=ORIENTED_EDGE('',*,*,#5206,.F.);
#7284=ORIENTED_EDGE('',*,*,#5205,.F.);
#7285=ORIENTED_EDGE('',*,*,#5190,.T.);
#7286=ORIENTED_EDGE('',*,*,#5184,.T.);
#7287=ORIENTED_EDGE('',*,*,#5204,.T.);
#7288=ORIENTED_EDGE('',*,*,#5195,.T.);
#7289=ORIENTED_EDGE('',*,*,#5199,.T.);
#7290=ORIENTED_EDGE('',*,*,#5197,.T.);
#7291=ORIENTED_EDGE('',*,*,#5203,.T.);
#7292=ORIENTED_EDGE('',*,*,#5201,.T.);
#7293=ORIENTED_EDGE('',*,*,#5143,.T.);
#7294=ORIENTED_EDGE('',*,*,#5082,.T.);
#7295=ORIENTED_EDGE('',*,*,#5139,.T.);
#7296=ORIENTED_EDGE('',*,*,#5134,.T.);
#7297=ORIENTED_EDGE('',*,*,#5157,.T.);
#7298=ORIENTED_EDGE('',*,*,#5056,.T.);
#7299=ORIENTED_EDGE('',*,*,#5154,.T.);
#7300=ORIENTED_EDGE('',*,*,#5108,.T.);
#7301=ORIENTED_EDGE('',*,*,#5206,.T.);
#7302=ORIENTED_EDGE('',*,*,#5207,.F.);
#7303=ORIENTED_EDGE('',*,*,#5208,.T.);
#7304=ORIENTED_EDGE('',*,*,#5209,.F.);
#7305=ORIENTED_EDGE('',*,*,#5208,.F.);
#7306=ORIENTED_EDGE('',*,*,#5210,.F.);
#7307=ORIENTED_EDGE('',*,*,#5211,.T.);
#7308=ORIENTED_EDGE('',*,*,#5212,.F.);
#7309=ORIENTED_EDGE('',*,*,#5211,.F.);
#7310=ORIENTED_EDGE('',*,*,#5213,.T.);
#7311=ORIENTED_EDGE('',*,*,#5214,.T.);
#7312=ORIENTED_EDGE('',*,*,#5215,.F.);
#7313=ORIENTED_EDGE('',*,*,#5216,.F.);
#7314=ORIENTED_EDGE('',*,*,#5217,.T.);
#7315=ORIENTED_EDGE('',*,*,#5216,.T.);
#7316=ORIENTED_EDGE('',*,*,#5218,.F.);
#7317=ORIENTED_EDGE('',*,*,#5219,.F.);
#7318=ORIENTED_EDGE('',*,*,#5220,.T.);
#7319=ORIENTED_EDGE('',*,*,#5219,.T.);
#7320=ORIENTED_EDGE('',*,*,#5221,.F.);
#7321=ORIENTED_EDGE('',*,*,#5222,.F.);
#7322=ORIENTED_EDGE('',*,*,#5223,.T.);
#7323=ORIENTED_EDGE('',*,*,#5222,.T.);
#7324=ORIENTED_EDGE('',*,*,#5224,.F.);
#7325=ORIENTED_EDGE('',*,*,#5214,.F.);
#7326=ORIENTED_EDGE('',*,*,#5224,.T.);
#7327=ORIENTED_EDGE('',*,*,#5221,.T.);
#7328=ORIENTED_EDGE('',*,*,#5218,.T.);
#7329=ORIENTED_EDGE('',*,*,#5215,.T.);
#7330=ORIENTED_EDGE('',*,*,#5207,.T.);
#7331=ORIENTED_EDGE('',*,*,#5210,.T.);
#7332=ORIENTED_EDGE('',*,*,#5223,.F.);
#7333=ORIENTED_EDGE('',*,*,#5213,.F.);
#7334=ORIENTED_EDGE('',*,*,#5217,.F.);
#7335=ORIENTED_EDGE('',*,*,#5220,.F.);
#7336=ORIENTED_EDGE('',*,*,#5209,.T.);
#7337=ORIENTED_EDGE('',*,*,#5212,.T.);
#7338=ORIENTED_EDGE('',*,*,#5225,.T.);
#7339=ORIENTED_EDGE('',*,*,#5226,.T.);
#7340=ORIENTED_EDGE('',*,*,#5227,.T.);
#7341=ORIENTED_EDGE('',*,*,#5226,.F.);
#7342=ORIENTED_EDGE('',*,*,#5228,.F.);
#7343=ORIENTED_EDGE('',*,*,#5229,.T.);
#7344=ORIENTED_EDGE('',*,*,#5225,.F.);
#7345=ORIENTED_EDGE('',*,*,#5229,.F.);
#7346=ORIENTED_EDGE('',*,*,#5227,.F.);
#7347=ORIENTED_EDGE('',*,*,#5230,.F.);
#7348=ORIENTED_EDGE('',*,*,#5231,.T.);
#7349=ORIENTED_EDGE('',*,*,#5232,.T.);
#7350=ORIENTED_EDGE('',*,*,#5228,.T.);
#7351=ORIENTED_EDGE('',*,*,#5232,.F.);
#7352=ORIENTED_EDGE('',*,*,#5231,.F.);
#7353=ORIENTED_EDGE('',*,*,#5233,.F.);
#7354=ORIENTED_EDGE('',*,*,#5234,.T.);
#7355=ORIENTED_EDGE('',*,*,#5235,.T.);
#7356=ORIENTED_EDGE('',*,*,#5230,.T.);
#7357=ORIENTED_EDGE('',*,*,#5235,.F.);
#7358=ORIENTED_EDGE('',*,*,#5236,.F.);
#7359=ORIENTED_EDGE('',*,*,#5237,.T.);
#7360=ORIENTED_EDGE('',*,*,#5234,.F.);
#7361=ORIENTED_EDGE('',*,*,#5237,.F.);
#7362=ORIENTED_EDGE('',*,*,#5233,.T.);
#7363=ORIENTED_EDGE('',*,*,#5238,.T.);
#7364=ORIENTED_EDGE('',*,*,#5236,.T.);
#7365=ORIENTED_EDGE('',*,*,#5238,.F.);
#7366=ORIENTED_EDGE('',*,*,#5239,.T.);
#7367=ORIENTED_EDGE('',*,*,#5240,.T.);
#7368=ORIENTED_EDGE('',*,*,#5241,.T.);
#7369=ORIENTED_EDGE('',*,*,#5242,.T.);
#7370=ORIENTED_EDGE('',*,*,#5243,.T.);
#7371=ORIENTED_EDGE('',*,*,#5244,.T.);
#7372=ORIENTED_EDGE('',*,*,#5243,.F.);
#7373=ORIENTED_EDGE('',*,*,#5245,.T.);
#7374=ORIENTED_EDGE('',*,*,#5246,.T.);
#7375=ORIENTED_EDGE('',*,*,#5247,.T.);
#7376=ORIENTED_EDGE('',*,*,#5239,.F.);
#7377=ORIENTED_EDGE('',*,*,#5248,.T.);
#7378=ORIENTED_EDGE('',*,*,#5249,.T.);
#7379=ORIENTED_EDGE('',*,*,#5250,.T.);
#7380=ORIENTED_EDGE('',*,*,#5246,.F.);
#7381=ORIENTED_EDGE('',*,*,#5251,.T.);
#7382=ORIENTED_EDGE('',*,*,#5252,.T.);
#7383=ORIENTED_EDGE('',*,*,#5253,.T.);
#7384=ORIENTED_EDGE('',*,*,#5249,.F.);
#7385=ORIENTED_EDGE('',*,*,#5254,.T.);
#7386=ORIENTED_EDGE('',*,*,#5255,.T.);
#7387=ORIENTED_EDGE('',*,*,#5256,.T.);
#7388=ORIENTED_EDGE('',*,*,#5252,.F.);
#7389=ORIENTED_EDGE('',*,*,#5257,.T.);
#7390=ORIENTED_EDGE('',*,*,#5258,.T.);
#7391=ORIENTED_EDGE('',*,*,#5259,.T.);
#7392=ORIENTED_EDGE('',*,*,#5255,.F.);
#7393=ORIENTED_EDGE('',*,*,#5260,.T.);
#7394=ORIENTED_EDGE('',*,*,#5261,.T.);
#7395=ORIENTED_EDGE('',*,*,#5262,.T.);
#7396=ORIENTED_EDGE('',*,*,#5258,.F.);
#7397=ORIENTED_EDGE('',*,*,#5263,.T.);
#7398=ORIENTED_EDGE('',*,*,#5264,.T.);
#7399=ORIENTED_EDGE('',*,*,#5265,.T.);
#7400=ORIENTED_EDGE('',*,*,#5261,.F.);
#7401=ORIENTED_EDGE('',*,*,#5266,.T.);
#7402=ORIENTED_EDGE('',*,*,#5267,.T.);
#7403=ORIENTED_EDGE('',*,*,#5268,.T.);
#7404=ORIENTED_EDGE('',*,*,#5264,.F.);
#7405=ORIENTED_EDGE('',*,*,#5269,.T.);
#7406=ORIENTED_EDGE('',*,*,#5270,.T.);
#7407=ORIENTED_EDGE('',*,*,#5271,.T.);
#7408=ORIENTED_EDGE('',*,*,#5267,.F.);
#7409=ORIENTED_EDGE('',*,*,#5272,.T.);
#7410=ORIENTED_EDGE('',*,*,#5273,.T.);
#7411=ORIENTED_EDGE('',*,*,#5274,.T.);
#7412=ORIENTED_EDGE('',*,*,#5270,.F.);
#7413=ORIENTED_EDGE('',*,*,#5275,.T.);
#7414=ORIENTED_EDGE('',*,*,#5276,.F.);
#7415=ORIENTED_EDGE('',*,*,#5277,.T.);
#7416=ORIENTED_EDGE('',*,*,#5278,.F.);
#7417=ORIENTED_EDGE('',*,*,#5279,.T.);
#7418=ORIENTED_EDGE('',*,*,#5280,.T.);
#7419=ORIENTED_EDGE('',*,*,#5281,.T.);
#7420=ORIENTED_EDGE('',*,*,#5282,.F.);
#7421=ORIENTED_EDGE('',*,*,#5283,.F.);
#7422=ORIENTED_EDGE('',*,*,#5284,.T.);
#7423=ORIENTED_EDGE('',*,*,#5285,.T.);
#7424=ORIENTED_EDGE('',*,*,#5280,.F.);
#7425=ORIENTED_EDGE('',*,*,#5286,.F.);
#7426=ORIENTED_EDGE('',*,*,#5287,.T.);
#7427=ORIENTED_EDGE('',*,*,#5288,.T.);
#7428=ORIENTED_EDGE('',*,*,#5284,.F.);
#7429=ORIENTED_EDGE('',*,*,#5289,.F.);
#7430=ORIENTED_EDGE('',*,*,#5290,.T.);
#7431=ORIENTED_EDGE('',*,*,#5291,.T.);
#7432=ORIENTED_EDGE('',*,*,#5287,.F.);
#7433=ORIENTED_EDGE('',*,*,#5292,.F.);
#7434=ORIENTED_EDGE('',*,*,#5293,.T.);
#7435=ORIENTED_EDGE('',*,*,#5294,.T.);
#7436=ORIENTED_EDGE('',*,*,#5290,.F.);
#7437=ORIENTED_EDGE('',*,*,#5295,.F.);
#7438=ORIENTED_EDGE('',*,*,#5296,.T.);
#7439=ORIENTED_EDGE('',*,*,#5297,.T.);
#7440=ORIENTED_EDGE('',*,*,#5293,.F.);
#7441=ORIENTED_EDGE('',*,*,#5298,.F.);
#7442=ORIENTED_EDGE('',*,*,#5299,.T.);
#7443=ORIENTED_EDGE('',*,*,#5300,.T.);
#7444=ORIENTED_EDGE('',*,*,#5296,.F.);
#7445=ORIENTED_EDGE('',*,*,#5301,.F.);
#7446=ORIENTED_EDGE('',*,*,#5302,.T.);
#7447=ORIENTED_EDGE('',*,*,#5303,.T.);
#7448=ORIENTED_EDGE('',*,*,#5299,.F.);
#7449=ORIENTED_EDGE('',*,*,#5304,.F.);
#7450=ORIENTED_EDGE('',*,*,#5305,.T.);
#7451=ORIENTED_EDGE('',*,*,#5306,.T.);
#7452=ORIENTED_EDGE('',*,*,#5302,.F.);
#7453=ORIENTED_EDGE('',*,*,#5307,.F.);
#7454=ORIENTED_EDGE('',*,*,#5308,.T.);
#7455=ORIENTED_EDGE('',*,*,#5309,.T.);
#7456=ORIENTED_EDGE('',*,*,#5305,.F.);
#7457=ORIENTED_EDGE('',*,*,#5310,.F.);
#7458=ORIENTED_EDGE('',*,*,#5311,.T.);
#7459=ORIENTED_EDGE('',*,*,#5312,.T.);
#7460=ORIENTED_EDGE('',*,*,#5308,.F.);
#7461=ORIENTED_EDGE('',*,*,#5313,.F.);
#7462=ORIENTED_EDGE('',*,*,#5314,.T.);
#7463=ORIENTED_EDGE('',*,*,#5315,.T.);
#7464=ORIENTED_EDGE('',*,*,#5311,.F.);
#7465=ORIENTED_EDGE('',*,*,#5316,.F.);
#7466=ORIENTED_EDGE('',*,*,#5317,.F.);
#7467=ORIENTED_EDGE('',*,*,#5318,.F.);
#7468=ORIENTED_EDGE('',*,*,#5319,.F.);
#7469=ORIENTED_EDGE('',*,*,#5320,.T.);
#7470=ORIENTED_EDGE('',*,*,#5321,.T.);
#7471=ORIENTED_EDGE('',*,*,#5322,.T.);
#7472=ORIENTED_EDGE('',*,*,#5323,.T.);
#7473=ORIENTED_EDGE('',*,*,#5324,.T.);
#7474=ORIENTED_EDGE('',*,*,#5325,.T.);
#7475=ORIENTED_EDGE('',*,*,#5324,.F.);
#7476=ORIENTED_EDGE('',*,*,#5326,.T.);
#7477=ORIENTED_EDGE('',*,*,#5327,.T.);
#7478=ORIENTED_EDGE('',*,*,#5328,.T.);
#7479=ORIENTED_EDGE('',*,*,#5329,.T.);
#7480=ORIENTED_EDGE('',*,*,#5321,.F.);
#7481=ORIENTED_EDGE('',*,*,#5330,.T.);
#7482=ORIENTED_EDGE('',*,*,#5331,.T.);
#7483=ORIENTED_EDGE('',*,*,#5332,.T.);
#7484=ORIENTED_EDGE('',*,*,#5328,.F.);
#7485=ORIENTED_EDGE('',*,*,#5333,.T.);
#7486=ORIENTED_EDGE('',*,*,#5334,.T.);
#7487=ORIENTED_EDGE('',*,*,#5335,.T.);
#7488=ORIENTED_EDGE('',*,*,#5331,.F.);
#7489=ORIENTED_EDGE('',*,*,#5336,.T.);
#7490=ORIENTED_EDGE('',*,*,#5337,.T.);
#7491=ORIENTED_EDGE('',*,*,#5338,.T.);
#7492=ORIENTED_EDGE('',*,*,#5334,.F.);
#7493=ORIENTED_EDGE('',*,*,#5339,.T.);
#7494=ORIENTED_EDGE('',*,*,#5340,.T.);
#7495=ORIENTED_EDGE('',*,*,#5341,.T.);
#7496=ORIENTED_EDGE('',*,*,#5337,.F.);
#7497=ORIENTED_EDGE('',*,*,#5342,.T.);
#7498=ORIENTED_EDGE('',*,*,#5343,.T.);
#7499=ORIENTED_EDGE('',*,*,#5344,.T.);
#7500=ORIENTED_EDGE('',*,*,#5340,.F.);
#7501=ORIENTED_EDGE('',*,*,#5345,.T.);
#7502=ORIENTED_EDGE('',*,*,#5346,.T.);
#7503=ORIENTED_EDGE('',*,*,#5347,.T.);
#7504=ORIENTED_EDGE('',*,*,#5343,.F.);
#7505=ORIENTED_EDGE('',*,*,#5348,.T.);
#7506=ORIENTED_EDGE('',*,*,#5349,.T.);
#7507=ORIENTED_EDGE('',*,*,#5350,.T.);
#7508=ORIENTED_EDGE('',*,*,#5346,.F.);
#7509=ORIENTED_EDGE('',*,*,#5351,.T.);
#7510=ORIENTED_EDGE('',*,*,#5352,.T.);
#7511=ORIENTED_EDGE('',*,*,#5353,.T.);
#7512=ORIENTED_EDGE('',*,*,#5349,.F.);
#7513=ORIENTED_EDGE('',*,*,#5354,.T.);
#7514=ORIENTED_EDGE('',*,*,#5355,.T.);
#7515=ORIENTED_EDGE('',*,*,#5356,.T.);
#7516=ORIENTED_EDGE('',*,*,#5352,.F.);
#7517=ORIENTED_EDGE('',*,*,#5357,.T.);
#7518=ORIENTED_EDGE('',*,*,#5358,.T.);
#7519=ORIENTED_EDGE('',*,*,#5359,.T.);
#7520=ORIENTED_EDGE('',*,*,#5355,.F.);
#7521=ORIENTED_EDGE('',*,*,#5360,.T.);
#7522=ORIENTED_EDGE('',*,*,#5361,.T.);
#7523=ORIENTED_EDGE('',*,*,#5362,.T.);
#7524=ORIENTED_EDGE('',*,*,#5358,.F.);
#7525=ORIENTED_EDGE('',*,*,#5363,.T.);
#7526=ORIENTED_EDGE('',*,*,#5364,.T.);
#7527=ORIENTED_EDGE('',*,*,#5365,.T.);
#7528=ORIENTED_EDGE('',*,*,#5361,.F.);
#7529=ORIENTED_EDGE('',*,*,#5366,.T.);
#7530=ORIENTED_EDGE('',*,*,#5367,.T.);
#7531=ORIENTED_EDGE('',*,*,#5368,.T.);
#7532=ORIENTED_EDGE('',*,*,#5364,.F.);
#7533=ORIENTED_EDGE('',*,*,#5369,.T.);
#7534=ORIENTED_EDGE('',*,*,#5370,.T.);
#7535=ORIENTED_EDGE('',*,*,#5371,.T.);
#7536=ORIENTED_EDGE('',*,*,#5367,.F.);
#7537=ORIENTED_EDGE('',*,*,#5372,.T.);
#7538=ORIENTED_EDGE('',*,*,#5373,.T.);
#7539=ORIENTED_EDGE('',*,*,#5374,.T.);
#7540=ORIENTED_EDGE('',*,*,#5370,.F.);
#7541=ORIENTED_EDGE('',*,*,#5375,.T.);
#7542=ORIENTED_EDGE('',*,*,#5376,.F.);
#7543=ORIENTED_EDGE('',*,*,#5377,.T.);
#7544=ORIENTED_EDGE('',*,*,#5378,.F.);
#7545=ORIENTED_EDGE('',*,*,#5379,.T.);
#7546=ORIENTED_EDGE('',*,*,#5380,.T.);
#7547=ORIENTED_EDGE('',*,*,#5381,.T.);
#7548=ORIENTED_EDGE('',*,*,#5382,.F.);
#7549=ORIENTED_EDGE('',*,*,#5383,.F.);
#7550=ORIENTED_EDGE('',*,*,#5384,.T.);
#7551=ORIENTED_EDGE('',*,*,#5385,.T.);
#7552=ORIENTED_EDGE('',*,*,#5380,.F.);
#7553=ORIENTED_EDGE('',*,*,#5386,.F.);
#7554=ORIENTED_EDGE('',*,*,#5387,.T.);
#7555=ORIENTED_EDGE('',*,*,#5388,.T.);
#7556=ORIENTED_EDGE('',*,*,#5384,.F.);
#7557=ORIENTED_EDGE('',*,*,#5389,.F.);
#7558=ORIENTED_EDGE('',*,*,#5390,.T.);
#7559=ORIENTED_EDGE('',*,*,#5391,.T.);
#7560=ORIENTED_EDGE('',*,*,#5387,.F.);
#7561=ORIENTED_EDGE('',*,*,#5392,.F.);
#7562=ORIENTED_EDGE('',*,*,#5393,.T.);
#7563=ORIENTED_EDGE('',*,*,#5394,.T.);
#7564=ORIENTED_EDGE('',*,*,#5390,.F.);
#7565=ORIENTED_EDGE('',*,*,#5395,.F.);
#7566=ORIENTED_EDGE('',*,*,#5396,.T.);
#7567=ORIENTED_EDGE('',*,*,#5397,.T.);
#7568=ORIENTED_EDGE('',*,*,#5393,.F.);
#7569=ORIENTED_EDGE('',*,*,#5398,.F.);
#7570=ORIENTED_EDGE('',*,*,#5399,.T.);
#7571=ORIENTED_EDGE('',*,*,#5400,.T.);
#7572=ORIENTED_EDGE('',*,*,#5396,.F.);
#7573=ORIENTED_EDGE('',*,*,#5401,.F.);
#7574=ORIENTED_EDGE('',*,*,#5402,.T.);
#7575=ORIENTED_EDGE('',*,*,#5403,.T.);
#7576=ORIENTED_EDGE('',*,*,#5399,.F.);
#7577=ORIENTED_EDGE('',*,*,#5404,.F.);
#7578=ORIENTED_EDGE('',*,*,#5405,.T.);
#7579=ORIENTED_EDGE('',*,*,#5406,.T.);
#7580=ORIENTED_EDGE('',*,*,#5402,.F.);
#7581=ORIENTED_EDGE('',*,*,#5407,.F.);
#7582=ORIENTED_EDGE('',*,*,#5408,.T.);
#7583=ORIENTED_EDGE('',*,*,#5409,.T.);
#7584=ORIENTED_EDGE('',*,*,#5405,.F.);
#7585=ORIENTED_EDGE('',*,*,#5410,.F.);
#7586=ORIENTED_EDGE('',*,*,#5411,.T.);
#7587=ORIENTED_EDGE('',*,*,#5412,.T.);
#7588=ORIENTED_EDGE('',*,*,#5408,.F.);
#7589=ORIENTED_EDGE('',*,*,#5413,.F.);
#7590=ORIENTED_EDGE('',*,*,#5414,.T.);
#7591=ORIENTED_EDGE('',*,*,#5415,.T.);
#7592=ORIENTED_EDGE('',*,*,#5411,.F.);
#7593=ORIENTED_EDGE('',*,*,#5416,.F.);
#7594=ORIENTED_EDGE('',*,*,#5417,.T.);
#7595=ORIENTED_EDGE('',*,*,#5418,.T.);
#7596=ORIENTED_EDGE('',*,*,#5414,.F.);
#7597=ORIENTED_EDGE('',*,*,#5419,.F.);
#7598=ORIENTED_EDGE('',*,*,#5420,.T.);
#7599=ORIENTED_EDGE('',*,*,#5421,.T.);
#7600=ORIENTED_EDGE('',*,*,#5417,.F.);
#7601=ORIENTED_EDGE('',*,*,#5422,.F.);
#7602=ORIENTED_EDGE('',*,*,#5423,.T.);
#7603=ORIENTED_EDGE('',*,*,#5424,.T.);
#7604=ORIENTED_EDGE('',*,*,#5420,.F.);
#7605=ORIENTED_EDGE('',*,*,#5425,.F.);
#7606=ORIENTED_EDGE('',*,*,#5426,.T.);
#7607=ORIENTED_EDGE('',*,*,#5427,.T.);
#7608=ORIENTED_EDGE('',*,*,#5423,.F.);
#7609=ORIENTED_EDGE('',*,*,#5428,.F.);
#7610=ORIENTED_EDGE('',*,*,#5429,.T.);
#7611=ORIENTED_EDGE('',*,*,#5430,.T.);
#7612=ORIENTED_EDGE('',*,*,#5426,.F.);
#7613=ORIENTED_EDGE('',*,*,#5431,.F.);
#7614=ORIENTED_EDGE('',*,*,#5432,.F.);
#7615=ORIENTED_EDGE('',*,*,#5433,.F.);
#7616=ORIENTED_EDGE('',*,*,#5434,.F.);
#7617=ORIENTED_EDGE('',*,*,#5435,.T.);
#7618=ORIENTED_EDGE('',*,*,#5323,.F.);
#7619=ORIENTED_EDGE('',*,*,#5436,.T.);
#7620=ORIENTED_EDGE('',*,*,#5382,.T.);
#7621=ORIENTED_EDGE('',*,*,#5437,.T.);
#7622=ORIENTED_EDGE('',*,*,#5326,.F.);
#7623=ORIENTED_EDGE('',*,*,#5432,.T.);
#7624=ORIENTED_EDGE('',*,*,#5438,.T.);
#7625=ORIENTED_EDGE('',*,*,#5429,.F.);
#7626=ORIENTED_EDGE('',*,*,#5439,.F.);
#7627=ORIENTED_EDGE('',*,*,#5437,.F.);
#7628=ORIENTED_EDGE('',*,*,#5381,.F.);
#7629=ORIENTED_EDGE('',*,*,#5385,.F.);
#7630=ORIENTED_EDGE('',*,*,#5388,.F.);
#7631=ORIENTED_EDGE('',*,*,#5391,.F.);
#7632=ORIENTED_EDGE('',*,*,#5394,.F.);
#7633=ORIENTED_EDGE('',*,*,#5397,.F.);
#7634=ORIENTED_EDGE('',*,*,#5400,.F.);
#7635=ORIENTED_EDGE('',*,*,#5403,.F.);
#7636=ORIENTED_EDGE('',*,*,#5406,.F.);
#7637=ORIENTED_EDGE('',*,*,#5409,.F.);
#7638=ORIENTED_EDGE('',*,*,#5412,.F.);
#7639=ORIENTED_EDGE('',*,*,#5415,.F.);
#7640=ORIENTED_EDGE('',*,*,#5418,.F.);
#7641=ORIENTED_EDGE('',*,*,#5421,.F.);
#7642=ORIENTED_EDGE('',*,*,#5424,.F.);
#7643=ORIENTED_EDGE('',*,*,#5427,.F.);
#7644=ORIENTED_EDGE('',*,*,#5430,.F.);
#7645=ORIENTED_EDGE('',*,*,#5438,.F.);
#7646=ORIENTED_EDGE('',*,*,#5435,.F.);
#7647=ORIENTED_EDGE('',*,*,#5440,.F.);
#7648=ORIENTED_EDGE('',*,*,#5377,.F.);
#7649=ORIENTED_EDGE('',*,*,#5441,.F.);
#7650=ORIENTED_EDGE('',*,*,#5375,.F.);
#7651=ORIENTED_EDGE('',*,*,#5372,.F.);
#7652=ORIENTED_EDGE('',*,*,#5369,.F.);
#7653=ORIENTED_EDGE('',*,*,#5366,.F.);
#7654=ORIENTED_EDGE('',*,*,#5363,.F.);
#7655=ORIENTED_EDGE('',*,*,#5360,.F.);
#7656=ORIENTED_EDGE('',*,*,#5357,.F.);
#7657=ORIENTED_EDGE('',*,*,#5354,.F.);
#7658=ORIENTED_EDGE('',*,*,#5351,.F.);
#7659=ORIENTED_EDGE('',*,*,#5348,.F.);
#7660=ORIENTED_EDGE('',*,*,#5345,.F.);
#7661=ORIENTED_EDGE('',*,*,#5342,.F.);
#7662=ORIENTED_EDGE('',*,*,#5339,.F.);
#7663=ORIENTED_EDGE('',*,*,#5336,.F.);
#7664=ORIENTED_EDGE('',*,*,#5333,.F.);
#7665=ORIENTED_EDGE('',*,*,#5330,.F.);
#7666=ORIENTED_EDGE('',*,*,#5327,.F.);
#7667=ORIENTED_EDGE('',*,*,#5436,.F.);
#7668=ORIENTED_EDGE('',*,*,#5322,.F.);
#7669=ORIENTED_EDGE('',*,*,#5329,.F.);
#7670=ORIENTED_EDGE('',*,*,#5332,.F.);
#7671=ORIENTED_EDGE('',*,*,#5335,.F.);
#7672=ORIENTED_EDGE('',*,*,#5338,.F.);
#7673=ORIENTED_EDGE('',*,*,#5341,.F.);
#7674=ORIENTED_EDGE('',*,*,#5344,.F.);
#7675=ORIENTED_EDGE('',*,*,#5347,.F.);
#7676=ORIENTED_EDGE('',*,*,#5350,.F.);
#7677=ORIENTED_EDGE('',*,*,#5353,.F.);
#7678=ORIENTED_EDGE('',*,*,#5356,.F.);
#7679=ORIENTED_EDGE('',*,*,#5359,.F.);
#7680=ORIENTED_EDGE('',*,*,#5362,.F.);
#7681=ORIENTED_EDGE('',*,*,#5365,.F.);
#7682=ORIENTED_EDGE('',*,*,#5368,.F.);
#7683=ORIENTED_EDGE('',*,*,#5371,.F.);
#7684=ORIENTED_EDGE('',*,*,#5374,.F.);
#7685=ORIENTED_EDGE('',*,*,#5442,.F.);
#7686=ORIENTED_EDGE('',*,*,#5379,.F.);
#7687=ORIENTED_EDGE('',*,*,#5443,.F.);
#7688=ORIENTED_EDGE('',*,*,#5433,.T.);
#7689=ORIENTED_EDGE('',*,*,#5439,.T.);
#7690=ORIENTED_EDGE('',*,*,#5431,.T.);
#7691=ORIENTED_EDGE('',*,*,#5428,.T.);
#7692=ORIENTED_EDGE('',*,*,#5425,.T.);
#7693=ORIENTED_EDGE('',*,*,#5422,.T.);
#7694=ORIENTED_EDGE('',*,*,#5419,.T.);
#7695=ORIENTED_EDGE('',*,*,#5416,.T.);
#7696=ORIENTED_EDGE('',*,*,#5413,.T.);
#7697=ORIENTED_EDGE('',*,*,#5410,.T.);
#7698=ORIENTED_EDGE('',*,*,#5407,.T.);
#7699=ORIENTED_EDGE('',*,*,#5404,.T.);
#7700=ORIENTED_EDGE('',*,*,#5401,.T.);
#7701=ORIENTED_EDGE('',*,*,#5398,.T.);
#7702=ORIENTED_EDGE('',*,*,#5395,.T.);
#7703=ORIENTED_EDGE('',*,*,#5392,.T.);
#7704=ORIENTED_EDGE('',*,*,#5389,.T.);
#7705=ORIENTED_EDGE('',*,*,#5386,.T.);
#7706=ORIENTED_EDGE('',*,*,#5383,.T.);
#7707=ORIENTED_EDGE('',*,*,#5376,.T.);
#7708=ORIENTED_EDGE('',*,*,#5442,.T.);
#7709=ORIENTED_EDGE('',*,*,#5373,.F.);
#7710=ORIENTED_EDGE('',*,*,#5441,.T.);
#7711=ORIENTED_EDGE('',*,*,#5325,.F.);
#7712=ORIENTED_EDGE('',*,*,#5241,.F.);
#7713=ORIENTED_EDGE('',*,*,#5444,.T.);
#7714=ORIENTED_EDGE('',*,*,#5282,.T.);
#7715=ORIENTED_EDGE('',*,*,#5445,.T.);
#7716=ORIENTED_EDGE('',*,*,#5317,.T.);
#7717=ORIENTED_EDGE('',*,*,#5446,.T.);
#7718=ORIENTED_EDGE('',*,*,#5314,.F.);
#7719=ORIENTED_EDGE('',*,*,#5447,.F.);
#7720=ORIENTED_EDGE('',*,*,#5445,.F.);
#7721=ORIENTED_EDGE('',*,*,#5281,.F.);
#7722=ORIENTED_EDGE('',*,*,#5285,.F.);
#7723=ORIENTED_EDGE('',*,*,#5288,.F.);
#7724=ORIENTED_EDGE('',*,*,#5291,.F.);
#7725=ORIENTED_EDGE('',*,*,#5294,.F.);
#7726=ORIENTED_EDGE('',*,*,#5297,.F.);
#7727=ORIENTED_EDGE('',*,*,#5300,.F.);
#7728=ORIENTED_EDGE('',*,*,#5303,.F.);
#7729=ORIENTED_EDGE('',*,*,#5306,.F.);
#7730=ORIENTED_EDGE('',*,*,#5309,.F.);
#7731=ORIENTED_EDGE('',*,*,#5312,.F.);
#7732=ORIENTED_EDGE('',*,*,#5315,.F.);
#7733=ORIENTED_EDGE('',*,*,#5446,.F.);
#7734=ORIENTED_EDGE('',*,*,#5320,.F.);
#7735=ORIENTED_EDGE('',*,*,#5448,.F.);
#7736=ORIENTED_EDGE('',*,*,#5277,.F.);
#7737=ORIENTED_EDGE('',*,*,#5449,.F.);
#7738=ORIENTED_EDGE('',*,*,#5275,.F.);
#7739=ORIENTED_EDGE('',*,*,#5272,.F.);
#7740=ORIENTED_EDGE('',*,*,#5269,.F.);
#7741=ORIENTED_EDGE('',*,*,#5266,.F.);
#7742=ORIENTED_EDGE('',*,*,#5263,.F.);
#7743=ORIENTED_EDGE('',*,*,#5260,.F.);
#7744=ORIENTED_EDGE('',*,*,#5257,.F.);
#7745=ORIENTED_EDGE('',*,*,#5254,.F.);
#7746=ORIENTED_EDGE('',*,*,#5251,.F.);
#7747=ORIENTED_EDGE('',*,*,#5248,.F.);
#7748=ORIENTED_EDGE('',*,*,#5245,.F.);
#7749=ORIENTED_EDGE('',*,*,#5242,.F.);
#7750=ORIENTED_EDGE('',*,*,#5444,.F.);
#7751=ORIENTED_EDGE('',*,*,#5240,.F.);
#7752=ORIENTED_EDGE('',*,*,#5247,.F.);
#7753=ORIENTED_EDGE('',*,*,#5250,.F.);
#7754=ORIENTED_EDGE('',*,*,#5253,.F.);
#7755=ORIENTED_EDGE('',*,*,#5256,.F.);
#7756=ORIENTED_EDGE('',*,*,#5259,.F.);
#7757=ORIENTED_EDGE('',*,*,#5262,.F.);
#7758=ORIENTED_EDGE('',*,*,#5265,.F.);
#7759=ORIENTED_EDGE('',*,*,#5268,.F.);
#7760=ORIENTED_EDGE('',*,*,#5271,.F.);
#7761=ORIENTED_EDGE('',*,*,#5274,.F.);
#7762=ORIENTED_EDGE('',*,*,#5450,.F.);
#7763=ORIENTED_EDGE('',*,*,#5279,.F.);
#7764=ORIENTED_EDGE('',*,*,#5451,.F.);
#7765=ORIENTED_EDGE('',*,*,#5318,.T.);
#7766=ORIENTED_EDGE('',*,*,#5447,.T.);
#7767=ORIENTED_EDGE('',*,*,#5316,.T.);
#7768=ORIENTED_EDGE('',*,*,#5313,.T.);
#7769=ORIENTED_EDGE('',*,*,#5310,.T.);
#7770=ORIENTED_EDGE('',*,*,#5307,.T.);
#7771=ORIENTED_EDGE('',*,*,#5304,.T.);
#7772=ORIENTED_EDGE('',*,*,#5301,.T.);
#7773=ORIENTED_EDGE('',*,*,#5298,.T.);
#7774=ORIENTED_EDGE('',*,*,#5295,.T.);
#7775=ORIENTED_EDGE('',*,*,#5292,.T.);
#7776=ORIENTED_EDGE('',*,*,#5289,.T.);
#7777=ORIENTED_EDGE('',*,*,#5286,.T.);
#7778=ORIENTED_EDGE('',*,*,#5283,.T.);
#7779=ORIENTED_EDGE('',*,*,#5276,.T.);
#7780=ORIENTED_EDGE('',*,*,#5450,.T.);
#7781=ORIENTED_EDGE('',*,*,#5273,.F.);
#7782=ORIENTED_EDGE('',*,*,#5449,.T.);
#7783=ORIENTED_EDGE('',*,*,#5244,.F.);
#7784=ORIENTED_EDGE('',*,*,#5452,.T.);
#7785=ORIENTED_EDGE('',*,*,#5453,.T.);
#7786=ORIENTED_EDGE('',*,*,#5454,.F.);
#7787=ORIENTED_EDGE('',*,*,#5455,.F.);
#7788=ORIENTED_EDGE('',*,*,#5456,.T.);
#7789=ORIENTED_EDGE('',*,*,#5455,.T.);
#7790=ORIENTED_EDGE('',*,*,#5457,.F.);
#7791=ORIENTED_EDGE('',*,*,#5458,.F.);
#7792=ORIENTED_EDGE('',*,*,#5459,.T.);
#7793=ORIENTED_EDGE('',*,*,#5458,.T.);
#7794=ORIENTED_EDGE('',*,*,#5460,.F.);
#7795=ORIENTED_EDGE('',*,*,#5461,.F.);
#7796=ORIENTED_EDGE('',*,*,#5462,.T.);
#7797=ORIENTED_EDGE('',*,*,#5461,.T.);
#7798=ORIENTED_EDGE('',*,*,#5463,.F.);
#7799=ORIENTED_EDGE('',*,*,#5453,.F.);
#7800=ORIENTED_EDGE('',*,*,#5463,.T.);
#7801=ORIENTED_EDGE('',*,*,#5460,.T.);
#7802=ORIENTED_EDGE('',*,*,#5457,.T.);
#7803=ORIENTED_EDGE('',*,*,#5454,.T.);
#7804=ORIENTED_EDGE('',*,*,#5443,.T.);
#7805=ORIENTED_EDGE('',*,*,#5378,.T.);
#7806=ORIENTED_EDGE('',*,*,#5440,.T.);
#7807=ORIENTED_EDGE('',*,*,#5434,.T.);
#7808=ORIENTED_EDGE('',*,*,#5462,.F.);
#7809=ORIENTED_EDGE('',*,*,#5452,.F.);
#7810=ORIENTED_EDGE('',*,*,#5456,.F.);
#7811=ORIENTED_EDGE('',*,*,#5459,.F.);
#7812=ORIENTED_EDGE('',*,*,#5451,.T.);
#7813=ORIENTED_EDGE('',*,*,#5278,.T.);
#7814=ORIENTED_EDGE('',*,*,#5448,.T.);
#7815=ORIENTED_EDGE('',*,*,#5319,.T.);
#7816=ORIENTED_EDGE('',*,*,#5464,.T.);
#7817=ORIENTED_EDGE('',*,*,#5465,.T.);
#7818=ORIENTED_EDGE('',*,*,#5466,.T.);
#7819=ORIENTED_EDGE('',*,*,#5467,.T.);
#7820=ORIENTED_EDGE('',*,*,#5468,.T.);
#7821=ORIENTED_EDGE('',*,*,#5467,.F.);
#7822=ORIENTED_EDGE('',*,*,#5469,.T.);
#7823=ORIENTED_EDGE('',*,*,#5470,.T.);
#7824=ORIENTED_EDGE('',*,*,#5471,.T.);
#7825=ORIENTED_EDGE('',*,*,#5472,.T.);
#7826=ORIENTED_EDGE('',*,*,#5464,.F.);
#7827=ORIENTED_EDGE('',*,*,#5473,.T.);
#7828=ORIENTED_EDGE('',*,*,#5474,.T.);
#7829=ORIENTED_EDGE('',*,*,#5475,.T.);
#7830=ORIENTED_EDGE('',*,*,#5471,.F.);
#7831=ORIENTED_EDGE('',*,*,#5476,.T.);
#7832=ORIENTED_EDGE('',*,*,#5477,.T.);
#7833=ORIENTED_EDGE('',*,*,#5478,.T.);
#7834=ORIENTED_EDGE('',*,*,#5474,.F.);
#7835=ORIENTED_EDGE('',*,*,#5479,.T.);
#7836=ORIENTED_EDGE('',*,*,#5480,.T.);
#7837=ORIENTED_EDGE('',*,*,#5481,.T.);
#7838=ORIENTED_EDGE('',*,*,#5477,.F.);
#7839=ORIENTED_EDGE('',*,*,#5482,.T.);
#7840=ORIENTED_EDGE('',*,*,#5483,.T.);
#7841=ORIENTED_EDGE('',*,*,#5484,.T.);
#7842=ORIENTED_EDGE('',*,*,#5480,.F.);
#7843=ORIENTED_EDGE('',*,*,#5485,.T.);
#7844=ORIENTED_EDGE('',*,*,#5486,.T.);
#7845=ORIENTED_EDGE('',*,*,#5487,.T.);
#7846=ORIENTED_EDGE('',*,*,#5483,.F.);
#7847=ORIENTED_EDGE('',*,*,#5488,.T.);
#7848=ORIENTED_EDGE('',*,*,#5489,.T.);
#7849=ORIENTED_EDGE('',*,*,#5490,.T.);
#7850=ORIENTED_EDGE('',*,*,#5486,.F.);
#7851=ORIENTED_EDGE('',*,*,#5491,.T.);
#7852=ORIENTED_EDGE('',*,*,#5492,.T.);
#7853=ORIENTED_EDGE('',*,*,#5493,.T.);
#7854=ORIENTED_EDGE('',*,*,#5489,.F.);
#7855=ORIENTED_EDGE('',*,*,#5494,.T.);
#7856=ORIENTED_EDGE('',*,*,#5495,.F.);
#7857=ORIENTED_EDGE('',*,*,#5496,.T.);
#7858=ORIENTED_EDGE('',*,*,#5497,.F.);
#7859=ORIENTED_EDGE('',*,*,#5498,.T.);
#7860=ORIENTED_EDGE('',*,*,#5499,.T.);
#7861=ORIENTED_EDGE('',*,*,#5500,.T.);
#7862=ORIENTED_EDGE('',*,*,#5501,.F.);
#7863=ORIENTED_EDGE('',*,*,#5502,.F.);
#7864=ORIENTED_EDGE('',*,*,#5503,.T.);
#7865=ORIENTED_EDGE('',*,*,#5504,.T.);
#7866=ORIENTED_EDGE('',*,*,#5499,.F.);
#7867=ORIENTED_EDGE('',*,*,#5505,.F.);
#7868=ORIENTED_EDGE('',*,*,#5506,.T.);
#7869=ORIENTED_EDGE('',*,*,#5507,.T.);
#7870=ORIENTED_EDGE('',*,*,#5503,.F.);
#7871=ORIENTED_EDGE('',*,*,#5508,.F.);
#7872=ORIENTED_EDGE('',*,*,#5509,.T.);
#7873=ORIENTED_EDGE('',*,*,#5510,.T.);
#7874=ORIENTED_EDGE('',*,*,#5506,.F.);
#7875=ORIENTED_EDGE('',*,*,#5511,.F.);
#7876=ORIENTED_EDGE('',*,*,#5512,.T.);
#7877=ORIENTED_EDGE('',*,*,#5513,.T.);
#7878=ORIENTED_EDGE('',*,*,#5509,.F.);
#7879=ORIENTED_EDGE('',*,*,#5514,.F.);
#7880=ORIENTED_EDGE('',*,*,#5515,.T.);
#7881=ORIENTED_EDGE('',*,*,#5516,.T.);
#7882=ORIENTED_EDGE('',*,*,#5512,.F.);
#7883=ORIENTED_EDGE('',*,*,#5517,.F.);
#7884=ORIENTED_EDGE('',*,*,#5518,.T.);
#7885=ORIENTED_EDGE('',*,*,#5519,.T.);
#7886=ORIENTED_EDGE('',*,*,#5515,.F.);
#7887=ORIENTED_EDGE('',*,*,#5520,.F.);
#7888=ORIENTED_EDGE('',*,*,#5521,.T.);
#7889=ORIENTED_EDGE('',*,*,#5522,.T.);
#7890=ORIENTED_EDGE('',*,*,#5518,.F.);
#7891=ORIENTED_EDGE('',*,*,#5523,.F.);
#7892=ORIENTED_EDGE('',*,*,#5524,.T.);
#7893=ORIENTED_EDGE('',*,*,#5525,.T.);
#7894=ORIENTED_EDGE('',*,*,#5521,.F.);
#7895=ORIENTED_EDGE('',*,*,#5526,.F.);
#7896=ORIENTED_EDGE('',*,*,#5527,.F.);
#7897=ORIENTED_EDGE('',*,*,#5528,.F.);
#7898=ORIENTED_EDGE('',*,*,#5529,.F.);
#7899=ORIENTED_EDGE('',*,*,#5530,.T.);
#7900=ORIENTED_EDGE('',*,*,#5466,.F.);
#7901=ORIENTED_EDGE('',*,*,#5531,.T.);
#7902=ORIENTED_EDGE('',*,*,#5501,.T.);
#7903=ORIENTED_EDGE('',*,*,#5532,.T.);
#7904=ORIENTED_EDGE('',*,*,#5469,.F.);
#7905=ORIENTED_EDGE('',*,*,#5527,.T.);
#7906=ORIENTED_EDGE('',*,*,#5533,.T.);
#7907=ORIENTED_EDGE('',*,*,#5524,.F.);
#7908=ORIENTED_EDGE('',*,*,#5534,.F.);
#7909=ORIENTED_EDGE('',*,*,#5532,.F.);
#7910=ORIENTED_EDGE('',*,*,#5500,.F.);
#7911=ORIENTED_EDGE('',*,*,#5504,.F.);
#7912=ORIENTED_EDGE('',*,*,#5507,.F.);
#7913=ORIENTED_EDGE('',*,*,#5510,.F.);
#7914=ORIENTED_EDGE('',*,*,#5513,.F.);
#7915=ORIENTED_EDGE('',*,*,#5516,.F.);
#7916=ORIENTED_EDGE('',*,*,#5519,.F.);
#7917=ORIENTED_EDGE('',*,*,#5522,.F.);
#7918=ORIENTED_EDGE('',*,*,#5525,.F.);
#7919=ORIENTED_EDGE('',*,*,#5533,.F.);
#7920=ORIENTED_EDGE('',*,*,#5530,.F.);
#7921=ORIENTED_EDGE('',*,*,#5535,.F.);
#7922=ORIENTED_EDGE('',*,*,#5496,.F.);
#7923=ORIENTED_EDGE('',*,*,#5536,.F.);
#7924=ORIENTED_EDGE('',*,*,#5494,.F.);
#7925=ORIENTED_EDGE('',*,*,#5491,.F.);
#7926=ORIENTED_EDGE('',*,*,#5488,.F.);
#7927=ORIENTED_EDGE('',*,*,#5485,.F.);
#7928=ORIENTED_EDGE('',*,*,#5482,.F.);
#7929=ORIENTED_EDGE('',*,*,#5479,.F.);
#7930=ORIENTED_EDGE('',*,*,#5476,.F.);
#7931=ORIENTED_EDGE('',*,*,#5473,.F.);
#7932=ORIENTED_EDGE('',*,*,#5470,.F.);
#7933=ORIENTED_EDGE('',*,*,#5531,.F.);
#7934=ORIENTED_EDGE('',*,*,#5465,.F.);
#7935=ORIENTED_EDGE('',*,*,#5472,.F.);
#7936=ORIENTED_EDGE('',*,*,#5475,.F.);
#7937=ORIENTED_EDGE('',*,*,#5478,.F.);
#7938=ORIENTED_EDGE('',*,*,#5481,.F.);
#7939=ORIENTED_EDGE('',*,*,#5484,.F.);
#7940=ORIENTED_EDGE('',*,*,#5487,.F.);
#7941=ORIENTED_EDGE('',*,*,#5490,.F.);
#7942=ORIENTED_EDGE('',*,*,#5493,.F.);
#7943=ORIENTED_EDGE('',*,*,#5537,.F.);
#7944=ORIENTED_EDGE('',*,*,#5498,.F.);
#7945=ORIENTED_EDGE('',*,*,#5538,.F.);
#7946=ORIENTED_EDGE('',*,*,#5528,.T.);
#7947=ORIENTED_EDGE('',*,*,#5534,.T.);
#7948=ORIENTED_EDGE('',*,*,#5526,.T.);
#7949=ORIENTED_EDGE('',*,*,#5523,.T.);
#7950=ORIENTED_EDGE('',*,*,#5520,.T.);
#7951=ORIENTED_EDGE('',*,*,#5517,.T.);
#7952=ORIENTED_EDGE('',*,*,#5514,.T.);
#7953=ORIENTED_EDGE('',*,*,#5511,.T.);
#7954=ORIENTED_EDGE('',*,*,#5508,.T.);
#7955=ORIENTED_EDGE('',*,*,#5505,.T.);
#7956=ORIENTED_EDGE('',*,*,#5502,.T.);
#7957=ORIENTED_EDGE('',*,*,#5495,.T.);
#7958=ORIENTED_EDGE('',*,*,#5537,.T.);
#7959=ORIENTED_EDGE('',*,*,#5492,.F.);
#7960=ORIENTED_EDGE('',*,*,#5536,.T.);
#7961=ORIENTED_EDGE('',*,*,#5468,.F.);
#7962=ORIENTED_EDGE('',*,*,#5539,.F.);
#7963=ORIENTED_EDGE('',*,*,#5540,.T.);
#7964=ORIENTED_EDGE('',*,*,#5541,.F.);
#7965=ORIENTED_EDGE('',*,*,#5540,.F.);
#7966=ORIENTED_EDGE('',*,*,#5542,.T.);
#7967=ORIENTED_EDGE('',*,*,#5543,.T.);
#7968=ORIENTED_EDGE('',*,*,#5544,.F.);
#7969=ORIENTED_EDGE('',*,*,#5545,.F.);
#7970=ORIENTED_EDGE('',*,*,#5546,.F.);
#7971=ORIENTED_EDGE('',*,*,#5547,.F.);
#7972=ORIENTED_EDGE('',*,*,#5542,.F.);
#7973=ORIENTED_EDGE('',*,*,#5548,.F.);
#7974=ORIENTED_EDGE('',*,*,#5541,.T.);
#7975=ORIENTED_EDGE('',*,*,#5549,.F.);
#7976=ORIENTED_EDGE('',*,*,#5543,.F.);
#7977=ORIENTED_EDGE('',*,*,#5547,.T.);
#7978=ORIENTED_EDGE('',*,*,#5550,.F.);
#7979=ORIENTED_EDGE('',*,*,#5551,.T.);
#7980=ORIENTED_EDGE('',*,*,#5552,.T.);
#7981=ORIENTED_EDGE('',*,*,#5546,.T.);
#7982=ORIENTED_EDGE('',*,*,#5553,.F.);
#7983=ORIENTED_EDGE('',*,*,#5554,.T.);
#7984=ORIENTED_EDGE('',*,*,#5550,.T.);
#7985=ORIENTED_EDGE('',*,*,#5555,.F.);
#7986=ORIENTED_EDGE('',*,*,#5556,.F.);
#7987=ORIENTED_EDGE('',*,*,#5557,.T.);
#7988=ORIENTED_EDGE('',*,*,#5553,.T.);
#7989=ORIENTED_EDGE('',*,*,#5548,.T.);
#7990=ORIENTED_EDGE('',*,*,#5545,.T.);
#7991=ORIENTED_EDGE('',*,*,#5558,.T.);
#7992=ORIENTED_EDGE('',*,*,#5556,.T.);
#7993=ORIENTED_EDGE('',*,*,#5559,.F.);
#7994=ORIENTED_EDGE('',*,*,#5552,.F.);
#7995=ORIENTED_EDGE('',*,*,#5549,.T.);
#7996=ORIENTED_EDGE('',*,*,#5559,.T.);
#7997=ORIENTED_EDGE('',*,*,#5555,.T.);
#7998=ORIENTED_EDGE('',*,*,#5544,.T.);
#7999=ORIENTED_EDGE('',*,*,#5538,.T.);
#8000=ORIENTED_EDGE('',*,*,#5497,.T.);
#8001=ORIENTED_EDGE('',*,*,#5535,.T.);
#8002=ORIENTED_EDGE('',*,*,#5529,.T.);
#8003=ORIENTED_EDGE('',*,*,#5539,.T.);
#8004=ORIENTED_EDGE('',*,*,#5558,.F.);
#8005=ORIENTED_EDGE('',*,*,#5551,.F.);
#8006=ORIENTED_EDGE('',*,*,#5554,.F.);
#8007=ORIENTED_EDGE('',*,*,#5557,.F.);
#8008=ORIENTED_EDGE('',*,*,#5560,.F.);
#8009=ORIENTED_EDGE('',*,*,#5561,.T.);
#8010=ORIENTED_EDGE('',*,*,#5562,.F.);
#8011=ORIENTED_EDGE('',*,*,#5561,.F.);
#8012=ORIENTED_EDGE('',*,*,#5563,.T.);
#8013=ORIENTED_EDGE('',*,*,#5564,.T.);
#8014=ORIENTED_EDGE('',*,*,#5565,.F.);
#8015=ORIENTED_EDGE('',*,*,#5566,.F.);
#8016=ORIENTED_EDGE('',*,*,#5567,.T.);
#8017=ORIENTED_EDGE('',*,*,#5566,.T.);
#8018=ORIENTED_EDGE('',*,*,#5568,.F.);
#8019=ORIENTED_EDGE('',*,*,#5569,.F.);
#8020=ORIENTED_EDGE('',*,*,#5570,.T.);
#8021=ORIENTED_EDGE('',*,*,#5569,.T.);
#8022=ORIENTED_EDGE('',*,*,#5571,.F.);
#8023=ORIENTED_EDGE('',*,*,#5572,.F.);
#8024=ORIENTED_EDGE('',*,*,#5573,.T.);
#8025=ORIENTED_EDGE('',*,*,#5572,.T.);
#8026=ORIENTED_EDGE('',*,*,#5574,.F.);
#8027=ORIENTED_EDGE('',*,*,#5564,.F.);
#8028=ORIENTED_EDGE('',*,*,#5574,.T.);
#8029=ORIENTED_EDGE('',*,*,#5571,.T.);
#8030=ORIENTED_EDGE('',*,*,#5568,.T.);
#8031=ORIENTED_EDGE('',*,*,#5565,.T.);
#8032=ORIENTED_EDGE('',*,*,#5560,.T.);
#8033=ORIENTED_EDGE('',*,*,#5573,.F.);
#8034=ORIENTED_EDGE('',*,*,#5563,.F.);
#8035=ORIENTED_EDGE('',*,*,#5567,.F.);
#8036=ORIENTED_EDGE('',*,*,#5570,.F.);
#8037=ORIENTED_EDGE('',*,*,#5562,.T.);
#8038=ORIENTED_EDGE('',*,*,#5575,.F.);
#8039=ORIENTED_EDGE('',*,*,#5576,.T.);
#8040=ORIENTED_EDGE('',*,*,#5577,.T.);
#8041=ORIENTED_EDGE('',*,*,#5576,.F.);
#8042=ORIENTED_EDGE('',*,*,#5578,.F.);
#8043=ORIENTED_EDGE('',*,*,#5579,.T.);
#8044=ORIENTED_EDGE('',*,*,#5580,.T.);
#8045=ORIENTED_EDGE('',*,*,#5579,.F.);
#8046=ORIENTED_EDGE('',*,*,#5578,.T.);
#8047=ORIENTED_EDGE('',*,*,#5575,.T.);
#8048=ORIENTED_EDGE('',*,*,#5580,.F.);
#8049=ORIENTED_EDGE('',*,*,#5577,.F.);
#8050=ORIENTED_EDGE('',*,*,#5581,.T.);
#8051=ORIENTED_EDGE('',*,*,#5582,.T.);
#8052=ORIENTED_EDGE('',*,*,#5583,.F.);
#8053=ORIENTED_EDGE('',*,*,#5582,.F.);
#8054=ORIENTED_EDGE('',*,*,#5584,.F.);
#8055=ORIENTED_EDGE('',*,*,#5581,.F.);
#8056=ORIENTED_EDGE('',*,*,#5585,.F.);
#8057=ORIENTED_EDGE('',*,*,#5583,.T.);
#8058=ORIENTED_EDGE('',*,*,#5586,.F.);
#8059=ORIENTED_EDGE('',*,*,#5587,.T.);
#8060=ORIENTED_EDGE('',*,*,#5585,.T.);
#8061=ORIENTED_EDGE('',*,*,#5587,.F.);
#8062=ORIENTED_EDGE('',*,*,#5588,.T.);
#8063=ORIENTED_EDGE('',*,*,#5589,.F.);
#8064=ORIENTED_EDGE('',*,*,#5588,.F.);
#8065=ORIENTED_EDGE('',*,*,#5590,.T.);
#8066=ORIENTED_EDGE('',*,*,#5591,.T.);
#8067=ORIENTED_EDGE('',*,*,#5590,.F.);
#8068=ORIENTED_EDGE('',*,*,#5591,.F.);
#8069=ORIENTED_EDGE('',*,*,#5584,.T.);
#8070=ORIENTED_EDGE('',*,*,#5592,.T.);
#8071=ORIENTED_EDGE('',*,*,#5589,.T.);
#8072=ORIENTED_EDGE('',*,*,#5592,.F.);
#8073=ORIENTED_EDGE('',*,*,#5586,.T.);
#8074=ORIENTED_EDGE('',*,*,#5593,.F.);
#8075=ORIENTED_EDGE('',*,*,#5594,.F.);
#8076=ORIENTED_EDGE('',*,*,#5595,.F.);
#8077=ORIENTED_EDGE('',*,*,#5596,.F.);
#8078=ORIENTED_EDGE('',*,*,#5597,.F.);
#8079=ORIENTED_EDGE('',*,*,#5598,.F.);
#8080=ORIENTED_EDGE('',*,*,#5599,.F.);
#8081=ORIENTED_EDGE('',*,*,#5600,.F.);
#8082=ORIENTED_EDGE('',*,*,#5600,.T.);
#8083=ORIENTED_EDGE('',*,*,#5601,.F.);
#8084=ORIENTED_EDGE('',*,*,#5594,.T.);
#8085=ORIENTED_EDGE('',*,*,#5602,.F.);
#8086=ORIENTED_EDGE('',*,*,#5597,.T.);
#8087=ORIENTED_EDGE('',*,*,#5602,.T.);
#8088=ORIENTED_EDGE('',*,*,#5593,.T.);
#8089=ORIENTED_EDGE('',*,*,#5603,.F.);
#8090=ORIENTED_EDGE('',*,*,#5599,.T.);
#8091=ORIENTED_EDGE('',*,*,#5604,.F.);
#8092=ORIENTED_EDGE('',*,*,#5595,.T.);
#8093=ORIENTED_EDGE('',*,*,#5601,.T.);
#8094=ORIENTED_EDGE('',*,*,#5598,.T.);
#8095=ORIENTED_EDGE('',*,*,#5603,.T.);
#8096=ORIENTED_EDGE('',*,*,#5596,.T.);
#8097=ORIENTED_EDGE('',*,*,#5604,.T.);
#8098=ORIENTED_EDGE('',*,*,#5605,.T.);
#8099=ORIENTED_EDGE('',*,*,#5606,.T.);
#8100=ORIENTED_EDGE('',*,*,#5607,.F.);
#8101=ORIENTED_EDGE('',*,*,#5606,.F.);
#8102=ORIENTED_EDGE('',*,*,#5607,.T.);
#8103=ORIENTED_EDGE('',*,*,#5605,.F.);
#8104=ORIENTED_EDGE('',*,*,#5608,.F.);
#8105=ORIENTED_EDGE('',*,*,#5609,.T.);
#8106=ORIENTED_EDGE('',*,*,#5610,.T.);
#8107=ORIENTED_EDGE('',*,*,#5609,.F.);
#8108=ORIENTED_EDGE('',*,*,#5611,.F.);
#8109=ORIENTED_EDGE('',*,*,#5612,.T.);
#8110=ORIENTED_EDGE('',*,*,#5613,.T.);
#8111=ORIENTED_EDGE('',*,*,#5612,.F.);
#8112=ORIENTED_EDGE('',*,*,#5611,.T.);
#8113=ORIENTED_EDGE('',*,*,#5608,.T.);
#8114=ORIENTED_EDGE('',*,*,#5613,.F.);
#8115=ORIENTED_EDGE('',*,*,#5610,.F.);
#8116=ORIENTED_EDGE('',*,*,#5614,.F.);
#8117=ORIENTED_EDGE('',*,*,#5615,.T.);
#8118=ORIENTED_EDGE('',*,*,#5616,.T.);
#8119=ORIENTED_EDGE('',*,*,#5617,.T.);
#8120=ORIENTED_EDGE('',*,*,#5618,.F.);
#8121=ORIENTED_EDGE('',*,*,#5619,.T.);
#8122=ORIENTED_EDGE('',*,*,#5614,.T.);
#8123=ORIENTED_EDGE('',*,*,#5620,.T.);
#8124=ORIENTED_EDGE('',*,*,#5621,.F.);
#8125=ORIENTED_EDGE('',*,*,#5622,.T.);
#8126=ORIENTED_EDGE('',*,*,#5618,.T.);
#8127=ORIENTED_EDGE('',*,*,#5623,.T.);
#8128=ORIENTED_EDGE('',*,*,#5624,.F.);
#8129=ORIENTED_EDGE('',*,*,#5625,.T.);
#8130=ORIENTED_EDGE('',*,*,#5621,.T.);
#8131=ORIENTED_EDGE('',*,*,#5626,.T.);
#8132=ORIENTED_EDGE('',*,*,#5627,.F.);
#8133=ORIENTED_EDGE('',*,*,#5628,.T.);
#8134=ORIENTED_EDGE('',*,*,#5624,.T.);
#8135=ORIENTED_EDGE('',*,*,#5629,.T.);
#8136=ORIENTED_EDGE('',*,*,#5630,.F.);
#8137=ORIENTED_EDGE('',*,*,#5631,.T.);
#8138=ORIENTED_EDGE('',*,*,#5627,.T.);
#8139=ORIENTED_EDGE('',*,*,#5632,.T.);
#8140=ORIENTED_EDGE('',*,*,#5633,.F.);
#8141=ORIENTED_EDGE('',*,*,#5634,.T.);
#8142=ORIENTED_EDGE('',*,*,#5630,.T.);
#8143=ORIENTED_EDGE('',*,*,#5635,.T.);
#8144=ORIENTED_EDGE('',*,*,#5636,.F.);
#8145=ORIENTED_EDGE('',*,*,#5637,.T.);
#8146=ORIENTED_EDGE('',*,*,#5633,.T.);
#8147=ORIENTED_EDGE('',*,*,#5638,.T.);
#8148=ORIENTED_EDGE('',*,*,#5639,.F.);
#8149=ORIENTED_EDGE('',*,*,#5640,.T.);
#8150=ORIENTED_EDGE('',*,*,#5636,.T.);
#8151=ORIENTED_EDGE('',*,*,#5641,.T.);
#8152=ORIENTED_EDGE('',*,*,#5642,.F.);
#8153=ORIENTED_EDGE('',*,*,#5643,.T.);
#8154=ORIENTED_EDGE('',*,*,#5639,.T.);
#8155=ORIENTED_EDGE('',*,*,#5644,.T.);
#8156=ORIENTED_EDGE('',*,*,#5645,.F.);
#8157=ORIENTED_EDGE('',*,*,#5646,.T.);
#8158=ORIENTED_EDGE('',*,*,#5642,.T.);
#8159=ORIENTED_EDGE('',*,*,#5647,.T.);
#8160=ORIENTED_EDGE('',*,*,#5648,.F.);
#8161=ORIENTED_EDGE('',*,*,#5649,.T.);
#8162=ORIENTED_EDGE('',*,*,#5645,.T.);
#8163=ORIENTED_EDGE('',*,*,#5650,.T.);
#8164=ORIENTED_EDGE('',*,*,#5651,.F.);
#8165=ORIENTED_EDGE('',*,*,#5652,.T.);
#8166=ORIENTED_EDGE('',*,*,#5648,.T.);
#8167=ORIENTED_EDGE('',*,*,#5653,.T.);
#8168=ORIENTED_EDGE('',*,*,#5654,.F.);
#8169=ORIENTED_EDGE('',*,*,#5655,.T.);
#8170=ORIENTED_EDGE('',*,*,#5651,.T.);
#8171=ORIENTED_EDGE('',*,*,#5656,.T.);
#8172=ORIENTED_EDGE('',*,*,#5657,.F.);
#8173=ORIENTED_EDGE('',*,*,#5658,.T.);
#8174=ORIENTED_EDGE('',*,*,#5654,.T.);
#8175=ORIENTED_EDGE('',*,*,#5659,.T.);
#8176=ORIENTED_EDGE('',*,*,#5660,.F.);
#8177=ORIENTED_EDGE('',*,*,#5661,.T.);
#8178=ORIENTED_EDGE('',*,*,#5657,.T.);
#8179=ORIENTED_EDGE('',*,*,#5662,.T.);
#8180=ORIENTED_EDGE('',*,*,#5663,.F.);
#8181=ORIENTED_EDGE('',*,*,#5664,.T.);
#8182=ORIENTED_EDGE('',*,*,#5665,.T.);
#8183=ORIENTED_EDGE('',*,*,#5666,.F.);
#8184=ORIENTED_EDGE('',*,*,#5667,.F.);
#8185=ORIENTED_EDGE('',*,*,#5668,.T.);
#8186=ORIENTED_EDGE('',*,*,#5663,.T.);
#8187=ORIENTED_EDGE('',*,*,#5669,.F.);
#8188=ORIENTED_EDGE('',*,*,#5670,.F.);
#8189=ORIENTED_EDGE('',*,*,#5671,.T.);
#8190=ORIENTED_EDGE('',*,*,#5667,.T.);
#8191=ORIENTED_EDGE('',*,*,#5672,.F.);
#8192=ORIENTED_EDGE('',*,*,#5673,.F.);
#8193=ORIENTED_EDGE('',*,*,#5674,.T.);
#8194=ORIENTED_EDGE('',*,*,#5670,.T.);
#8195=ORIENTED_EDGE('',*,*,#5675,.F.);
#8196=ORIENTED_EDGE('',*,*,#5676,.F.);
#8197=ORIENTED_EDGE('',*,*,#5677,.T.);
#8198=ORIENTED_EDGE('',*,*,#5673,.T.);
#8199=ORIENTED_EDGE('',*,*,#5678,.F.);
#8200=ORIENTED_EDGE('',*,*,#5679,.F.);
#8201=ORIENTED_EDGE('',*,*,#5680,.T.);
#8202=ORIENTED_EDGE('',*,*,#5676,.T.);
#8203=ORIENTED_EDGE('',*,*,#5681,.F.);
#8204=ORIENTED_EDGE('',*,*,#5682,.F.);
#8205=ORIENTED_EDGE('',*,*,#5683,.T.);
#8206=ORIENTED_EDGE('',*,*,#5679,.T.);
#8207=ORIENTED_EDGE('',*,*,#5684,.F.);
#8208=ORIENTED_EDGE('',*,*,#5685,.F.);
#8209=ORIENTED_EDGE('',*,*,#5686,.T.);
#8210=ORIENTED_EDGE('',*,*,#5682,.T.);
#8211=ORIENTED_EDGE('',*,*,#5687,.F.);
#8212=ORIENTED_EDGE('',*,*,#5688,.F.);
#8213=ORIENTED_EDGE('',*,*,#5689,.T.);
#8214=ORIENTED_EDGE('',*,*,#5685,.T.);
#8215=ORIENTED_EDGE('',*,*,#5690,.F.);
#8216=ORIENTED_EDGE('',*,*,#5691,.F.);
#8217=ORIENTED_EDGE('',*,*,#5692,.T.);
#8218=ORIENTED_EDGE('',*,*,#5688,.T.);
#8219=ORIENTED_EDGE('',*,*,#5693,.F.);
#8220=ORIENTED_EDGE('',*,*,#5694,.F.);
#8221=ORIENTED_EDGE('',*,*,#5695,.T.);
#8222=ORIENTED_EDGE('',*,*,#5691,.T.);
#8223=ORIENTED_EDGE('',*,*,#5696,.F.);
#8224=ORIENTED_EDGE('',*,*,#5697,.F.);
#8225=ORIENTED_EDGE('',*,*,#5698,.T.);
#8226=ORIENTED_EDGE('',*,*,#5694,.T.);
#8227=ORIENTED_EDGE('',*,*,#5699,.F.);
#8228=ORIENTED_EDGE('',*,*,#5700,.F.);
#8229=ORIENTED_EDGE('',*,*,#5701,.T.);
#8230=ORIENTED_EDGE('',*,*,#5697,.T.);
#8231=ORIENTED_EDGE('',*,*,#5702,.F.);
#8232=ORIENTED_EDGE('',*,*,#5703,.F.);
#8233=ORIENTED_EDGE('',*,*,#5704,.T.);
#8234=ORIENTED_EDGE('',*,*,#5700,.T.);
#8235=ORIENTED_EDGE('',*,*,#5705,.F.);
#8236=ORIENTED_EDGE('',*,*,#5706,.F.);
#8237=ORIENTED_EDGE('',*,*,#5707,.T.);
#8238=ORIENTED_EDGE('',*,*,#5703,.T.);
#8239=ORIENTED_EDGE('',*,*,#5708,.F.);
#8240=ORIENTED_EDGE('',*,*,#5709,.F.);
#8241=ORIENTED_EDGE('',*,*,#5710,.T.);
#8242=ORIENTED_EDGE('',*,*,#5706,.T.);
#8243=ORIENTED_EDGE('',*,*,#5711,.F.);
#8244=ORIENTED_EDGE('',*,*,#5712,.F.);
#8245=ORIENTED_EDGE('',*,*,#5665,.F.);
#8246=ORIENTED_EDGE('',*,*,#5713,.F.);
#8247=ORIENTED_EDGE('',*,*,#5714,.F.);
#8248=ORIENTED_EDGE('',*,*,#5715,.F.);
#8249=ORIENTED_EDGE('',*,*,#5716,.T.);
#8250=ORIENTED_EDGE('',*,*,#5717,.F.);
#8251=ORIENTED_EDGE('',*,*,#5716,.F.);
#8252=ORIENTED_EDGE('',*,*,#5713,.T.);
#8253=ORIENTED_EDGE('',*,*,#5664,.F.);
#8254=ORIENTED_EDGE('',*,*,#5668,.F.);
#8255=ORIENTED_EDGE('',*,*,#5671,.F.);
#8256=ORIENTED_EDGE('',*,*,#5674,.F.);
#8257=ORIENTED_EDGE('',*,*,#5677,.F.);
#8258=ORIENTED_EDGE('',*,*,#5680,.F.);
#8259=ORIENTED_EDGE('',*,*,#5683,.F.);
#8260=ORIENTED_EDGE('',*,*,#5686,.F.);
#8261=ORIENTED_EDGE('',*,*,#5689,.F.);
#8262=ORIENTED_EDGE('',*,*,#5692,.F.);
#8263=ORIENTED_EDGE('',*,*,#5695,.F.);
#8264=ORIENTED_EDGE('',*,*,#5698,.F.);
#8265=ORIENTED_EDGE('',*,*,#5701,.F.);
#8266=ORIENTED_EDGE('',*,*,#5704,.F.);
#8267=ORIENTED_EDGE('',*,*,#5707,.F.);
#8268=ORIENTED_EDGE('',*,*,#5710,.F.);
#8269=ORIENTED_EDGE('',*,*,#5718,.F.);
#8270=ORIENTED_EDGE('',*,*,#5719,.F.);
#8271=ORIENTED_EDGE('',*,*,#5615,.F.);
#8272=ORIENTED_EDGE('',*,*,#5619,.F.);
#8273=ORIENTED_EDGE('',*,*,#5622,.F.);
#8274=ORIENTED_EDGE('',*,*,#5625,.F.);
#8275=ORIENTED_EDGE('',*,*,#5628,.F.);
#8276=ORIENTED_EDGE('',*,*,#5631,.F.);
#8277=ORIENTED_EDGE('',*,*,#5634,.F.);
#8278=ORIENTED_EDGE('',*,*,#5637,.F.);
#8279=ORIENTED_EDGE('',*,*,#5640,.F.);
#8280=ORIENTED_EDGE('',*,*,#5643,.F.);
#8281=ORIENTED_EDGE('',*,*,#5646,.F.);
#8282=ORIENTED_EDGE('',*,*,#5649,.F.);
#8283=ORIENTED_EDGE('',*,*,#5652,.F.);
#8284=ORIENTED_EDGE('',*,*,#5655,.F.);
#8285=ORIENTED_EDGE('',*,*,#5658,.F.);
#8286=ORIENTED_EDGE('',*,*,#5661,.F.);
#8287=ORIENTED_EDGE('',*,*,#5720,.F.);
#8288=ORIENTED_EDGE('',*,*,#5709,.T.);
#8289=ORIENTED_EDGE('',*,*,#5721,.F.);
#8290=ORIENTED_EDGE('',*,*,#5722,.F.);
#8291=ORIENTED_EDGE('',*,*,#5718,.T.);
#8292=ORIENTED_EDGE('',*,*,#5712,.T.);
#8293=ORIENTED_EDGE('',*,*,#5715,.T.);
#8294=ORIENTED_EDGE('',*,*,#5723,.F.);
#8295=ORIENTED_EDGE('',*,*,#5662,.F.);
#8296=ORIENTED_EDGE('',*,*,#5659,.F.);
#8297=ORIENTED_EDGE('',*,*,#5656,.F.);
#8298=ORIENTED_EDGE('',*,*,#5653,.F.);
#8299=ORIENTED_EDGE('',*,*,#5650,.F.);
#8300=ORIENTED_EDGE('',*,*,#5647,.F.);
#8301=ORIENTED_EDGE('',*,*,#5644,.F.);
#8302=ORIENTED_EDGE('',*,*,#5641,.F.);
#8303=ORIENTED_EDGE('',*,*,#5638,.F.);
#8304=ORIENTED_EDGE('',*,*,#5635,.F.);
#8305=ORIENTED_EDGE('',*,*,#5632,.F.);
#8306=ORIENTED_EDGE('',*,*,#5629,.F.);
#8307=ORIENTED_EDGE('',*,*,#5626,.F.);
#8308=ORIENTED_EDGE('',*,*,#5623,.F.);
#8309=ORIENTED_EDGE('',*,*,#5620,.F.);
#8310=ORIENTED_EDGE('',*,*,#5617,.F.);
#8311=ORIENTED_EDGE('',*,*,#5724,.F.);
#8312=ORIENTED_EDGE('',*,*,#5721,.T.);
#8313=ORIENTED_EDGE('',*,*,#5711,.T.);
#8314=ORIENTED_EDGE('',*,*,#5708,.T.);
#8315=ORIENTED_EDGE('',*,*,#5705,.T.);
#8316=ORIENTED_EDGE('',*,*,#5702,.T.);
#8317=ORIENTED_EDGE('',*,*,#5699,.T.);
#8318=ORIENTED_EDGE('',*,*,#5696,.T.);
#8319=ORIENTED_EDGE('',*,*,#5693,.T.);
#8320=ORIENTED_EDGE('',*,*,#5690,.T.);
#8321=ORIENTED_EDGE('',*,*,#5687,.T.);
#8322=ORIENTED_EDGE('',*,*,#5684,.T.);
#8323=ORIENTED_EDGE('',*,*,#5681,.T.);
#8324=ORIENTED_EDGE('',*,*,#5678,.T.);
#8325=ORIENTED_EDGE('',*,*,#5675,.T.);
#8326=ORIENTED_EDGE('',*,*,#5672,.T.);
#8327=ORIENTED_EDGE('',*,*,#5669,.T.);
#8328=ORIENTED_EDGE('',*,*,#5666,.T.);
#8329=ORIENTED_EDGE('',*,*,#5660,.T.);
#8330=ORIENTED_EDGE('',*,*,#5723,.T.);
#8331=ORIENTED_EDGE('',*,*,#5714,.T.);
#8332=ORIENTED_EDGE('',*,*,#5720,.T.);
#8333=ORIENTED_EDGE('',*,*,#5725,.F.);
#8334=ORIENTED_EDGE('',*,*,#5726,.T.);
#8335=ORIENTED_EDGE('',*,*,#5727,.T.);
#8336=ORIENTED_EDGE('',*,*,#5728,.F.);
#8337=ORIENTED_EDGE('',*,*,#5729,.F.);
#8338=ORIENTED_EDGE('',*,*,#5730,.T.);
#8339=ORIENTED_EDGE('',*,*,#5731,.T.);
#8340=ORIENTED_EDGE('',*,*,#5726,.F.);
#8341=ORIENTED_EDGE('',*,*,#5732,.F.);
#8342=ORIENTED_EDGE('',*,*,#5733,.T.);
#8343=ORIENTED_EDGE('',*,*,#5734,.T.);
#8344=ORIENTED_EDGE('',*,*,#5730,.F.);
#8345=ORIENTED_EDGE('',*,*,#5735,.F.);
#8346=ORIENTED_EDGE('',*,*,#5736,.T.);
#8347=ORIENTED_EDGE('',*,*,#5737,.T.);
#8348=ORIENTED_EDGE('',*,*,#5733,.F.);
#8349=ORIENTED_EDGE('',*,*,#5738,.F.);
#8350=ORIENTED_EDGE('',*,*,#5739,.T.);
#8351=ORIENTED_EDGE('',*,*,#5740,.T.);
#8352=ORIENTED_EDGE('',*,*,#5736,.F.);
#8353=ORIENTED_EDGE('',*,*,#5741,.F.);
#8354=ORIENTED_EDGE('',*,*,#5728,.T.);
#8355=ORIENTED_EDGE('',*,*,#5742,.T.);
#8356=ORIENTED_EDGE('',*,*,#5739,.F.);
#8357=ORIENTED_EDGE('',*,*,#5742,.F.);
#8358=ORIENTED_EDGE('',*,*,#5727,.F.);
#8359=ORIENTED_EDGE('',*,*,#5731,.F.);
#8360=ORIENTED_EDGE('',*,*,#5734,.F.);
#8361=ORIENTED_EDGE('',*,*,#5737,.F.);
#8362=ORIENTED_EDGE('',*,*,#5740,.F.);
#8363=ORIENTED_EDGE('',*,*,#5743,.T.);
#8364=ORIENTED_EDGE('',*,*,#5719,.T.);
#8365=ORIENTED_EDGE('',*,*,#5722,.T.);
#8366=ORIENTED_EDGE('',*,*,#5724,.T.);
#8367=ORIENTED_EDGE('',*,*,#5616,.F.);
#8368=ORIENTED_EDGE('',*,*,#5743,.F.);
#8369=ORIENTED_EDGE('',*,*,#5744,.T.);
#8370=ORIENTED_EDGE('',*,*,#5745,.T.);
#8371=ORIENTED_EDGE('',*,*,#5744,.F.);
#8372=ORIENTED_EDGE('',*,*,#5745,.F.);
#8373=ORIENTED_EDGE('',*,*,#5725,.T.);
#8374=ORIENTED_EDGE('',*,*,#5741,.T.);
#8375=ORIENTED_EDGE('',*,*,#5738,.T.);
#8376=ORIENTED_EDGE('',*,*,#5735,.T.);
#8377=ORIENTED_EDGE('',*,*,#5732,.T.);
#8378=ORIENTED_EDGE('',*,*,#5729,.T.);
#8379=ORIENTED_EDGE('',*,*,#5717,.T.);
#8380=ORIENTED_EDGE('',*,*,#5746,.F.);
#8381=ORIENTED_EDGE('',*,*,#5747,.T.);
#8382=ORIENTED_EDGE('',*,*,#5748,.T.);
#8383=ORIENTED_EDGE('',*,*,#5749,.T.);
#8384=ORIENTED_EDGE('',*,*,#5750,.F.);
#8385=ORIENTED_EDGE('',*,*,#5751,.T.);
#8386=ORIENTED_EDGE('',*,*,#5746,.T.);
#8387=ORIENTED_EDGE('',*,*,#5752,.T.);
#8388=ORIENTED_EDGE('',*,*,#5753,.F.);
#8389=ORIENTED_EDGE('',*,*,#5754,.T.);
#8390=ORIENTED_EDGE('',*,*,#5750,.T.);
#8391=ORIENTED_EDGE('',*,*,#5755,.T.);
#8392=ORIENTED_EDGE('',*,*,#5756,.F.);
#8393=ORIENTED_EDGE('',*,*,#5757,.T.);
#8394=ORIENTED_EDGE('',*,*,#5753,.T.);
#8395=ORIENTED_EDGE('',*,*,#5758,.T.);
#8396=ORIENTED_EDGE('',*,*,#5759,.F.);
#8397=ORIENTED_EDGE('',*,*,#5760,.T.);
#8398=ORIENTED_EDGE('',*,*,#5756,.T.);
#8399=ORIENTED_EDGE('',*,*,#5761,.T.);
#8400=ORIENTED_EDGE('',*,*,#5762,.F.);
#8401=ORIENTED_EDGE('',*,*,#5763,.T.);
#8402=ORIENTED_EDGE('',*,*,#5759,.T.);
#8403=ORIENTED_EDGE('',*,*,#5764,.T.);
#8404=ORIENTED_EDGE('',*,*,#5765,.F.);
#8405=ORIENTED_EDGE('',*,*,#5766,.T.);
#8406=ORIENTED_EDGE('',*,*,#5762,.T.);
#8407=ORIENTED_EDGE('',*,*,#5767,.T.);
#8408=ORIENTED_EDGE('',*,*,#5768,.F.);
#8409=ORIENTED_EDGE('',*,*,#5769,.T.);
#8410=ORIENTED_EDGE('',*,*,#5765,.T.);
#8411=ORIENTED_EDGE('',*,*,#5770,.T.);
#8412=ORIENTED_EDGE('',*,*,#5771,.F.);
#8413=ORIENTED_EDGE('',*,*,#5772,.T.);
#8414=ORIENTED_EDGE('',*,*,#5768,.T.);
#8415=ORIENTED_EDGE('',*,*,#5773,.T.);
#8416=ORIENTED_EDGE('',*,*,#5774,.F.);
#8417=ORIENTED_EDGE('',*,*,#5775,.T.);
#8418=ORIENTED_EDGE('',*,*,#5771,.T.);
#8419=ORIENTED_EDGE('',*,*,#5776,.T.);
#8420=ORIENTED_EDGE('',*,*,#5777,.F.);
#8421=ORIENTED_EDGE('',*,*,#5778,.T.);
#8422=ORIENTED_EDGE('',*,*,#5779,.T.);
#8423=ORIENTED_EDGE('',*,*,#5780,.F.);
#8424=ORIENTED_EDGE('',*,*,#5781,.F.);
#8425=ORIENTED_EDGE('',*,*,#5782,.T.);
#8426=ORIENTED_EDGE('',*,*,#5777,.T.);
#8427=ORIENTED_EDGE('',*,*,#5783,.F.);
#8428=ORIENTED_EDGE('',*,*,#5784,.F.);
#8429=ORIENTED_EDGE('',*,*,#5785,.T.);
#8430=ORIENTED_EDGE('',*,*,#5781,.T.);
#8431=ORIENTED_EDGE('',*,*,#5786,.F.);
#8432=ORIENTED_EDGE('',*,*,#5787,.F.);
#8433=ORIENTED_EDGE('',*,*,#5788,.T.);
#8434=ORIENTED_EDGE('',*,*,#5784,.T.);
#8435=ORIENTED_EDGE('',*,*,#5789,.F.);
#8436=ORIENTED_EDGE('',*,*,#5790,.F.);
#8437=ORIENTED_EDGE('',*,*,#5791,.T.);
#8438=ORIENTED_EDGE('',*,*,#5787,.T.);
#8439=ORIENTED_EDGE('',*,*,#5792,.F.);
#8440=ORIENTED_EDGE('',*,*,#5793,.F.);
#8441=ORIENTED_EDGE('',*,*,#5794,.T.);
#8442=ORIENTED_EDGE('',*,*,#5790,.T.);
#8443=ORIENTED_EDGE('',*,*,#5795,.F.);
#8444=ORIENTED_EDGE('',*,*,#5796,.F.);
#8445=ORIENTED_EDGE('',*,*,#5797,.T.);
#8446=ORIENTED_EDGE('',*,*,#5793,.T.);
#8447=ORIENTED_EDGE('',*,*,#5798,.F.);
#8448=ORIENTED_EDGE('',*,*,#5799,.F.);
#8449=ORIENTED_EDGE('',*,*,#5800,.T.);
#8450=ORIENTED_EDGE('',*,*,#5796,.T.);
#8451=ORIENTED_EDGE('',*,*,#5801,.F.);
#8452=ORIENTED_EDGE('',*,*,#5802,.F.);
#8453=ORIENTED_EDGE('',*,*,#5803,.T.);
#8454=ORIENTED_EDGE('',*,*,#5799,.T.);
#8455=ORIENTED_EDGE('',*,*,#5804,.F.);
#8456=ORIENTED_EDGE('',*,*,#5805,.F.);
#8457=ORIENTED_EDGE('',*,*,#5806,.T.);
#8458=ORIENTED_EDGE('',*,*,#5802,.T.);
#8459=ORIENTED_EDGE('',*,*,#5807,.F.);
#8460=ORIENTED_EDGE('',*,*,#5808,.F.);
#8461=ORIENTED_EDGE('',*,*,#5779,.F.);
#8462=ORIENTED_EDGE('',*,*,#5809,.F.);
#8463=ORIENTED_EDGE('',*,*,#5810,.F.);
#8464=ORIENTED_EDGE('',*,*,#5811,.F.);
#8465=ORIENTED_EDGE('',*,*,#5812,.T.);
#8466=ORIENTED_EDGE('',*,*,#5813,.F.);
#8467=ORIENTED_EDGE('',*,*,#5812,.F.);
#8468=ORIENTED_EDGE('',*,*,#5809,.T.);
#8469=ORIENTED_EDGE('',*,*,#5778,.F.);
#8470=ORIENTED_EDGE('',*,*,#5782,.F.);
#8471=ORIENTED_EDGE('',*,*,#5785,.F.);
#8472=ORIENTED_EDGE('',*,*,#5788,.F.);
#8473=ORIENTED_EDGE('',*,*,#5791,.F.);
#8474=ORIENTED_EDGE('',*,*,#5794,.F.);
#8475=ORIENTED_EDGE('',*,*,#5797,.F.);
#8476=ORIENTED_EDGE('',*,*,#5800,.F.);
#8477=ORIENTED_EDGE('',*,*,#5803,.F.);
#8478=ORIENTED_EDGE('',*,*,#5806,.F.);
#8479=ORIENTED_EDGE('',*,*,#5814,.F.);
#8480=ORIENTED_EDGE('',*,*,#5815,.F.);
#8481=ORIENTED_EDGE('',*,*,#5747,.F.);
#8482=ORIENTED_EDGE('',*,*,#5751,.F.);
#8483=ORIENTED_EDGE('',*,*,#5754,.F.);
#8484=ORIENTED_EDGE('',*,*,#5757,.F.);
#8485=ORIENTED_EDGE('',*,*,#5760,.F.);
#8486=ORIENTED_EDGE('',*,*,#5763,.F.);
#8487=ORIENTED_EDGE('',*,*,#5766,.F.);
#8488=ORIENTED_EDGE('',*,*,#5769,.F.);
#8489=ORIENTED_EDGE('',*,*,#5772,.F.);
#8490=ORIENTED_EDGE('',*,*,#5775,.F.);
#8491=ORIENTED_EDGE('',*,*,#5816,.F.);
#8492=ORIENTED_EDGE('',*,*,#5805,.T.);
#8493=ORIENTED_EDGE('',*,*,#5817,.F.);
#8494=ORIENTED_EDGE('',*,*,#5818,.F.);
#8495=ORIENTED_EDGE('',*,*,#5814,.T.);
#8496=ORIENTED_EDGE('',*,*,#5808,.T.);
#8497=ORIENTED_EDGE('',*,*,#5811,.T.);
#8498=ORIENTED_EDGE('',*,*,#5819,.F.);
#8499=ORIENTED_EDGE('',*,*,#5776,.F.);
#8500=ORIENTED_EDGE('',*,*,#5773,.F.);
#8501=ORIENTED_EDGE('',*,*,#5770,.F.);
#8502=ORIENTED_EDGE('',*,*,#5767,.F.);
#8503=ORIENTED_EDGE('',*,*,#5764,.F.);
#8504=ORIENTED_EDGE('',*,*,#5761,.F.);
#8505=ORIENTED_EDGE('',*,*,#5758,.F.);
#8506=ORIENTED_EDGE('',*,*,#5755,.F.);
#8507=ORIENTED_EDGE('',*,*,#5752,.F.);
#8508=ORIENTED_EDGE('',*,*,#5749,.F.);
#8509=ORIENTED_EDGE('',*,*,#5820,.F.);
#8510=ORIENTED_EDGE('',*,*,#5817,.T.);
#8511=ORIENTED_EDGE('',*,*,#5807,.T.);
#8512=ORIENTED_EDGE('',*,*,#5804,.T.);
#8513=ORIENTED_EDGE('',*,*,#5801,.T.);
#8514=ORIENTED_EDGE('',*,*,#5798,.T.);
#8515=ORIENTED_EDGE('',*,*,#5795,.T.);
#8516=ORIENTED_EDGE('',*,*,#5792,.T.);
#8517=ORIENTED_EDGE('',*,*,#5789,.T.);
#8518=ORIENTED_EDGE('',*,*,#5786,.T.);
#8519=ORIENTED_EDGE('',*,*,#5783,.T.);
#8520=ORIENTED_EDGE('',*,*,#5780,.T.);
#8521=ORIENTED_EDGE('',*,*,#5774,.T.);
#8522=ORIENTED_EDGE('',*,*,#5819,.T.);
#8523=ORIENTED_EDGE('',*,*,#5810,.T.);
#8524=ORIENTED_EDGE('',*,*,#5816,.T.);
#8525=ORIENTED_EDGE('',*,*,#5821,.F.);
#8526=ORIENTED_EDGE('',*,*,#5822,.T.);
#8527=ORIENTED_EDGE('',*,*,#5823,.T.);
#8528=ORIENTED_EDGE('',*,*,#5824,.F.);
#8529=ORIENTED_EDGE('',*,*,#5825,.F.);
#8530=ORIENTED_EDGE('',*,*,#5826,.T.);
#8531=ORIENTED_EDGE('',*,*,#5827,.T.);
#8532=ORIENTED_EDGE('',*,*,#5822,.F.);
#8533=ORIENTED_EDGE('',*,*,#5828,.F.);
#8534=ORIENTED_EDGE('',*,*,#5829,.T.);
#8535=ORIENTED_EDGE('',*,*,#5830,.T.);
#8536=ORIENTED_EDGE('',*,*,#5826,.F.);
#8537=ORIENTED_EDGE('',*,*,#5831,.F.);
#8538=ORIENTED_EDGE('',*,*,#5832,.T.);
#8539=ORIENTED_EDGE('',*,*,#5833,.T.);
#8540=ORIENTED_EDGE('',*,*,#5829,.F.);
#8541=ORIENTED_EDGE('',*,*,#5834,.F.);
#8542=ORIENTED_EDGE('',*,*,#5835,.T.);
#8543=ORIENTED_EDGE('',*,*,#5836,.T.);
#8544=ORIENTED_EDGE('',*,*,#5832,.F.);
#8545=ORIENTED_EDGE('',*,*,#5837,.F.);
#8546=ORIENTED_EDGE('',*,*,#5824,.T.);
#8547=ORIENTED_EDGE('',*,*,#5838,.T.);
#8548=ORIENTED_EDGE('',*,*,#5835,.F.);
#8549=ORIENTED_EDGE('',*,*,#5838,.F.);
#8550=ORIENTED_EDGE('',*,*,#5823,.F.);
#8551=ORIENTED_EDGE('',*,*,#5827,.F.);
#8552=ORIENTED_EDGE('',*,*,#5830,.F.);
#8553=ORIENTED_EDGE('',*,*,#5833,.F.);
#8554=ORIENTED_EDGE('',*,*,#5836,.F.);
#8555=ORIENTED_EDGE('',*,*,#5839,.T.);
#8556=ORIENTED_EDGE('',*,*,#5815,.T.);
#8557=ORIENTED_EDGE('',*,*,#5818,.T.);
#8558=ORIENTED_EDGE('',*,*,#5820,.T.);
#8559=ORIENTED_EDGE('',*,*,#5748,.F.);
#8560=ORIENTED_EDGE('',*,*,#5839,.F.);
#8561=ORIENTED_EDGE('',*,*,#5840,.T.);
#8562=ORIENTED_EDGE('',*,*,#5841,.T.);
#8563=ORIENTED_EDGE('',*,*,#5840,.F.);
#8564=ORIENTED_EDGE('',*,*,#5841,.F.);
#8565=ORIENTED_EDGE('',*,*,#5821,.T.);
#8566=ORIENTED_EDGE('',*,*,#5837,.T.);
#8567=ORIENTED_EDGE('',*,*,#5834,.T.);
#8568=ORIENTED_EDGE('',*,*,#5831,.T.);
#8569=ORIENTED_EDGE('',*,*,#5828,.T.);
#8570=ORIENTED_EDGE('',*,*,#5825,.T.);
#8571=ORIENTED_EDGE('',*,*,#5813,.T.);
#8572=ORIENTED_EDGE('',*,*,#5842,.F.);
#8573=ORIENTED_EDGE('',*,*,#5843,.T.);
#8574=ORIENTED_EDGE('',*,*,#5844,.T.);
#8575=ORIENTED_EDGE('',*,*,#5845,.T.);
#8576=ORIENTED_EDGE('',*,*,#5846,.F.);
#8577=ORIENTED_EDGE('',*,*,#5847,.T.);
#8578=ORIENTED_EDGE('',*,*,#5842,.T.);
#8579=ORIENTED_EDGE('',*,*,#5848,.T.);
#8580=ORIENTED_EDGE('',*,*,#5849,.F.);
#8581=ORIENTED_EDGE('',*,*,#5850,.T.);
#8582=ORIENTED_EDGE('',*,*,#5846,.T.);
#8583=ORIENTED_EDGE('',*,*,#5851,.T.);
#8584=ORIENTED_EDGE('',*,*,#5852,.F.);
#8585=ORIENTED_EDGE('',*,*,#5853,.T.);
#8586=ORIENTED_EDGE('',*,*,#5849,.T.);
#8587=ORIENTED_EDGE('',*,*,#5854,.T.);
#8588=ORIENTED_EDGE('',*,*,#5855,.F.);
#8589=ORIENTED_EDGE('',*,*,#5856,.T.);
#8590=ORIENTED_EDGE('',*,*,#5852,.T.);
#8591=ORIENTED_EDGE('',*,*,#5857,.T.);
#8592=ORIENTED_EDGE('',*,*,#5858,.F.);
#8593=ORIENTED_EDGE('',*,*,#5859,.T.);
#8594=ORIENTED_EDGE('',*,*,#5855,.T.);
#8595=ORIENTED_EDGE('',*,*,#5860,.T.);
#8596=ORIENTED_EDGE('',*,*,#5861,.F.);
#8597=ORIENTED_EDGE('',*,*,#5862,.T.);
#8598=ORIENTED_EDGE('',*,*,#5858,.T.);
#8599=ORIENTED_EDGE('',*,*,#5863,.T.);
#8600=ORIENTED_EDGE('',*,*,#5864,.F.);
#8601=ORIENTED_EDGE('',*,*,#5865,.T.);
#8602=ORIENTED_EDGE('',*,*,#5861,.T.);
#8603=ORIENTED_EDGE('',*,*,#5866,.T.);
#8604=ORIENTED_EDGE('',*,*,#5867,.F.);
#8605=ORIENTED_EDGE('',*,*,#5868,.T.);
#8606=ORIENTED_EDGE('',*,*,#5864,.T.);
#8607=ORIENTED_EDGE('',*,*,#5869,.T.);
#8608=ORIENTED_EDGE('',*,*,#5870,.F.);
#8609=ORIENTED_EDGE('',*,*,#5871,.T.);
#8610=ORIENTED_EDGE('',*,*,#5867,.T.);
#8611=ORIENTED_EDGE('',*,*,#5872,.T.);
#8612=ORIENTED_EDGE('',*,*,#5873,.F.);
#8613=ORIENTED_EDGE('',*,*,#5874,.T.);
#8614=ORIENTED_EDGE('',*,*,#5870,.T.);
#8615=ORIENTED_EDGE('',*,*,#5875,.T.);
#8616=ORIENTED_EDGE('',*,*,#5876,.F.);
#8617=ORIENTED_EDGE('',*,*,#5877,.T.);
#8618=ORIENTED_EDGE('',*,*,#5873,.T.);
#8619=ORIENTED_EDGE('',*,*,#5878,.T.);
#8620=ORIENTED_EDGE('',*,*,#5879,.F.);
#8621=ORIENTED_EDGE('',*,*,#5880,.T.);
#8622=ORIENTED_EDGE('',*,*,#5876,.T.);
#8623=ORIENTED_EDGE('',*,*,#5881,.T.);
#8624=ORIENTED_EDGE('',*,*,#5882,.F.);
#8625=ORIENTED_EDGE('',*,*,#5883,.T.);
#8626=ORIENTED_EDGE('',*,*,#5879,.T.);
#8627=ORIENTED_EDGE('',*,*,#5884,.T.);
#8628=ORIENTED_EDGE('',*,*,#5885,.F.);
#8629=ORIENTED_EDGE('',*,*,#5886,.T.);
#8630=ORIENTED_EDGE('',*,*,#5882,.T.);
#8631=ORIENTED_EDGE('',*,*,#5887,.T.);
#8632=ORIENTED_EDGE('',*,*,#5888,.F.);
#8633=ORIENTED_EDGE('',*,*,#5889,.T.);
#8634=ORIENTED_EDGE('',*,*,#5885,.T.);
#8635=ORIENTED_EDGE('',*,*,#5890,.T.);
#8636=ORIENTED_EDGE('',*,*,#5891,.F.);
#8637=ORIENTED_EDGE('',*,*,#5892,.T.);
#8638=ORIENTED_EDGE('',*,*,#5888,.T.);
#8639=ORIENTED_EDGE('',*,*,#5893,.T.);
#8640=ORIENTED_EDGE('',*,*,#5894,.F.);
#8641=ORIENTED_EDGE('',*,*,#5895,.T.);
#8642=ORIENTED_EDGE('',*,*,#5891,.T.);
#8643=ORIENTED_EDGE('',*,*,#5896,.T.);
#8644=ORIENTED_EDGE('',*,*,#5897,.F.);
#8645=ORIENTED_EDGE('',*,*,#5898,.T.);
#8646=ORIENTED_EDGE('',*,*,#5899,.T.);
#8647=ORIENTED_EDGE('',*,*,#5900,.F.);
#8648=ORIENTED_EDGE('',*,*,#5901,.F.);
#8649=ORIENTED_EDGE('',*,*,#5902,.T.);
#8650=ORIENTED_EDGE('',*,*,#5897,.T.);
#8651=ORIENTED_EDGE('',*,*,#5903,.F.);
#8652=ORIENTED_EDGE('',*,*,#5904,.F.);
#8653=ORIENTED_EDGE('',*,*,#5905,.T.);
#8654=ORIENTED_EDGE('',*,*,#5901,.T.);
#8655=ORIENTED_EDGE('',*,*,#5906,.F.);
#8656=ORIENTED_EDGE('',*,*,#5907,.F.);
#8657=ORIENTED_EDGE('',*,*,#5908,.T.);
#8658=ORIENTED_EDGE('',*,*,#5904,.T.);
#8659=ORIENTED_EDGE('',*,*,#5909,.F.);
#8660=ORIENTED_EDGE('',*,*,#5910,.F.);
#8661=ORIENTED_EDGE('',*,*,#5911,.T.);
#8662=ORIENTED_EDGE('',*,*,#5907,.T.);
#8663=ORIENTED_EDGE('',*,*,#5912,.F.);
#8664=ORIENTED_EDGE('',*,*,#5913,.F.);
#8665=ORIENTED_EDGE('',*,*,#5914,.T.);
#8666=ORIENTED_EDGE('',*,*,#5910,.T.);
#8667=ORIENTED_EDGE('',*,*,#5915,.F.);
#8668=ORIENTED_EDGE('',*,*,#5916,.F.);
#8669=ORIENTED_EDGE('',*,*,#5917,.T.);
#8670=ORIENTED_EDGE('',*,*,#5913,.T.);
#8671=ORIENTED_EDGE('',*,*,#5918,.F.);
#8672=ORIENTED_EDGE('',*,*,#5919,.F.);
#8673=ORIENTED_EDGE('',*,*,#5920,.T.);
#8674=ORIENTED_EDGE('',*,*,#5916,.T.);
#8675=ORIENTED_EDGE('',*,*,#5921,.F.);
#8676=ORIENTED_EDGE('',*,*,#5922,.F.);
#8677=ORIENTED_EDGE('',*,*,#5923,.T.);
#8678=ORIENTED_EDGE('',*,*,#5919,.T.);
#8679=ORIENTED_EDGE('',*,*,#5924,.F.);
#8680=ORIENTED_EDGE('',*,*,#5925,.F.);
#8681=ORIENTED_EDGE('',*,*,#5926,.T.);
#8682=ORIENTED_EDGE('',*,*,#5922,.T.);
#8683=ORIENTED_EDGE('',*,*,#5927,.F.);
#8684=ORIENTED_EDGE('',*,*,#5928,.F.);
#8685=ORIENTED_EDGE('',*,*,#5929,.T.);
#8686=ORIENTED_EDGE('',*,*,#5925,.T.);
#8687=ORIENTED_EDGE('',*,*,#5930,.F.);
#8688=ORIENTED_EDGE('',*,*,#5931,.F.);
#8689=ORIENTED_EDGE('',*,*,#5932,.T.);
#8690=ORIENTED_EDGE('',*,*,#5928,.T.);
#8691=ORIENTED_EDGE('',*,*,#5933,.F.);
#8692=ORIENTED_EDGE('',*,*,#5934,.F.);
#8693=ORIENTED_EDGE('',*,*,#5935,.T.);
#8694=ORIENTED_EDGE('',*,*,#5931,.T.);
#8695=ORIENTED_EDGE('',*,*,#5936,.F.);
#8696=ORIENTED_EDGE('',*,*,#5937,.F.);
#8697=ORIENTED_EDGE('',*,*,#5938,.T.);
#8698=ORIENTED_EDGE('',*,*,#5934,.T.);
#8699=ORIENTED_EDGE('',*,*,#5939,.F.);
#8700=ORIENTED_EDGE('',*,*,#5940,.F.);
#8701=ORIENTED_EDGE('',*,*,#5941,.T.);
#8702=ORIENTED_EDGE('',*,*,#5937,.T.);
#8703=ORIENTED_EDGE('',*,*,#5942,.F.);
#8704=ORIENTED_EDGE('',*,*,#5943,.F.);
#8705=ORIENTED_EDGE('',*,*,#5944,.T.);
#8706=ORIENTED_EDGE('',*,*,#5940,.T.);
#8707=ORIENTED_EDGE('',*,*,#5945,.F.);
#8708=ORIENTED_EDGE('',*,*,#5946,.F.);
#8709=ORIENTED_EDGE('',*,*,#5947,.T.);
#8710=ORIENTED_EDGE('',*,*,#5943,.T.);
#8711=ORIENTED_EDGE('',*,*,#5948,.F.);
#8712=ORIENTED_EDGE('',*,*,#5949,.F.);
#8713=ORIENTED_EDGE('',*,*,#5950,.T.);
#8714=ORIENTED_EDGE('',*,*,#5946,.T.);
#8715=ORIENTED_EDGE('',*,*,#5951,.F.);
#8716=ORIENTED_EDGE('',*,*,#5952,.F.);
#8717=ORIENTED_EDGE('',*,*,#5899,.F.);
#8718=ORIENTED_EDGE('',*,*,#5953,.F.);
#8719=ORIENTED_EDGE('',*,*,#5954,.F.);
#8720=ORIENTED_EDGE('',*,*,#5955,.F.);
#8721=ORIENTED_EDGE('',*,*,#5956,.T.);
#8722=ORIENTED_EDGE('',*,*,#5957,.F.);
#8723=ORIENTED_EDGE('',*,*,#5956,.F.);
#8724=ORIENTED_EDGE('',*,*,#5953,.T.);
#8725=ORIENTED_EDGE('',*,*,#5898,.F.);
#8726=ORIENTED_EDGE('',*,*,#5902,.F.);
#8727=ORIENTED_EDGE('',*,*,#5905,.F.);
#8728=ORIENTED_EDGE('',*,*,#5908,.F.);
#8729=ORIENTED_EDGE('',*,*,#5911,.F.);
#8730=ORIENTED_EDGE('',*,*,#5914,.F.);
#8731=ORIENTED_EDGE('',*,*,#5917,.F.);
#8732=ORIENTED_EDGE('',*,*,#5920,.F.);
#8733=ORIENTED_EDGE('',*,*,#5923,.F.);
#8734=ORIENTED_EDGE('',*,*,#5926,.F.);
#8735=ORIENTED_EDGE('',*,*,#5929,.F.);
#8736=ORIENTED_EDGE('',*,*,#5932,.F.);
#8737=ORIENTED_EDGE('',*,*,#5935,.F.);
#8738=ORIENTED_EDGE('',*,*,#5938,.F.);
#8739=ORIENTED_EDGE('',*,*,#5941,.F.);
#8740=ORIENTED_EDGE('',*,*,#5944,.F.);
#8741=ORIENTED_EDGE('',*,*,#5947,.F.);
#8742=ORIENTED_EDGE('',*,*,#5950,.F.);
#8743=ORIENTED_EDGE('',*,*,#5958,.F.);
#8744=ORIENTED_EDGE('',*,*,#5959,.F.);
#8745=ORIENTED_EDGE('',*,*,#5843,.F.);
#8746=ORIENTED_EDGE('',*,*,#5847,.F.);
#8747=ORIENTED_EDGE('',*,*,#5850,.F.);
#8748=ORIENTED_EDGE('',*,*,#5853,.F.);
#8749=ORIENTED_EDGE('',*,*,#5856,.F.);
#8750=ORIENTED_EDGE('',*,*,#5859,.F.);
#8751=ORIENTED_EDGE('',*,*,#5862,.F.);
#8752=ORIENTED_EDGE('',*,*,#5865,.F.);
#8753=ORIENTED_EDGE('',*,*,#5868,.F.);
#8754=ORIENTED_EDGE('',*,*,#5871,.F.);
#8755=ORIENTED_EDGE('',*,*,#5874,.F.);
#8756=ORIENTED_EDGE('',*,*,#5877,.F.);
#8757=ORIENTED_EDGE('',*,*,#5880,.F.);
#8758=ORIENTED_EDGE('',*,*,#5883,.F.);
#8759=ORIENTED_EDGE('',*,*,#5886,.F.);
#8760=ORIENTED_EDGE('',*,*,#5889,.F.);
#8761=ORIENTED_EDGE('',*,*,#5892,.F.);
#8762=ORIENTED_EDGE('',*,*,#5895,.F.);
#8763=ORIENTED_EDGE('',*,*,#5960,.F.);
#8764=ORIENTED_EDGE('',*,*,#5949,.T.);
#8765=ORIENTED_EDGE('',*,*,#5961,.F.);
#8766=ORIENTED_EDGE('',*,*,#5962,.F.);
#8767=ORIENTED_EDGE('',*,*,#5958,.T.);
#8768=ORIENTED_EDGE('',*,*,#5952,.T.);
#8769=ORIENTED_EDGE('',*,*,#5955,.T.);
#8770=ORIENTED_EDGE('',*,*,#5963,.F.);
#8771=ORIENTED_EDGE('',*,*,#5896,.F.);
#8772=ORIENTED_EDGE('',*,*,#5893,.F.);
#8773=ORIENTED_EDGE('',*,*,#5890,.F.);
#8774=ORIENTED_EDGE('',*,*,#5887,.F.);
#8775=ORIENTED_EDGE('',*,*,#5884,.F.);
#8776=ORIENTED_EDGE('',*,*,#5881,.F.);
#8777=ORIENTED_EDGE('',*,*,#5878,.F.);
#8778=ORIENTED_EDGE('',*,*,#5875,.F.);
#8779=ORIENTED_EDGE('',*,*,#5872,.F.);
#8780=ORIENTED_EDGE('',*,*,#5869,.F.);
#8781=ORIENTED_EDGE('',*,*,#5866,.F.);
#8782=ORIENTED_EDGE('',*,*,#5863,.F.);
#8783=ORIENTED_EDGE('',*,*,#5860,.F.);
#8784=ORIENTED_EDGE('',*,*,#5857,.F.);
#8785=ORIENTED_EDGE('',*,*,#5854,.F.);
#8786=ORIENTED_EDGE('',*,*,#5851,.F.);
#8787=ORIENTED_EDGE('',*,*,#5848,.F.);
#8788=ORIENTED_EDGE('',*,*,#5845,.F.);
#8789=ORIENTED_EDGE('',*,*,#5964,.F.);
#8790=ORIENTED_EDGE('',*,*,#5961,.T.);
#8791=ORIENTED_EDGE('',*,*,#5951,.T.);
#8792=ORIENTED_EDGE('',*,*,#5948,.T.);
#8793=ORIENTED_EDGE('',*,*,#5945,.T.);
#8794=ORIENTED_EDGE('',*,*,#5942,.T.);
#8795=ORIENTED_EDGE('',*,*,#5939,.T.);
#8796=ORIENTED_EDGE('',*,*,#5936,.T.);
#8797=ORIENTED_EDGE('',*,*,#5933,.T.);
#8798=ORIENTED_EDGE('',*,*,#5930,.T.);
#8799=ORIENTED_EDGE('',*,*,#5927,.T.);
#8800=ORIENTED_EDGE('',*,*,#5924,.T.);
#8801=ORIENTED_EDGE('',*,*,#5921,.T.);
#8802=ORIENTED_EDGE('',*,*,#5918,.T.);
#8803=ORIENTED_EDGE('',*,*,#5915,.T.);
#8804=ORIENTED_EDGE('',*,*,#5912,.T.);
#8805=ORIENTED_EDGE('',*,*,#5909,.T.);
#8806=ORIENTED_EDGE('',*,*,#5906,.T.);
#8807=ORIENTED_EDGE('',*,*,#5903,.T.);
#8808=ORIENTED_EDGE('',*,*,#5900,.T.);
#8809=ORIENTED_EDGE('',*,*,#5894,.T.);
#8810=ORIENTED_EDGE('',*,*,#5963,.T.);
#8811=ORIENTED_EDGE('',*,*,#5954,.T.);
#8812=ORIENTED_EDGE('',*,*,#5960,.T.);
#8813=ORIENTED_EDGE('',*,*,#5965,.F.);
#8814=ORIENTED_EDGE('',*,*,#5966,.T.);
#8815=ORIENTED_EDGE('',*,*,#5967,.T.);
#8816=ORIENTED_EDGE('',*,*,#5968,.F.);
#8817=ORIENTED_EDGE('',*,*,#5969,.F.);
#8818=ORIENTED_EDGE('',*,*,#5970,.T.);
#8819=ORIENTED_EDGE('',*,*,#5971,.T.);
#8820=ORIENTED_EDGE('',*,*,#5966,.F.);
#8821=ORIENTED_EDGE('',*,*,#5972,.F.);
#8822=ORIENTED_EDGE('',*,*,#5973,.T.);
#8823=ORIENTED_EDGE('',*,*,#5974,.T.);
#8824=ORIENTED_EDGE('',*,*,#5970,.F.);
#8825=ORIENTED_EDGE('',*,*,#5975,.F.);
#8826=ORIENTED_EDGE('',*,*,#5976,.T.);
#8827=ORIENTED_EDGE('',*,*,#5977,.T.);
#8828=ORIENTED_EDGE('',*,*,#5973,.F.);
#8829=ORIENTED_EDGE('',*,*,#5978,.F.);
#8830=ORIENTED_EDGE('',*,*,#5979,.T.);
#8831=ORIENTED_EDGE('',*,*,#5980,.T.);
#8832=ORIENTED_EDGE('',*,*,#5976,.F.);
#8833=ORIENTED_EDGE('',*,*,#5981,.F.);
#8834=ORIENTED_EDGE('',*,*,#5968,.T.);
#8835=ORIENTED_EDGE('',*,*,#5982,.T.);
#8836=ORIENTED_EDGE('',*,*,#5979,.F.);
#8837=ORIENTED_EDGE('',*,*,#5982,.F.);
#8838=ORIENTED_EDGE('',*,*,#5967,.F.);
#8839=ORIENTED_EDGE('',*,*,#5971,.F.);
#8840=ORIENTED_EDGE('',*,*,#5974,.F.);
#8841=ORIENTED_EDGE('',*,*,#5977,.F.);
#8842=ORIENTED_EDGE('',*,*,#5980,.F.);
#8843=ORIENTED_EDGE('',*,*,#5983,.T.);
#8844=ORIENTED_EDGE('',*,*,#5959,.T.);
#8845=ORIENTED_EDGE('',*,*,#5962,.T.);
#8846=ORIENTED_EDGE('',*,*,#5964,.T.);
#8847=ORIENTED_EDGE('',*,*,#5844,.F.);
#8848=ORIENTED_EDGE('',*,*,#5983,.F.);
#8849=ORIENTED_EDGE('',*,*,#5984,.T.);
#8850=ORIENTED_EDGE('',*,*,#5985,.T.);
#8851=ORIENTED_EDGE('',*,*,#5984,.F.);
#8852=ORIENTED_EDGE('',*,*,#5985,.F.);
#8853=ORIENTED_EDGE('',*,*,#5965,.T.);
#8854=ORIENTED_EDGE('',*,*,#5981,.T.);
#8855=ORIENTED_EDGE('',*,*,#5978,.T.);
#8856=ORIENTED_EDGE('',*,*,#5975,.T.);
#8857=ORIENTED_EDGE('',*,*,#5972,.T.);
#8858=ORIENTED_EDGE('',*,*,#5969,.T.);
#8859=ORIENTED_EDGE('',*,*,#5957,.T.);
#8860=CYLINDRICAL_SURFACE('',#9974,0.1666);
#8861=CYLINDRICAL_SURFACE('',#9977,0.1666);
#8862=CYLINDRICAL_SURFACE('',#9978,0.1666);
#8863=CYLINDRICAL_SURFACE('',#9979,0.1666);
#8864=CYLINDRICAL_SURFACE('',#9980,0.1666);
#8865=CYLINDRICAL_SURFACE('',#9981,0.1666);
#8866=CYLINDRICAL_SURFACE('',#9982,0.1666);
#8867=CYLINDRICAL_SURFACE('',#9983,0.1666);
#8868=CYLINDRICAL_SURFACE('',#9984,0.1666);
#8869=CYLINDRICAL_SURFACE('',#9985,0.1666);
#8870=CYLINDRICAL_SURFACE('',#9986,0.1666);
#8871=CYLINDRICAL_SURFACE('',#9987,0.1666);
#8872=CYLINDRICAL_SURFACE('',#9989,0.205475);
#8873=CYLINDRICAL_SURFACE('',#9991,0.205475);
#8874=CYLINDRICAL_SURFACE('',#9992,0.205475);
#8875=CYLINDRICAL_SURFACE('',#9993,0.205475);
#8876=CYLINDRICAL_SURFACE('',#9994,0.205475);
#8877=CYLINDRICAL_SURFACE('',#9995,0.205475);
#8878=CYLINDRICAL_SURFACE('',#9996,0.205475);
#8879=CYLINDRICAL_SURFACE('',#9997,0.205475);
#8880=CYLINDRICAL_SURFACE('',#9998,0.205475);
#8881=CYLINDRICAL_SURFACE('',#9999,0.205475);
#8882=CYLINDRICAL_SURFACE('',#10000,0.205475);
#8883=CYLINDRICAL_SURFACE('',#10001,0.205475);
#8884=CYLINDRICAL_SURFACE('',#10002,0.205475);
#8885=CYLINDRICAL_SURFACE('',#10004,0.1666);
#8886=CYLINDRICAL_SURFACE('',#10007,0.1666);
#8887=CYLINDRICAL_SURFACE('',#10008,0.1666);
#8888=CYLINDRICAL_SURFACE('',#10009,0.1666);
#8889=CYLINDRICAL_SURFACE('',#10010,0.1666);
#8890=CYLINDRICAL_SURFACE('',#10011,0.1666);
#8891=CYLINDRICAL_SURFACE('',#10012,0.1666);
#8892=CYLINDRICAL_SURFACE('',#10013,0.1666);
#8893=CYLINDRICAL_SURFACE('',#10014,0.1666);
#8894=CYLINDRICAL_SURFACE('',#10015,0.1666);
#8895=CYLINDRICAL_SURFACE('',#10016,0.1666);
#8896=CYLINDRICAL_SURFACE('',#10017,0.1666);
#8897=CYLINDRICAL_SURFACE('',#10019,0.205475000000001);
#8898=CYLINDRICAL_SURFACE('',#10021,0.205475000000001);
#8899=CYLINDRICAL_SURFACE('',#10022,0.205475000000001);
#8900=CYLINDRICAL_SURFACE('',#10023,0.205475000000001);
#8901=CYLINDRICAL_SURFACE('',#10024,0.205475000000001);
#8902=CYLINDRICAL_SURFACE('',#10025,0.205475000000001);
#8903=CYLINDRICAL_SURFACE('',#10026,0.205475000000001);
#8904=CYLINDRICAL_SURFACE('',#10027,0.205475000000001);
#8905=CYLINDRICAL_SURFACE('',#10028,0.205475000000001);
#8906=CYLINDRICAL_SURFACE('',#10029,0.205475000000001);
#8907=CYLINDRICAL_SURFACE('',#10030,0.205475000000001);
#8908=CYLINDRICAL_SURFACE('',#10031,0.205475000000001);
#8909=CYLINDRICAL_SURFACE('',#10032,0.205475000000001);
#8910=CYLINDRICAL_SURFACE('',#10034,0.1666);
#8911=CYLINDRICAL_SURFACE('',#10037,0.1666);
#8912=CYLINDRICAL_SURFACE('',#10038,0.1666);
#8913=CYLINDRICAL_SURFACE('',#10039,0.1666);
#8914=CYLINDRICAL_SURFACE('',#10040,0.1666);
#8915=CYLINDRICAL_SURFACE('',#10041,0.1666);
#8916=CYLINDRICAL_SURFACE('',#10042,0.1666);
#8917=CYLINDRICAL_SURFACE('',#10043,0.1666);
#8918=CYLINDRICAL_SURFACE('',#10044,0.1666);
#8919=CYLINDRICAL_SURFACE('',#10045,0.1666);
#8920=CYLINDRICAL_SURFACE('',#10046,0.1666);
#8921=CYLINDRICAL_SURFACE('',#10047,0.1666);
#8922=CYLINDRICAL_SURFACE('',#10049,0.205475000000001);
#8923=CYLINDRICAL_SURFACE('',#10051,0.205475000000001);
#8924=CYLINDRICAL_SURFACE('',#10052,0.205475000000001);
#8925=CYLINDRICAL_SURFACE('',#10053,0.205475000000001);
#8926=CYLINDRICAL_SURFACE('',#10054,0.205475000000001);
#8927=CYLINDRICAL_SURFACE('',#10055,0.205475000000001);
#8928=CYLINDRICAL_SURFACE('',#10056,0.205475000000001);
#8929=CYLINDRICAL_SURFACE('',#10057,0.205475000000001);
#8930=CYLINDRICAL_SURFACE('',#10058,0.205475000000001);
#8931=CYLINDRICAL_SURFACE('',#10059,0.205475000000001);
#8932=CYLINDRICAL_SURFACE('',#10060,0.205475000000001);
#8933=CYLINDRICAL_SURFACE('',#10061,0.205475000000001);
#8934=CYLINDRICAL_SURFACE('',#10062,0.205475000000001);
#8935=CYLINDRICAL_SURFACE('',#10064,0.1666);
#8936=CYLINDRICAL_SURFACE('',#10067,0.1666);
#8937=CYLINDRICAL_SURFACE('',#10068,0.1666);
#8938=CYLINDRICAL_SURFACE('',#10069,0.1666);
#8939=CYLINDRICAL_SURFACE('',#10070,0.1666);
#8940=CYLINDRICAL_SURFACE('',#10071,0.1666);
#8941=CYLINDRICAL_SURFACE('',#10072,0.1666);
#8942=CYLINDRICAL_SURFACE('',#10073,0.1666);
#8943=CYLINDRICAL_SURFACE('',#10074,0.1666);
#8944=CYLINDRICAL_SURFACE('',#10075,0.1666);
#8945=CYLINDRICAL_SURFACE('',#10076,0.1666);
#8946=CYLINDRICAL_SURFACE('',#10077,0.1666);
#8947=CYLINDRICAL_SURFACE('',#10079,0.205475);
#8948=CYLINDRICAL_SURFACE('',#10081,0.205475);
#8949=CYLINDRICAL_SURFACE('',#10082,0.205475);
#8950=CYLINDRICAL_SURFACE('',#10083,0.205475);
#8951=CYLINDRICAL_SURFACE('',#10084,0.205475);
#8952=CYLINDRICAL_SURFACE('',#10085,0.205475);
#8953=CYLINDRICAL_SURFACE('',#10086,0.205475);
#8954=CYLINDRICAL_SURFACE('',#10087,0.205475);
#8955=CYLINDRICAL_SURFACE('',#10088,0.205475);
#8956=CYLINDRICAL_SURFACE('',#10089,0.205475);
#8957=CYLINDRICAL_SURFACE('',#10090,0.205475);
#8958=CYLINDRICAL_SURFACE('',#10091,0.205475);
#8959=CYLINDRICAL_SURFACE('',#10092,0.205475);
#8960=CYLINDRICAL_SURFACE('',#10094,0.2);
#8961=CYLINDRICAL_SURFACE('',#10098,0.2);
#8962=CYLINDRICAL_SURFACE('',#10102,0.2);
#8963=CYLINDRICAL_SURFACE('',#10112,0.2);
#8964=CYLINDRICAL_SURFACE('',#10114,0.6);
#8965=CYLINDRICAL_SURFACE('',#10119,0.4);
#8966=CYLINDRICAL_SURFACE('',#10121,0.25);
#8967=CYLINDRICAL_SURFACE('',#10125,0.4);
#8968=CYLINDRICAL_SURFACE('',#10127,0.25);
#8969=CYLINDRICAL_SURFACE('',#10129,0.205475);
#8970=CYLINDRICAL_SURFACE('',#10130,0.1666);
#8971=CYLINDRICAL_SURFACE('',#10132,0.205475000000001);
#8972=CYLINDRICAL_SURFACE('',#10133,0.1666);
#8973=CYLINDRICAL_SURFACE('',#10135,0.205475000000001);
#8974=CYLINDRICAL_SURFACE('',#10136,0.1666);
#8975=CYLINDRICAL_SURFACE('',#10138,0.205475);
#8976=CYLINDRICAL_SURFACE('',#10139,0.1666);
#8977=CYLINDRICAL_SURFACE('',#10144,0.3);
#8978=CYLINDRICAL_SURFACE('',#10147,0.3);
#8979=CYLINDRICAL_SURFACE('',#10158,0.65);
#8980=CYLINDRICAL_SURFACE('',#10161,0.8);
#8981=CYLINDRICAL_SURFACE('',#10173,0.25);
#8982=CYLINDRICAL_SURFACE('',#10176,0.25);
#8983=CYLINDRICAL_SURFACE('',#10179,0.25);
#8984=CYLINDRICAL_SURFACE('',#10182,0.25);
#8985=CYLINDRICAL_SURFACE('',#10185,0.6);
#8986=CYLINDRICAL_SURFACE('',#10198,0.8);
#8987=CYLINDRICAL_SURFACE('',#10202,0.4);
#8988=CYLINDRICAL_SURFACE('',#10204,0.6);
#8989=CYLINDRICAL_SURFACE('',#10208,0.12645);
#8990=CYLINDRICAL_SURFACE('',#10210,0.12645);
#8991=CYLINDRICAL_SURFACE('',#10211,0.12645);
#8992=CYLINDRICAL_SURFACE('',#10212,0.12645);
#8993=CYLINDRICAL_SURFACE('',#10213,0.12645);
#8994=CYLINDRICAL_SURFACE('',#10214,0.12645);
#8995=CYLINDRICAL_SURFACE('',#10215,0.12645);
#8996=CYLINDRICAL_SURFACE('',#10216,0.12645);
#8997=CYLINDRICAL_SURFACE('',#10218,0.12645);
#8998=CYLINDRICAL_SURFACE('',#10220,0.12645);
#8999=CYLINDRICAL_SURFACE('',#10221,0.12645);
#9000=CYLINDRICAL_SURFACE('',#10222,0.12645);
#9001=CYLINDRICAL_SURFACE('',#10223,0.12645);
#9002=CYLINDRICAL_SURFACE('',#10224,0.12645);
#9003=CYLINDRICAL_SURFACE('',#10225,0.12645);
#9004=CYLINDRICAL_SURFACE('',#10226,0.12645);
#9005=CYLINDRICAL_SURFACE('',#10228,0.1543);
#9006=CYLINDRICAL_SURFACE('',#10230,0.1543);
#9007=CYLINDRICAL_SURFACE('',#10231,0.1543);
#9008=CYLINDRICAL_SURFACE('',#10232,0.1543);
#9009=CYLINDRICAL_SURFACE('',#10233,0.1543);
#9010=CYLINDRICAL_SURFACE('',#10234,0.1543);
#9011=CYLINDRICAL_SURFACE('',#10235,0.1543);
#9012=CYLINDRICAL_SURFACE('',#10236,0.1543);
#9013=CYLINDRICAL_SURFACE('',#10238,0.1543);
#9014=CYLINDRICAL_SURFACE('',#10240,0.1543);
#9015=CYLINDRICAL_SURFACE('',#10241,0.1543);
#9016=CYLINDRICAL_SURFACE('',#10242,0.1543);
#9017=CYLINDRICAL_SURFACE('',#10243,0.1543);
#9018=CYLINDRICAL_SURFACE('',#10244,0.1543);
#9019=CYLINDRICAL_SURFACE('',#10245,0.1543);
#9020=CYLINDRICAL_SURFACE('',#10246,0.1543);
#9021=CYLINDRICAL_SURFACE('',#10248,0.1543);
#9022=CYLINDRICAL_SURFACE('',#10251,0.1543);
#9023=CYLINDRICAL_SURFACE('',#10252,0.12645);
#9024=CYLINDRICAL_SURFACE('',#10253,0.12645);
#9025=CYLINDRICAL_SURFACE('',#10254,0.2);
#9026=CYLINDRICAL_SURFACE('',#10257,0.2);
#9027=CYLINDRICAL_SURFACE('',#10279,1.);
#9028=CYLINDRICAL_SURFACE('',#10281,0.6);
#9029=CYLINDRICAL_SURFACE('',#10285,0.2);
#9030=CYLINDRICAL_SURFACE('',#10288,0.2);
#9031=CYLINDRICAL_SURFACE('',#10301,0.7);
#9032=CYLINDRICAL_SURFACE('',#10311,0.3);
#9033=CYLINDRICAL_SURFACE('',#10315,0.1666);
#9034=CYLINDRICAL_SURFACE('',#10318,0.1666);
#9035=CYLINDRICAL_SURFACE('',#10319,0.1666);
#9036=CYLINDRICAL_SURFACE('',#10320,0.1666);
#9037=CYLINDRICAL_SURFACE('',#10321,0.1666);
#9038=CYLINDRICAL_SURFACE('',#10322,0.1666);
#9039=CYLINDRICAL_SURFACE('',#10323,0.1666);
#9040=CYLINDRICAL_SURFACE('',#10324,0.1666);
#9041=CYLINDRICAL_SURFACE('',#10325,0.1666);
#9042=CYLINDRICAL_SURFACE('',#10326,0.1666);
#9043=CYLINDRICAL_SURFACE('',#10327,0.1666);
#9044=CYLINDRICAL_SURFACE('',#10328,0.1666);
#9045=CYLINDRICAL_SURFACE('',#10330,0.205475);
#9046=CYLINDRICAL_SURFACE('',#10332,0.205475);
#9047=CYLINDRICAL_SURFACE('',#10333,0.205475);
#9048=CYLINDRICAL_SURFACE('',#10334,0.205475);
#9049=CYLINDRICAL_SURFACE('',#10335,0.205475);
#9050=CYLINDRICAL_SURFACE('',#10336,0.205475);
#9051=CYLINDRICAL_SURFACE('',#10337,0.205475);
#9052=CYLINDRICAL_SURFACE('',#10338,0.205475);
#9053=CYLINDRICAL_SURFACE('',#10339,0.205475);
#9054=CYLINDRICAL_SURFACE('',#10340,0.205475);
#9055=CYLINDRICAL_SURFACE('',#10341,0.205475);
#9056=CYLINDRICAL_SURFACE('',#10342,0.205475);
#9057=CYLINDRICAL_SURFACE('',#10343,0.205475);
#9058=CYLINDRICAL_SURFACE('',#10345,0.12645);
#9059=CYLINDRICAL_SURFACE('',#10349,0.12645);
#9060=CYLINDRICAL_SURFACE('',#10350,0.12645);
#9061=CYLINDRICAL_SURFACE('',#10351,0.12645);
#9062=CYLINDRICAL_SURFACE('',#10352,0.12645);
#9063=CYLINDRICAL_SURFACE('',#10353,0.12645);
#9064=CYLINDRICAL_SURFACE('',#10354,0.12645);
#9065=CYLINDRICAL_SURFACE('',#10355,0.12645);
#9066=CYLINDRICAL_SURFACE('',#10356,0.12645);
#9067=CYLINDRICAL_SURFACE('',#10357,0.12645);
#9068=CYLINDRICAL_SURFACE('',#10358,0.12645);
#9069=CYLINDRICAL_SURFACE('',#10359,0.12645);
#9070=CYLINDRICAL_SURFACE('',#10360,0.12645);
#9071=CYLINDRICAL_SURFACE('',#10361,0.12645);
#9072=CYLINDRICAL_SURFACE('',#10362,0.12645);
#9073=CYLINDRICAL_SURFACE('',#10363,0.12645);
#9074=CYLINDRICAL_SURFACE('',#10364,0.12645);
#9075=CYLINDRICAL_SURFACE('',#10365,0.12645);
#9076=CYLINDRICAL_SURFACE('',#10367,0.1543);
#9077=CYLINDRICAL_SURFACE('',#10369,0.1543);
#9078=CYLINDRICAL_SURFACE('',#10370,0.1543);
#9079=CYLINDRICAL_SURFACE('',#10371,0.1543);
#9080=CYLINDRICAL_SURFACE('',#10372,0.1543);
#9081=CYLINDRICAL_SURFACE('',#10373,0.1543);
#9082=CYLINDRICAL_SURFACE('',#10374,0.1543);
#9083=CYLINDRICAL_SURFACE('',#10375,0.1543);
#9084=CYLINDRICAL_SURFACE('',#10376,0.1543);
#9085=CYLINDRICAL_SURFACE('',#10377,0.1543);
#9086=CYLINDRICAL_SURFACE('',#10378,0.1543);
#9087=CYLINDRICAL_SURFACE('',#10379,0.1543);
#9088=CYLINDRICAL_SURFACE('',#10380,0.1543);
#9089=CYLINDRICAL_SURFACE('',#10381,0.1543);
#9090=CYLINDRICAL_SURFACE('',#10382,0.1543);
#9091=CYLINDRICAL_SURFACE('',#10383,0.1543);
#9092=CYLINDRICAL_SURFACE('',#10384,0.1543);
#9093=CYLINDRICAL_SURFACE('',#10385,0.1543);
#9094=CYLINDRICAL_SURFACE('',#10388,0.1543);
#9095=CYLINDRICAL_SURFACE('',#10389,0.12645);
#9096=CYLINDRICAL_SURFACE('',#10392,0.205475);
#9097=CYLINDRICAL_SURFACE('',#10393,0.1666);
#9098=CYLINDRICAL_SURFACE('',#10402,0.12645);
#9099=CYLINDRICAL_SURFACE('',#10406,0.12645);
#9100=CYLINDRICAL_SURFACE('',#10407,0.12645);
#9101=CYLINDRICAL_SURFACE('',#10408,0.12645);
#9102=CYLINDRICAL_SURFACE('',#10409,0.12645);
#9103=CYLINDRICAL_SURFACE('',#10410,0.12645);
#9104=CYLINDRICAL_SURFACE('',#10411,0.12645);
#9105=CYLINDRICAL_SURFACE('',#10412,0.12645);
#9106=CYLINDRICAL_SURFACE('',#10413,0.12645);
#9107=CYLINDRICAL_SURFACE('',#10414,0.12645);
#9108=CYLINDRICAL_SURFACE('',#10416,0.1543);
#9109=CYLINDRICAL_SURFACE('',#10418,0.1543);
#9110=CYLINDRICAL_SURFACE('',#10419,0.1543);
#9111=CYLINDRICAL_SURFACE('',#10420,0.1543);
#9112=CYLINDRICAL_SURFACE('',#10421,0.1543);
#9113=CYLINDRICAL_SURFACE('',#10422,0.1543);
#9114=CYLINDRICAL_SURFACE('',#10423,0.1543);
#9115=CYLINDRICAL_SURFACE('',#10424,0.1543);
#9116=CYLINDRICAL_SURFACE('',#10425,0.1543);
#9117=CYLINDRICAL_SURFACE('',#10426,0.1543);
#9118=CYLINDRICAL_SURFACE('',#10429,0.1543);
#9119=CYLINDRICAL_SURFACE('',#10430,0.12645);
#9120=CYLINDRICAL_SURFACE('',#10432,0.2);
#9121=CYLINDRICAL_SURFACE('',#10444,0.2);
#9122=CYLINDRICAL_SURFACE('',#10454,0.2);
#9123=CYLINDRICAL_SURFACE('',#10457,0.3);
#9124=CYLINDRICAL_SURFACE('',#10463,0.15);
#9125=CYLINDRICAL_SURFACE('',#10470,0.2);
#9126=CYLINDRICAL_SURFACE('',#10475,0.4);
#9127=CYLINDRICAL_SURFACE('',#10478,0.2);
#9128=CYLINDRICAL_SURFACE('',#10486,0.15);
#9129=CYLINDRICAL_SURFACE('',#10488,0.35);
#9130=CYLINDRICAL_SURFACE('',#10497,0.2);
#9131=CYLINDRICAL_SURFACE('',#10500,0.4);
#9132=CYLINDRICAL_SURFACE('',#10506,0.1954);
#9133=CYLINDRICAL_SURFACE('',#10508,0.1954);
#9134=CYLINDRICAL_SURFACE('',#10509,0.1954);
#9135=CYLINDRICAL_SURFACE('',#10510,0.1954);
#9136=CYLINDRICAL_SURFACE('',#10511,0.1954);
#9137=CYLINDRICAL_SURFACE('',#10512,0.1954);
#9138=CYLINDRICAL_SURFACE('',#10513,0.1954);
#9139=CYLINDRICAL_SURFACE('',#10514,0.1954);
#9140=CYLINDRICAL_SURFACE('',#10515,0.1954);
#9141=CYLINDRICAL_SURFACE('',#10516,0.1954);
#9142=CYLINDRICAL_SURFACE('',#10517,0.1954);
#9143=CYLINDRICAL_SURFACE('',#10518,0.1954);
#9144=CYLINDRICAL_SURFACE('',#10519,0.1954);
#9145=CYLINDRICAL_SURFACE('',#10520,0.1954);
#9146=CYLINDRICAL_SURFACE('',#10521,0.1954);
#9147=CYLINDRICAL_SURFACE('',#10522,0.1954);
#9148=CYLINDRICAL_SURFACE('',#10523,0.15555);
#9149=CYLINDRICAL_SURFACE('',#10525,0.15555);
#9150=CYLINDRICAL_SURFACE('',#10526,0.15555);
#9151=CYLINDRICAL_SURFACE('',#10527,0.15555);
#9152=CYLINDRICAL_SURFACE('',#10528,0.15555);
#9153=CYLINDRICAL_SURFACE('',#10529,0.15555);
#9154=CYLINDRICAL_SURFACE('',#10530,0.15555);
#9155=CYLINDRICAL_SURFACE('',#10531,0.15555);
#9156=CYLINDRICAL_SURFACE('',#10532,0.15555);
#9157=CYLINDRICAL_SURFACE('',#10533,0.15555);
#9158=CYLINDRICAL_SURFACE('',#10534,0.15555);
#9159=CYLINDRICAL_SURFACE('',#10535,0.15555);
#9160=CYLINDRICAL_SURFACE('',#10536,0.15555);
#9161=CYLINDRICAL_SURFACE('',#10537,0.15555);
#9162=CYLINDRICAL_SURFACE('',#10538,0.15555);
#9163=CYLINDRICAL_SURFACE('',#10539,0.15555);
#9164=CYLINDRICAL_SURFACE('',#10543,0.15555);
#9165=CYLINDRICAL_SURFACE('',#10545,0.1954);
#9166=CYLINDRICAL_SURFACE('',#10555,0.35);
#9167=CYLINDRICAL_SURFACE('',#10560,0.14635);
#9168=CYLINDRICAL_SURFACE('',#10562,0.14635);
#9169=CYLINDRICAL_SURFACE('',#10563,0.14635);
#9170=CYLINDRICAL_SURFACE('',#10564,0.14635);
#9171=CYLINDRICAL_SURFACE('',#10565,0.14635);
#9172=CYLINDRICAL_SURFACE('',#10566,0.14635);
#9173=CYLINDRICAL_SURFACE('',#10567,0.14635);
#9174=CYLINDRICAL_SURFACE('',#10568,0.14635);
#9175=CYLINDRICAL_SURFACE('',#10569,0.14635);
#9176=CYLINDRICAL_SURFACE('',#10570,0.14635);
#9177=CYLINDRICAL_SURFACE('',#10571,0.117775);
#9178=CYLINDRICAL_SURFACE('',#10573,0.117775);
#9179=CYLINDRICAL_SURFACE('',#10574,0.117775);
#9180=CYLINDRICAL_SURFACE('',#10575,0.117775);
#9181=CYLINDRICAL_SURFACE('',#10576,0.117775);
#9182=CYLINDRICAL_SURFACE('',#10577,0.117775);
#9183=CYLINDRICAL_SURFACE('',#10578,0.117775);
#9184=CYLINDRICAL_SURFACE('',#10579,0.117775);
#9185=CYLINDRICAL_SURFACE('',#10580,0.117775);
#9186=CYLINDRICAL_SURFACE('',#10581,0.117775);
#9187=CYLINDRICAL_SURFACE('',#10585,0.117775);
#9188=CYLINDRICAL_SURFACE('',#10587,0.14635);
#9189=CYLINDRICAL_SURFACE('',#10597,0.3);
#9190=CYLINDRICAL_SURFACE('',#10602,0.14635);
#9191=CYLINDRICAL_SURFACE('',#10604,0.14635);
#9192=CYLINDRICAL_SURFACE('',#10605,0.14635);
#9193=CYLINDRICAL_SURFACE('',#10606,0.14635);
#9194=CYLINDRICAL_SURFACE('',#10607,0.14635);
#9195=CYLINDRICAL_SURFACE('',#10608,0.14635);
#9196=CYLINDRICAL_SURFACE('',#10609,0.14635);
#9197=CYLINDRICAL_SURFACE('',#10610,0.14635);
#9198=CYLINDRICAL_SURFACE('',#10611,0.14635);
#9199=CYLINDRICAL_SURFACE('',#10612,0.14635);
#9200=CYLINDRICAL_SURFACE('',#10613,0.14635);
#9201=CYLINDRICAL_SURFACE('',#10614,0.14635);
#9202=CYLINDRICAL_SURFACE('',#10615,0.14635);
#9203=CYLINDRICAL_SURFACE('',#10616,0.14635);
#9204=CYLINDRICAL_SURFACE('',#10617,0.14635);
#9205=CYLINDRICAL_SURFACE('',#10618,0.14635);
#9206=CYLINDRICAL_SURFACE('',#10619,0.14635);
#9207=CYLINDRICAL_SURFACE('',#10620,0.14635);
#9208=CYLINDRICAL_SURFACE('',#10621,0.117775);
#9209=CYLINDRICAL_SURFACE('',#10623,0.117775);
#9210=CYLINDRICAL_SURFACE('',#10624,0.117775);
#9211=CYLINDRICAL_SURFACE('',#10625,0.117775);
#9212=CYLINDRICAL_SURFACE('',#10626,0.117775);
#9213=CYLINDRICAL_SURFACE('',#10627,0.117775);
#9214=CYLINDRICAL_SURFACE('',#10628,0.117775);
#9215=CYLINDRICAL_SURFACE('',#10629,0.117775);
#9216=CYLINDRICAL_SURFACE('',#10630,0.117775);
#9217=CYLINDRICAL_SURFACE('',#10631,0.117775);
#9218=CYLINDRICAL_SURFACE('',#10632,0.117775);
#9219=CYLINDRICAL_SURFACE('',#10633,0.117775);
#9220=CYLINDRICAL_SURFACE('',#10634,0.117775);
#9221=CYLINDRICAL_SURFACE('',#10635,0.117775);
#9222=CYLINDRICAL_SURFACE('',#10636,0.117775);
#9223=CYLINDRICAL_SURFACE('',#10637,0.117775);
#9224=CYLINDRICAL_SURFACE('',#10638,0.117775);
#9225=CYLINDRICAL_SURFACE('',#10639,0.117775);
#9226=CYLINDRICAL_SURFACE('',#10643,0.117775);
#9227=CYLINDRICAL_SURFACE('',#10645,0.14635);
#9228=CYLINDRICAL_SURFACE('',#10655,0.3);
#9229=ADVANCED_FACE('',(#439),#8860,.F.);
#9230=ADVANCED_FACE('',(#440),#8861,.F.);
#9231=ADVANCED_FACE('',(#441),#8862,.F.);
#9232=ADVANCED_FACE('',(#442),#8863,.F.);
#9233=ADVANCED_FACE('',(#443),#8864,.F.);
#9234=ADVANCED_FACE('',(#444),#8865,.F.);
#9235=ADVANCED_FACE('',(#445),#8866,.F.);
#9236=ADVANCED_FACE('',(#446),#8867,.F.);
#9237=ADVANCED_FACE('',(#447),#8868,.F.);
#9238=ADVANCED_FACE('',(#448),#8869,.F.);
#9239=ADVANCED_FACE('',(#449),#8870,.F.);
#9240=ADVANCED_FACE('',(#450),#8871,.F.);
#9241=ADVANCED_FACE('',(#451),#8872,.F.);
#9242=ADVANCED_FACE('',(#452),#8873,.F.);
#9243=ADVANCED_FACE('',(#453),#8874,.F.);
#9244=ADVANCED_FACE('',(#454),#8875,.F.);
#9245=ADVANCED_FACE('',(#455),#8876,.F.);
#9246=ADVANCED_FACE('',(#456),#8877,.F.);
#9247=ADVANCED_FACE('',(#457),#8878,.F.);
#9248=ADVANCED_FACE('',(#458),#8879,.F.);
#9249=ADVANCED_FACE('',(#459),#8880,.F.);
#9250=ADVANCED_FACE('',(#460),#8881,.F.);
#9251=ADVANCED_FACE('',(#461),#8882,.F.);
#9252=ADVANCED_FACE('',(#462),#8883,.F.);
#9253=ADVANCED_FACE('',(#463),#8884,.F.);
#9254=ADVANCED_FACE('',(#464),#8885,.F.);
#9255=ADVANCED_FACE('',(#465),#8886,.F.);
#9256=ADVANCED_FACE('',(#466),#8887,.F.);
#9257=ADVANCED_FACE('',(#467),#8888,.F.);
#9258=ADVANCED_FACE('',(#468),#8889,.F.);
#9259=ADVANCED_FACE('',(#469),#8890,.F.);
#9260=ADVANCED_FACE('',(#470),#8891,.F.);
#9261=ADVANCED_FACE('',(#471),#8892,.F.);
#9262=ADVANCED_FACE('',(#472),#8893,.F.);
#9263=ADVANCED_FACE('',(#473),#8894,.F.);
#9264=ADVANCED_FACE('',(#474),#8895,.F.);
#9265=ADVANCED_FACE('',(#475),#8896,.F.);
#9266=ADVANCED_FACE('',(#476),#8897,.F.);
#9267=ADVANCED_FACE('',(#477),#8898,.F.);
#9268=ADVANCED_FACE('',(#478),#8899,.F.);
#9269=ADVANCED_FACE('',(#479),#8900,.F.);
#9270=ADVANCED_FACE('',(#480),#8901,.F.);
#9271=ADVANCED_FACE('',(#481),#8902,.F.);
#9272=ADVANCED_FACE('',(#482),#8903,.F.);
#9273=ADVANCED_FACE('',(#483),#8904,.F.);
#9274=ADVANCED_FACE('',(#484),#8905,.F.);
#9275=ADVANCED_FACE('',(#485),#8906,.F.);
#9276=ADVANCED_FACE('',(#486),#8907,.F.);
#9277=ADVANCED_FACE('',(#487),#8908,.F.);
#9278=ADVANCED_FACE('',(#488),#8909,.F.);
#9279=ADVANCED_FACE('',(#489),#8910,.F.);
#9280=ADVANCED_FACE('',(#490),#8911,.F.);
#9281=ADVANCED_FACE('',(#491),#8912,.F.);
#9282=ADVANCED_FACE('',(#492),#8913,.F.);
#9283=ADVANCED_FACE('',(#493),#8914,.F.);
#9284=ADVANCED_FACE('',(#494),#8915,.F.);
#9285=ADVANCED_FACE('',(#495),#8916,.F.);
#9286=ADVANCED_FACE('',(#496),#8917,.F.);
#9287=ADVANCED_FACE('',(#497),#8918,.F.);
#9288=ADVANCED_FACE('',(#498),#8919,.F.);
#9289=ADVANCED_FACE('',(#499),#8920,.F.);
#9290=ADVANCED_FACE('',(#500),#8921,.F.);
#9291=ADVANCED_FACE('',(#501),#8922,.F.);
#9292=ADVANCED_FACE('',(#502),#8923,.F.);
#9293=ADVANCED_FACE('',(#503),#8924,.F.);
#9294=ADVANCED_FACE('',(#504),#8925,.F.);
#9295=ADVANCED_FACE('',(#505),#8926,.F.);
#9296=ADVANCED_FACE('',(#506),#8927,.F.);
#9297=ADVANCED_FACE('',(#507),#8928,.F.);
#9298=ADVANCED_FACE('',(#508),#8929,.F.);
#9299=ADVANCED_FACE('',(#509),#8930,.F.);
#9300=ADVANCED_FACE('',(#510),#8931,.F.);
#9301=ADVANCED_FACE('',(#511),#8932,.F.);
#9302=ADVANCED_FACE('',(#512),#8933,.F.);
#9303=ADVANCED_FACE('',(#513),#8934,.F.);
#9304=ADVANCED_FACE('',(#514),#8935,.F.);
#9305=ADVANCED_FACE('',(#515),#8936,.F.);
#9306=ADVANCED_FACE('',(#516),#8937,.F.);
#9307=ADVANCED_FACE('',(#517),#8938,.F.);
#9308=ADVANCED_FACE('',(#518),#8939,.F.);
#9309=ADVANCED_FACE('',(#519),#8940,.F.);
#9310=ADVANCED_FACE('',(#520),#8941,.F.);
#9311=ADVANCED_FACE('',(#521),#8942,.F.);
#9312=ADVANCED_FACE('',(#522),#8943,.F.);
#9313=ADVANCED_FACE('',(#523),#8944,.F.);
#9314=ADVANCED_FACE('',(#524),#8945,.F.);
#9315=ADVANCED_FACE('',(#525),#8946,.F.);
#9316=ADVANCED_FACE('',(#526),#8947,.F.);
#9317=ADVANCED_FACE('',(#527),#8948,.F.);
#9318=ADVANCED_FACE('',(#528),#8949,.F.);
#9319=ADVANCED_FACE('',(#529),#8950,.F.);
#9320=ADVANCED_FACE('',(#530),#8951,.F.);
#9321=ADVANCED_FACE('',(#531),#8952,.F.);
#9322=ADVANCED_FACE('',(#532),#8953,.F.);
#9323=ADVANCED_FACE('',(#533),#8954,.F.);
#9324=ADVANCED_FACE('',(#534),#8955,.F.);
#9325=ADVANCED_FACE('',(#535),#8956,.F.);
#9326=ADVANCED_FACE('',(#536),#8957,.F.);
#9327=ADVANCED_FACE('',(#537),#8958,.F.);
#9328=ADVANCED_FACE('',(#538),#8959,.F.);
#9329=ADVANCED_FACE('',(#539),#8960,.F.);
#9330=ADVANCED_FACE('',(#540),#302,.F.);
#9331=ADVANCED_FACE('',(#541),#8961,.F.);
#9332=ADVANCED_FACE('',(#542),#303,.F.);
#9333=ADVANCED_FACE('',(#543),#8962,.F.);
#9334=ADVANCED_FACE('',(#544,#235,#236,#237),#304,.F.);
#9335=ADVANCED_FACE('',(#545,#238),#305,.F.);
#9336=ADVANCED_FACE('',(#546),#8963,.F.);
#9337=ADVANCED_FACE('',(#547),#8964,.F.);
#9338=ADVANCED_FACE('',(#548,#239),#306,.F.);
#9339=ADVANCED_FACE('',(#549),#8965,.F.);
#9340=ADVANCED_FACE('',(#550),#8966,.F.);
#9341=ADVANCED_FACE('',(#551,#240),#307,.F.);
#9342=ADVANCED_FACE('',(#552),#8967,.F.);
#9343=ADVANCED_FACE('',(#553),#8968,.F.);
#9344=ADVANCED_FACE('',(#554),#308,.T.);
#9345=ADVANCED_FACE('',(#555),#8969,.F.);
#9346=ADVANCED_FACE('',(#556),#210,.F.);
#9347=ADVANCED_FACE('',(#557),#211,.F.);
#9348=ADVANCED_FACE('',(#558),#8970,.F.);
#9349=ADVANCED_FACE('',(#559),#309,.T.);
#9350=ADVANCED_FACE('',(#560),#8971,.F.);
#9351=ADVANCED_FACE('',(#561),#212,.F.);
#9352=ADVANCED_FACE('',(#562),#213,.F.);
#9353=ADVANCED_FACE('',(#563),#8972,.F.);
#9354=ADVANCED_FACE('',(#564),#310,.T.);
#9355=ADVANCED_FACE('',(#565),#8973,.F.);
#9356=ADVANCED_FACE('',(#566),#214,.F.);
#9357=ADVANCED_FACE('',(#567),#215,.F.);
#9358=ADVANCED_FACE('',(#568),#8974,.F.);
#9359=ADVANCED_FACE('',(#569),#311,.T.);
#9360=ADVANCED_FACE('',(#570),#8975,.F.);
#9361=ADVANCED_FACE('',(#571),#216,.F.);
#9362=ADVANCED_FACE('',(#572),#217,.F.);
#9363=ADVANCED_FACE('',(#573),#8976,.F.);
#9364=ADVANCED_FACE('',(#574),#312,.F.);
#9365=ADVANCED_FACE('',(#575),#313,.F.);
#9366=ADVANCED_FACE('',(#576),#314,.F.);
#9367=ADVANCED_FACE('',(#577),#315,.F.);
#9368=ADVANCED_FACE('',(#578),#8977,.F.);
#9369=ADVANCED_FACE('',(#579),#8978,.F.);
#9370=ADVANCED_FACE('',(#580),#316,.T.);
#9371=ADVANCED_FACE('',(#581),#317,.T.);
#9372=ADVANCED_FACE('',(#582),#318,.T.);
#9373=ADVANCED_FACE('',(#583,#241),#319,.T.);
#9374=ADVANCED_FACE('',(#584),#320,.T.);
#9375=ADVANCED_FACE('',(#585),#321,.T.);
#9376=ADVANCED_FACE('',(#586),#322,.T.);
#9377=ADVANCED_FACE('',(#587,#242),#323,.T.);
#9378=ADVANCED_FACE('',(#588),#8979,.F.);
#9379=ADVANCED_FACE('',(#589),#8980,.T.);
#9380=ADVANCED_FACE('',(#590,#243),#324,.T.);
#9381=ADVANCED_FACE('',(#591),#325,.F.);
#9382=ADVANCED_FACE('',(#592),#326,.F.);
#9383=ADVANCED_FACE('',(#593),#327,.T.);
#9384=ADVANCED_FACE('',(#594),#328,.T.);
#9385=ADVANCED_FACE('',(#595,#244),#329,.T.);
#9386=ADVANCED_FACE('',(#596),#330,.T.);
#9387=ADVANCED_FACE('',(#597,#245,#246,#247,#248,#249),#331,.T.);
#9388=ADVANCED_FACE('',(#598,#250,#251,#252,#253),#332,.F.);
#9389=ADVANCED_FACE('',(#599),#8981,.F.);
#9390=ADVANCED_FACE('',(#600),#8982,.F.);
#9391=ADVANCED_FACE('',(#601),#8983,.F.);
#9392=ADVANCED_FACE('',(#602),#8984,.F.);
#9393=ADVANCED_FACE('',(#603),#8985,.F.);
#9394=ADVANCED_FACE('',(#604),#333,.T.);
#9395=ADVANCED_FACE('',(#605),#334,.T.);
#9396=ADVANCED_FACE('',(#606),#335,.T.);
#9397=ADVANCED_FACE('',(#607),#336,.T.);
#9398=ADVANCED_FACE('',(#608,#254,#255,#256,#257,#258),#337,.T.);
#9399=ADVANCED_FACE('',(#609,#259,#260,#261,#262,#263),#338,.F.);
#9400=ADVANCED_FACE('',(#610,#264),#339,.T.);
#9401=ADVANCED_FACE('',(#611),#8986,.T.);
#9402=ADVANCED_FACE('',(#612,#265),#340,.F.);
#9403=ADVANCED_FACE('',(#613),#8987,.F.);
#9404=ADVANCED_FACE('',(#614),#8988,.T.);
#9405=ADVANCED_FACE('',(#615,#266),#341,.T.);
#9406=ADVANCED_FACE('',(#616),#8989,.F.);
#9407=ADVANCED_FACE('',(#617),#8990,.F.);
#9408=ADVANCED_FACE('',(#618),#8991,.F.);
#9409=ADVANCED_FACE('',(#619),#8992,.F.);
#9410=ADVANCED_FACE('',(#620),#8993,.F.);
#9411=ADVANCED_FACE('',(#621),#8994,.F.);
#9412=ADVANCED_FACE('',(#622),#8995,.F.);
#9413=ADVANCED_FACE('',(#623),#8996,.F.);
#9414=ADVANCED_FACE('',(#624),#8997,.F.);
#9415=ADVANCED_FACE('',(#625),#8998,.F.);
#9416=ADVANCED_FACE('',(#626),#8999,.F.);
#9417=ADVANCED_FACE('',(#627),#9000,.F.);
#9418=ADVANCED_FACE('',(#628),#9001,.F.);
#9419=ADVANCED_FACE('',(#629),#9002,.F.);
#9420=ADVANCED_FACE('',(#630),#9003,.F.);
#9421=ADVANCED_FACE('',(#631),#9004,.F.);
#9422=ADVANCED_FACE('',(#632),#9005,.F.);
#9423=ADVANCED_FACE('',(#633),#9006,.F.);
#9424=ADVANCED_FACE('',(#634),#9007,.F.);
#9425=ADVANCED_FACE('',(#635),#9008,.F.);
#9426=ADVANCED_FACE('',(#636),#9009,.F.);
#9427=ADVANCED_FACE('',(#637),#9010,.F.);
#9428=ADVANCED_FACE('',(#638),#9011,.F.);
#9429=ADVANCED_FACE('',(#639),#9012,.F.);
#9430=ADVANCED_FACE('',(#640),#9013,.F.);
#9431=ADVANCED_FACE('',(#641),#9014,.F.);
#9432=ADVANCED_FACE('',(#642),#9015,.F.);
#9433=ADVANCED_FACE('',(#643),#9016,.F.);
#9434=ADVANCED_FACE('',(#644),#9017,.F.);
#9435=ADVANCED_FACE('',(#645),#9018,.F.);
#9436=ADVANCED_FACE('',(#646),#9019,.F.);
#9437=ADVANCED_FACE('',(#647),#9020,.F.);
#9438=ADVANCED_FACE('',(#648),#9021,.F.);
#9439=ADVANCED_FACE('',(#649),#218,.F.);
#9440=ADVANCED_FACE('',(#650),#219,.F.);
#9441=ADVANCED_FACE('',(#651,#267,#268),#342,.F.);
#9442=ADVANCED_FACE('',(#652),#9022,.F.);
#9443=ADVANCED_FACE('',(#653),#220,.F.);
#9444=ADVANCED_FACE('',(#654),#221,.F.);
#9445=ADVANCED_FACE('',(#655),#9023,.F.);
#9446=ADVANCED_FACE('',(#656),#9024,.F.);
#9447=ADVANCED_FACE('',(#657),#9025,.F.);
#9448=ADVANCED_FACE('',(#658),#9026,.F.);
#9449=ADVANCED_FACE('',(#659,#269),#343,.T.);
#9450=ADVANCED_FACE('',(#660),#344,.T.);
#9451=ADVANCED_FACE('',(#661),#345,.T.);
#9452=ADVANCED_FACE('',(#662),#346,.T.);
#9453=ADVANCED_FACE('',(#663,#270),#347,.T.);
#9454=ADVANCED_FACE('',(#664),#348,.T.);
#9455=ADVANCED_FACE('',(#665),#349,.F.);
#9456=ADVANCED_FACE('',(#666),#350,.F.);
#9457=ADVANCED_FACE('',(#667),#351,.T.);
#9458=ADVANCED_FACE('',(#668,#271),#352,.T.);
#9459=ADVANCED_FACE('',(#669,#272),#353,.T.);
#9460=ADVANCED_FACE('',(#670),#354,.T.);
#9461=ADVANCED_FACE('',(#671),#355,.T.);
#9462=ADVANCED_FACE('',(#672),#356,.T.);
#9463=ADVANCED_FACE('',(#673),#357,.T.);
#9464=ADVANCED_FACE('',(#674),#358,.T.);
#9465=ADVANCED_FACE('',(#675),#9027,.T.);
#9466=ADVANCED_FACE('',(#676),#9028,.T.);
#9467=ADVANCED_FACE('',(#677,#273,#274,#275),#359,.T.);
#9468=ADVANCED_FACE('',(#678),#9029,.F.);
#9469=ADVANCED_FACE('',(#679),#9030,.F.);
#9470=ADVANCED_FACE('',(#680),#360,.T.);
#9471=ADVANCED_FACE('',(#681),#361,.T.);
#9472=ADVANCED_FACE('',(#682),#362,.T.);
#9473=ADVANCED_FACE('',(#683),#363,.T.);
#9474=ADVANCED_FACE('',(#684,#276,#277),#364,.T.);
#9475=ADVANCED_FACE('',(#685,#278,#279),#365,.F.);
#9476=ADVANCED_FACE('',(#686),#135,.T.);
#9477=ADVANCED_FACE('',(#687),#9031,.T.);
#9478=ADVANCED_FACE('',(#688,#280),#366,.F.);
#9479=ADVANCED_FACE('',(#689),#136,.T.);
#9480=ADVANCED_FACE('',(#690,#281),#367,.T.);
#9481=ADVANCED_FACE('',(#691),#137,.F.);
#9482=ADVANCED_FACE('',(#692),#9032,.F.);
#9483=ADVANCED_FACE('',(#693),#138,.F.);
#9484=ADVANCED_FACE('',(#694),#9033,.F.);
#9485=ADVANCED_FACE('',(#695),#9034,.F.);
#9486=ADVANCED_FACE('',(#696),#9035,.F.);
#9487=ADVANCED_FACE('',(#697),#9036,.F.);
#9488=ADVANCED_FACE('',(#698),#9037,.F.);
#9489=ADVANCED_FACE('',(#699),#9038,.F.);
#9490=ADVANCED_FACE('',(#700),#9039,.F.);
#9491=ADVANCED_FACE('',(#701),#9040,.F.);
#9492=ADVANCED_FACE('',(#702),#9041,.F.);
#9493=ADVANCED_FACE('',(#703),#9042,.F.);
#9494=ADVANCED_FACE('',(#704),#9043,.F.);
#9495=ADVANCED_FACE('',(#705),#9044,.F.);
#9496=ADVANCED_FACE('',(#706),#9045,.F.);
#9497=ADVANCED_FACE('',(#707),#9046,.F.);
#9498=ADVANCED_FACE('',(#708),#9047,.F.);
#9499=ADVANCED_FACE('',(#709),#9048,.F.);
#9500=ADVANCED_FACE('',(#710),#9049,.F.);
#9501=ADVANCED_FACE('',(#711),#9050,.F.);
#9502=ADVANCED_FACE('',(#712),#9051,.F.);
#9503=ADVANCED_FACE('',(#713),#9052,.F.);
#9504=ADVANCED_FACE('',(#714),#9053,.F.);
#9505=ADVANCED_FACE('',(#715),#9054,.F.);
#9506=ADVANCED_FACE('',(#716),#9055,.F.);
#9507=ADVANCED_FACE('',(#717),#9056,.F.);
#9508=ADVANCED_FACE('',(#718),#9057,.F.);
#9509=ADVANCED_FACE('',(#719),#9058,.F.);
#9510=ADVANCED_FACE('',(#720),#9059,.F.);
#9511=ADVANCED_FACE('',(#721),#9060,.F.);
#9512=ADVANCED_FACE('',(#722),#9061,.F.);
#9513=ADVANCED_FACE('',(#723),#9062,.F.);
#9514=ADVANCED_FACE('',(#724),#9063,.F.);
#9515=ADVANCED_FACE('',(#725),#9064,.F.);
#9516=ADVANCED_FACE('',(#726),#9065,.F.);
#9517=ADVANCED_FACE('',(#727),#9066,.F.);
#9518=ADVANCED_FACE('',(#728),#9067,.F.);
#9519=ADVANCED_FACE('',(#729),#9068,.F.);
#9520=ADVANCED_FACE('',(#730),#9069,.F.);
#9521=ADVANCED_FACE('',(#731),#9070,.F.);
#9522=ADVANCED_FACE('',(#732),#9071,.F.);
#9523=ADVANCED_FACE('',(#733),#9072,.F.);
#9524=ADVANCED_FACE('',(#734),#9073,.F.);
#9525=ADVANCED_FACE('',(#735),#9074,.F.);
#9526=ADVANCED_FACE('',(#736),#9075,.F.);
#9527=ADVANCED_FACE('',(#737),#9076,.F.);
#9528=ADVANCED_FACE('',(#738),#9077,.F.);
#9529=ADVANCED_FACE('',(#739),#9078,.F.);
#9530=ADVANCED_FACE('',(#740),#9079,.F.);
#9531=ADVANCED_FACE('',(#741),#9080,.F.);
#9532=ADVANCED_FACE('',(#742),#9081,.F.);
#9533=ADVANCED_FACE('',(#743),#9082,.F.);
#9534=ADVANCED_FACE('',(#744),#9083,.F.);
#9535=ADVANCED_FACE('',(#745),#9084,.F.);
#9536=ADVANCED_FACE('',(#746),#9085,.F.);
#9537=ADVANCED_FACE('',(#747),#9086,.F.);
#9538=ADVANCED_FACE('',(#748),#9087,.F.);
#9539=ADVANCED_FACE('',(#749),#9088,.F.);
#9540=ADVANCED_FACE('',(#750),#9089,.F.);
#9541=ADVANCED_FACE('',(#751),#9090,.F.);
#9542=ADVANCED_FACE('',(#752),#9091,.F.);
#9543=ADVANCED_FACE('',(#753),#9092,.F.);
#9544=ADVANCED_FACE('',(#754),#9093,.F.);
#9545=ADVANCED_FACE('',(#755),#368,.T.);
#9546=ADVANCED_FACE('',(#756),#9094,.F.);
#9547=ADVANCED_FACE('',(#757),#222,.F.);
#9548=ADVANCED_FACE('',(#758),#223,.F.);
#9549=ADVANCED_FACE('',(#759),#9095,.F.);
#9550=ADVANCED_FACE('',(#760),#369,.F.);
#9551=ADVANCED_FACE('',(#761),#370,.F.);
#9552=ADVANCED_FACE('',(#762),#9096,.F.);
#9553=ADVANCED_FACE('',(#763),#224,.F.);
#9554=ADVANCED_FACE('',(#764),#225,.F.);
#9555=ADVANCED_FACE('',(#765),#9097,.F.);
#9556=ADVANCED_FACE('',(#766),#371,.F.);
#9557=ADVANCED_FACE('',(#767),#372,.T.);
#9558=ADVANCED_FACE('',(#768),#373,.T.);
#9559=ADVANCED_FACE('',(#769),#374,.T.);
#9560=ADVANCED_FACE('',(#770),#375,.T.);
#9561=ADVANCED_FACE('',(#771,#282),#376,.T.);
#9562=ADVANCED_FACE('',(#772,#283),#377,.F.);
#9563=ADVANCED_FACE('',(#773),#9098,.F.);
#9564=ADVANCED_FACE('',(#774),#9099,.F.);
#9565=ADVANCED_FACE('',(#775),#9100,.F.);
#9566=ADVANCED_FACE('',(#776),#9101,.F.);
#9567=ADVANCED_FACE('',(#777),#9102,.F.);
#9568=ADVANCED_FACE('',(#778),#9103,.F.);
#9569=ADVANCED_FACE('',(#779),#9104,.F.);
#9570=ADVANCED_FACE('',(#780),#9105,.F.);
#9571=ADVANCED_FACE('',(#781),#9106,.F.);
#9572=ADVANCED_FACE('',(#782),#9107,.F.);
#9573=ADVANCED_FACE('',(#783),#9108,.F.);
#9574=ADVANCED_FACE('',(#784),#9109,.F.);
#9575=ADVANCED_FACE('',(#785),#9110,.F.);
#9576=ADVANCED_FACE('',(#786),#9111,.F.);
#9577=ADVANCED_FACE('',(#787),#9112,.F.);
#9578=ADVANCED_FACE('',(#788),#9113,.F.);
#9579=ADVANCED_FACE('',(#789),#9114,.F.);
#9580=ADVANCED_FACE('',(#790),#9115,.F.);
#9581=ADVANCED_FACE('',(#791),#9116,.F.);
#9582=ADVANCED_FACE('',(#792),#9117,.F.);
#9583=ADVANCED_FACE('',(#793),#378,.T.);
#9584=ADVANCED_FACE('',(#794),#9118,.F.);
#9585=ADVANCED_FACE('',(#795),#226,.F.);
#9586=ADVANCED_FACE('',(#796),#227,.F.);
#9587=ADVANCED_FACE('',(#797),#9119,.F.);
#9588=ADVANCED_FACE('',(#798),#379,.F.);
#9589=ADVANCED_FACE('',(#799),#9120,.F.);
#9590=ADVANCED_FACE('',(#800),#380,.T.);
#9591=ADVANCED_FACE('',(#801,#284),#381,.F.);
#9592=ADVANCED_FACE('',(#802),#382,.T.);
#9593=ADVANCED_FACE('',(#803),#383,.T.);
#9594=ADVANCED_FACE('',(#804),#384,.T.);
#9595=ADVANCED_FACE('',(#805),#385,.T.);
#9596=ADVANCED_FACE('',(#806,#285,#286),#386,.T.);
#9597=ADVANCED_FACE('',(#807),#387,.F.);
#9598=ADVANCED_FACE('',(#808),#9121,.F.);
#9599=ADVANCED_FACE('',(#809),#388,.T.);
#9600=ADVANCED_FACE('',(#810),#389,.T.);
#9601=ADVANCED_FACE('',(#811),#390,.T.);
#9602=ADVANCED_FACE('',(#812),#391,.T.);
#9603=ADVANCED_FACE('',(#813,#287),#392,.T.);
#9604=ADVANCED_FACE('',(#814,#288),#393,.F.);
#9605=ADVANCED_FACE('',(#815),#9122,.F.);
#9606=ADVANCED_FACE('',(#816),#9123,.T.);
#9607=ADVANCED_FACE('',(#817,#289),#394,.T.);
#9608=ADVANCED_FACE('',(#818,#290),#395,.F.);
#9609=ADVANCED_FACE('',(#819),#9124,.T.);
#9610=ADVANCED_FACE('',(#820,#291),#396,.F.);
#9611=ADVANCED_FACE('',(#821,#292),#397,.F.);
#9612=ADVANCED_FACE('',(#822),#9125,.T.);
#9613=ADVANCED_FACE('',(#823,#293),#398,.T.);
#9614=ADVANCED_FACE('',(#824),#9126,.T.);
#9615=ADVANCED_FACE('',(#825),#399,.F.);
#9616=ADVANCED_FACE('',(#826),#9127,.T.);
#9617=ADVANCED_FACE('',(#827),#400,.T.);
#9618=ADVANCED_FACE('',(#828),#401,.F.);
#9619=ADVANCED_FACE('',(#829),#402,.F.);
#9620=ADVANCED_FACE('',(#830),#403,.F.);
#9621=ADVANCED_FACE('',(#831),#9128,.F.);
#9622=ADVANCED_FACE('',(#832),#9129,.T.);
#9623=ADVANCED_FACE('',(#833),#404,.T.);
#9624=ADVANCED_FACE('',(#834),#228,.T.);
#9625=ADVANCED_FACE('',(#835),#405,.F.);
#9626=ADVANCED_FACE('',(#836),#406,.T.);
#9627=ADVANCED_FACE('',(#837),#9130,.F.);
#9628=ADVANCED_FACE('',(#838),#9131,.T.);
#9629=ADVANCED_FACE('',(#839,#294),#407,.T.);
#9630=ADVANCED_FACE('',(#840,#295),#408,.F.);
#9631=ADVANCED_FACE('',(#841),#9132,.T.);
#9632=ADVANCED_FACE('',(#842),#9133,.T.);
#9633=ADVANCED_FACE('',(#843),#9134,.T.);
#9634=ADVANCED_FACE('',(#844),#9135,.T.);
#9635=ADVANCED_FACE('',(#845),#9136,.T.);
#9636=ADVANCED_FACE('',(#846),#9137,.T.);
#9637=ADVANCED_FACE('',(#847),#9138,.T.);
#9638=ADVANCED_FACE('',(#848),#9139,.T.);
#9639=ADVANCED_FACE('',(#849),#9140,.T.);
#9640=ADVANCED_FACE('',(#850),#9141,.T.);
#9641=ADVANCED_FACE('',(#851),#9142,.T.);
#9642=ADVANCED_FACE('',(#852),#9143,.T.);
#9643=ADVANCED_FACE('',(#853),#9144,.T.);
#9644=ADVANCED_FACE('',(#854),#9145,.T.);
#9645=ADVANCED_FACE('',(#855),#9146,.T.);
#9646=ADVANCED_FACE('',(#856),#9147,.T.);
#9647=ADVANCED_FACE('',(#857),#9148,.T.);
#9648=ADVANCED_FACE('',(#858),#9149,.T.);
#9649=ADVANCED_FACE('',(#859),#9150,.T.);
#9650=ADVANCED_FACE('',(#860),#9151,.T.);
#9651=ADVANCED_FACE('',(#861),#9152,.T.);
#9652=ADVANCED_FACE('',(#862),#9153,.T.);
#9653=ADVANCED_FACE('',(#863),#9154,.T.);
#9654=ADVANCED_FACE('',(#864),#9155,.T.);
#9655=ADVANCED_FACE('',(#865),#9156,.T.);
#9656=ADVANCED_FACE('',(#866),#9157,.T.);
#9657=ADVANCED_FACE('',(#867),#9158,.T.);
#9658=ADVANCED_FACE('',(#868),#9159,.T.);
#9659=ADVANCED_FACE('',(#869),#9160,.T.);
#9660=ADVANCED_FACE('',(#870),#9161,.T.);
#9661=ADVANCED_FACE('',(#871),#9162,.T.);
#9662=ADVANCED_FACE('',(#872),#9163,.T.);
#9663=ADVANCED_FACE('',(#873),#139,.T.);
#9664=ADVANCED_FACE('',(#874),#229,.F.);
#9665=ADVANCED_FACE('',(#875),#9164,.T.);
#9666=ADVANCED_FACE('',(#876),#230,.F.);
#9667=ADVANCED_FACE('',(#877),#9165,.T.);
#9668=ADVANCED_FACE('',(#878),#409,.F.);
#9669=ADVANCED_FACE('',(#879),#410,.F.);
#9670=ADVANCED_FACE('',(#880),#411,.F.);
#9671=ADVANCED_FACE('',(#881),#412,.F.);
#9672=ADVANCED_FACE('',(#882),#413,.F.);
#9673=ADVANCED_FACE('',(#883),#414,.F.);
#9674=ADVANCED_FACE('',(#884),#415,.F.);
#9675=ADVANCED_FACE('',(#885,#296),#416,.T.);
#9676=ADVANCED_FACE('',(#886),#9166,.T.);
#9677=ADVANCED_FACE('',(#887,#297),#417,.F.);
#9678=ADVANCED_FACE('',(#888),#418,.T.);
#9679=ADVANCED_FACE('',(#889),#9167,.T.);
#9680=ADVANCED_FACE('',(#890),#9168,.T.);
#9681=ADVANCED_FACE('',(#891),#9169,.T.);
#9682=ADVANCED_FACE('',(#892),#9170,.T.);
#9683=ADVANCED_FACE('',(#893),#9171,.T.);
#9684=ADVANCED_FACE('',(#894),#9172,.T.);
#9685=ADVANCED_FACE('',(#895),#9173,.T.);
#9686=ADVANCED_FACE('',(#896),#9174,.T.);
#9687=ADVANCED_FACE('',(#897),#9175,.T.);
#9688=ADVANCED_FACE('',(#898),#9176,.T.);
#9689=ADVANCED_FACE('',(#899),#9177,.T.);
#9690=ADVANCED_FACE('',(#900),#9178,.T.);
#9691=ADVANCED_FACE('',(#901),#9179,.T.);
#9692=ADVANCED_FACE('',(#902),#9180,.T.);
#9693=ADVANCED_FACE('',(#903),#9181,.T.);
#9694=ADVANCED_FACE('',(#904),#9182,.T.);
#9695=ADVANCED_FACE('',(#905),#9183,.T.);
#9696=ADVANCED_FACE('',(#906),#9184,.T.);
#9697=ADVANCED_FACE('',(#907),#9185,.T.);
#9698=ADVANCED_FACE('',(#908),#9186,.T.);
#9699=ADVANCED_FACE('',(#909),#140,.T.);
#9700=ADVANCED_FACE('',(#910),#231,.F.);
#9701=ADVANCED_FACE('',(#911),#9187,.T.);
#9702=ADVANCED_FACE('',(#912),#232,.F.);
#9703=ADVANCED_FACE('',(#913),#9188,.T.);
#9704=ADVANCED_FACE('',(#914),#419,.F.);
#9705=ADVANCED_FACE('',(#915),#420,.F.);
#9706=ADVANCED_FACE('',(#916),#421,.F.);
#9707=ADVANCED_FACE('',(#917),#422,.F.);
#9708=ADVANCED_FACE('',(#918),#423,.F.);
#9709=ADVANCED_FACE('',(#919),#424,.F.);
#9710=ADVANCED_FACE('',(#920),#425,.F.);
#9711=ADVANCED_FACE('',(#921,#298),#426,.T.);
#9712=ADVANCED_FACE('',(#922),#9189,.T.);
#9713=ADVANCED_FACE('',(#923,#299),#427,.F.);
#9714=ADVANCED_FACE('',(#924),#428,.T.);
#9715=ADVANCED_FACE('',(#925),#9190,.T.);
#9716=ADVANCED_FACE('',(#926),#9191,.T.);
#9717=ADVANCED_FACE('',(#927),#9192,.T.);
#9718=ADVANCED_FACE('',(#928),#9193,.T.);
#9719=ADVANCED_FACE('',(#929),#9194,.T.);
#9720=ADVANCED_FACE('',(#930),#9195,.T.);
#9721=ADVANCED_FACE('',(#931),#9196,.T.);
#9722=ADVANCED_FACE('',(#932),#9197,.T.);
#9723=ADVANCED_FACE('',(#933),#9198,.T.);
#9724=ADVANCED_FACE('',(#934),#9199,.T.);
#9725=ADVANCED_FACE('',(#935),#9200,.T.);
#9726=ADVANCED_FACE('',(#936),#9201,.T.);
#9727=ADVANCED_FACE('',(#937),#9202,.T.);
#9728=ADVANCED_FACE('',(#938),#9203,.T.);
#9729=ADVANCED_FACE('',(#939),#9204,.T.);
#9730=ADVANCED_FACE('',(#940),#9205,.T.);
#9731=ADVANCED_FACE('',(#941),#9206,.T.);
#9732=ADVANCED_FACE('',(#942),#9207,.T.);
#9733=ADVANCED_FACE('',(#943),#9208,.T.);
#9734=ADVANCED_FACE('',(#944),#9209,.T.);
#9735=ADVANCED_FACE('',(#945),#9210,.T.);
#9736=ADVANCED_FACE('',(#946),#9211,.T.);
#9737=ADVANCED_FACE('',(#947),#9212,.T.);
#9738=ADVANCED_FACE('',(#948),#9213,.T.);
#9739=ADVANCED_FACE('',(#949),#9214,.T.);
#9740=ADVANCED_FACE('',(#950),#9215,.T.);
#9741=ADVANCED_FACE('',(#951),#9216,.T.);
#9742=ADVANCED_FACE('',(#952),#9217,.T.);
#9743=ADVANCED_FACE('',(#953),#9218,.T.);
#9744=ADVANCED_FACE('',(#954),#9219,.T.);
#9745=ADVANCED_FACE('',(#955),#9220,.T.);
#9746=ADVANCED_FACE('',(#956),#9221,.T.);
#9747=ADVANCED_FACE('',(#957),#9222,.T.);
#9748=ADVANCED_FACE('',(#958),#9223,.T.);
#9749=ADVANCED_FACE('',(#959),#9224,.T.);
#9750=ADVANCED_FACE('',(#960),#9225,.T.);
#9751=ADVANCED_FACE('',(#961),#141,.T.);
#9752=ADVANCED_FACE('',(#962),#233,.F.);
#9753=ADVANCED_FACE('',(#963),#9226,.T.);
#9754=ADVANCED_FACE('',(#964),#234,.F.);
#9755=ADVANCED_FACE('',(#965),#9227,.T.);
#9756=ADVANCED_FACE('',(#966),#429,.F.);
#9757=ADVANCED_FACE('',(#967),#430,.F.);
#9758=ADVANCED_FACE('',(#968),#431,.F.);
#9759=ADVANCED_FACE('',(#969),#432,.F.);
#9760=ADVANCED_FACE('',(#970),#433,.F.);
#9761=ADVANCED_FACE('',(#971),#434,.F.);
#9762=ADVANCED_FACE('',(#972),#435,.F.);
#9763=ADVANCED_FACE('',(#973,#300),#436,.T.);
#9764=ADVANCED_FACE('',(#974),#9228,.T.);
#9765=ADVANCED_FACE('',(#975,#301),#437,.F.);
#9766=ADVANCED_FACE('',(#976),#438,.T.);
#9767=CLOSED_SHELL('',(#9229,#9230,#9231,#9232,#9233,#9234,#9235,#9236,
#9237,#9238,#9239,#9240,#9241,#9242,#9243,#9244,#9245,#9246,#9247,#9248,
#9249,#9250,#9251,#9252,#9253,#9254,#9255,#9256,#9257,#9258,#9259,#9260,
#9261,#9262,#9263,#9264,#9265,#9266,#9267,#9268,#9269,#9270,#9271,#9272,
#9273,#9274,#9275,#9276,#9277,#9278,#9279,#9280,#9281,#9282,#9283,#9284,
#9285,#9286,#9287,#9288,#9289,#9290,#9291,#9292,#9293,#9294,#9295,#9296,
#9297,#9298,#9299,#9300,#9301,#9302,#9303,#9304,#9305,#9306,#9307,#9308,
#9309,#9310,#9311,#9312,#9313,#9314,#9315,#9316,#9317,#9318,#9319,#9320,
#9321,#9322,#9323,#9324,#9325,#9326,#9327,#9328,#9329,#9330,#9331,#9332,
#9333,#9334,#9335,#9336,#9337,#9338,#9339,#9340,#9341,#9342,#9343,#9344,
#9345,#9346,#9347,#9348,#9349,#9350,#9351,#9352,#9353,#9354,#9355,#9356,
#9357,#9358,#9359,#9360,#9361,#9362,#9363,#9364,#9365,#9366,#9367,#9368,
#9369,#9370,#9371,#9372,#9373,#9374,#9375,#9376,#9377,#9378,#9379,#9380,
#9381,#9382,#9383,#9384,#9385,#9386,#9387,#9388));
#9768=CLOSED_SHELL('',(#9389,#9390,#9391,#9392,#9393,#9394,#9395,#9396,
#9397,#9398,#9399));
#9769=CLOSED_SHELL('',(#9400,#9401,#9402,#9403,#9404,#9405));
#9770=CLOSED_SHELL('',(#9406,#9407,#9408,#9409,#9410,#9411,#9412,#9413,
#9414,#9415,#9416,#9417,#9418,#9419,#9420,#9421,#9422,#9423,#9424,#9425,
#9426,#9427,#9428,#9429,#9430,#9431,#9432,#9433,#9434,#9435,#9436,#9437,
#9438,#9439,#9440,#9441,#9442,#9443,#9444,#9445,#9446,#9447,#9448,#9449,
#9450,#9451,#9452,#9453,#9454,#9455,#9456,#9457,#9458,#9459,#9460,#9461,
#9462,#9463,#9464,#9465,#9466,#9467));
#9771=CLOSED_SHELL('',(#9468,#9469,#9470,#9471,#9472,#9473,#9474,#9475));
#9772=CLOSED_SHELL('',(#9476,#9477,#9478,#9479,#9480,#9481,#9482,#9483));
#9773=CLOSED_SHELL('',(#9484,#9485,#9486,#9487,#9488,#9489,#9490,#9491,
#9492,#9493,#9494,#9495,#9496,#9497,#9498,#9499,#9500,#9501,#9502,#9503,
#9504,#9505,#9506,#9507,#9508,#9509,#9510,#9511,#9512,#9513,#9514,#9515,
#9516,#9517,#9518,#9519,#9520,#9521,#9522,#9523,#9524,#9525,#9526,#9527,
#9528,#9529,#9530,#9531,#9532,#9533,#9534,#9535,#9536,#9537,#9538,#9539,
#9540,#9541,#9542,#9543,#9544,#9545,#9546,#9547,#9548,#9549,#9550,#9551,
#9552,#9553,#9554,#9555,#9556,#9557,#9558,#9559,#9560,#9561,#9562));
#9774=CLOSED_SHELL('',(#9563,#9564,#9565,#9566,#9567,#9568,#9569,#9570,
#9571,#9572,#9573,#9574,#9575,#9576,#9577,#9578,#9579,#9580,#9581,#9582,
#9583,#9584,#9585,#9586,#9587,#9588,#9589,#9590,#9591,#9592,#9593,#9594,
#9595,#9596,#9597));
#9775=CLOSED_SHELL('',(#9598,#9599,#9600,#9601,#9602,#9603,#9604));
#9776=CLOSED_SHELL('',(#9605,#9606,#9607,#9608));
#9777=CLOSED_SHELL('',(#9609,#9610,#9611,#9612,#9613,#9614,#9615,#9616,
#9617));
#9778=CLOSED_SHELL('',(#9618,#9619,#9620,#9621,#9622,#9623));
#9779=CLOSED_SHELL('',(#9624,#9625,#9626));
#9780=CLOSED_SHELL('',(#9627,#9628,#9629,#9630));
#9781=CLOSED_SHELL('',(#9631,#9632,#9633,#9634,#9635,#9636,#9637,#9638,
#9639,#9640,#9641,#9642,#9643,#9644,#9645,#9646,#9647,#9648,#9649,#9650,
#9651,#9652,#9653,#9654,#9655,#9656,#9657,#9658,#9659,#9660,#9661,#9662,
#9663,#9664,#9665,#9666,#9667,#9668,#9669,#9670,#9671,#9672,#9673,#9674,
#9675,#9676,#9677,#9678));
#9782=CLOSED_SHELL('',(#9679,#9680,#9681,#9682,#9683,#9684,#9685,#9686,
#9687,#9688,#9689,#9690,#9691,#9692,#9693,#9694,#9695,#9696,#9697,#9698,
#9699,#9700,#9701,#9702,#9703,#9704,#9705,#9706,#9707,#9708,#9709,#9710,
#9711,#9712,#9713,#9714));
#9783=CLOSED_SHELL('',(#9715,#9716,#9717,#9718,#9719,#9720,#9721,#9722,
#9723,#9724,#9725,#9726,#9727,#9728,#9729,#9730,#9731,#9732,#9733,#9734,
#9735,#9736,#9737,#9738,#9739,#9740,#9741,#9742,#9743,#9744,#9745,#9746,
#9747,#9748,#9749,#9750,#9751,#9752,#9753,#9754,#9755,#9756,#9757,#9758,
#9759,#9760,#9761,#9762,#9763,#9764,#9765,#9766));
#9784=DERIVED_UNIT_ELEMENT(#9818,1.);
#9785=DERIVED_UNIT_ELEMENT(#36484,-3.);
#9786=DERIVED_UNIT_ELEMENT(#9818,1.);
#9787=DERIVED_UNIT_ELEMENT(#36484,-3.);
#9788=DERIVED_UNIT_ELEMENT(#9818,1.);
#9789=DERIVED_UNIT_ELEMENT(#36484,-3.);
#9790=DERIVED_UNIT_ELEMENT(#9818,1.);
#9791=DERIVED_UNIT_ELEMENT(#36484,-3.);
#9792=DERIVED_UNIT_ELEMENT(#9818,1.);
#9793=DERIVED_UNIT_ELEMENT(#36484,-3.);
#9794=DERIVED_UNIT_ELEMENT(#9818,1.);
#9795=DERIVED_UNIT_ELEMENT(#36484,-3.);
#9796=DERIVED_UNIT_ELEMENT(#9818,1.);
#9797=DERIVED_UNIT_ELEMENT(#36484,-3.);
#9798=DERIVED_UNIT_ELEMENT(#9818,1.);
#9799=DERIVED_UNIT_ELEMENT(#36484,-3.);
#9800=DERIVED_UNIT_ELEMENT(#9818,1.);
#9801=DERIVED_UNIT_ELEMENT(#36484,-3.);
#9802=DERIVED_UNIT_ELEMENT(#9818,1.);
#9803=DERIVED_UNIT_ELEMENT(#36484,-3.);
#9804=DERIVED_UNIT_ELEMENT(#9818,1.);
#9805=DERIVED_UNIT_ELEMENT(#36484,-3.);
#9806=DERIVED_UNIT_ELEMENT(#9818,1.);
#9807=DERIVED_UNIT_ELEMENT(#36484,-3.);
#9808=DERIVED_UNIT_ELEMENT(#9818,1.);
#9809=DERIVED_UNIT_ELEMENT(#36484,-3.);
#9810=DERIVED_UNIT_ELEMENT(#9818,1.);
#9811=DERIVED_UNIT_ELEMENT(#36484,-3.);
#9812=DERIVED_UNIT_ELEMENT(#9818,1.);
#9813=DERIVED_UNIT_ELEMENT(#36484,-3.);
#9814=DERIVED_UNIT_ELEMENT(#9818,1.);
#9815=DERIVED_UNIT_ELEMENT(#36484,-3.);
#9816=DERIVED_UNIT_ELEMENT(#9818,1.);
#9817=DERIVED_UNIT_ELEMENT(#36484,-3.);
#9818=(
MASS_UNIT()
NAMED_UNIT(*)
SI_UNIT(.KILO.,.GRAM.)
);
#9819=DERIVED_UNIT((#9784,#9785));
#9820=DERIVED_UNIT((#9786,#9787));
#9821=DERIVED_UNIT((#9788,#9789));
#9822=DERIVED_UNIT((#9790,#9791));
#9823=DERIVED_UNIT((#9792,#9793));
#9824=DERIVED_UNIT((#9794,#9795));
#9825=DERIVED_UNIT((#9796,#9797));
#9826=DERIVED_UNIT((#9798,#9799));
#9827=DERIVED_UNIT((#9800,#9801));
#9828=DERIVED_UNIT((#9802,#9803));
#9829=DERIVED_UNIT((#9804,#9805));
#9830=DERIVED_UNIT((#9806,#9807));
#9831=DERIVED_UNIT((#9808,#9809));
#9832=DERIVED_UNIT((#9810,#9811));
#9833=DERIVED_UNIT((#9812,#9813));
#9834=DERIVED_UNIT((#9814,#9815));
#9835=DERIVED_UNIT((#9816,#9817));
#9836=MEASURE_REPRESENTATION_ITEM('density measure',
POSITIVE_RATIO_MEASURE(7850.),#9819);
#9837=MEASURE_REPRESENTATION_ITEM('density measure',
POSITIVE_RATIO_MEASURE(7850.),#9820);
#9838=MEASURE_REPRESENTATION_ITEM('density measure',
POSITIVE_RATIO_MEASURE(1200.),#9821);
#9839=MEASURE_REPRESENTATION_ITEM('density measure',
POSITIVE_RATIO_MEASURE(1425.),#9822);
#9840=MEASURE_REPRESENTATION_ITEM('density measure',
POSITIVE_RATIO_MEASURE(8920.),#9823);
#9841=MEASURE_REPRESENTATION_ITEM('density measure',
POSITIVE_RATIO_MEASURE(1425.),#9824);
#9842=MEASURE_REPRESENTATION_ITEM('density measure',
POSITIVE_RATIO_MEASURE(1425.),#9825);
#9843=MEASURE_REPRESENTATION_ITEM('density measure',
POSITIVE_RATIO_MEASURE(8920.),#9826);
#9844=MEASURE_REPRESENTATION_ITEM('density measure',
POSITIVE_RATIO_MEASURE(8920.),#9827);
#9845=MEASURE_REPRESENTATION_ITEM('density measure',
POSITIVE_RATIO_MEASURE(8920.),#9828);
#9846=MEASURE_REPRESENTATION_ITEM('density measure',
POSITIVE_RATIO_MEASURE(7850.),#9829);
#9847=MEASURE_REPRESENTATION_ITEM('density measure',
POSITIVE_RATIO_MEASURE(7850.),#9830);
#9848=MEASURE_REPRESENTATION_ITEM('density measure',
POSITIVE_RATIO_MEASURE(7850.),#9831);
#9849=MEASURE_REPRESENTATION_ITEM('density measure',
POSITIVE_RATIO_MEASURE(7850.),#9832);
#9850=MEASURE_REPRESENTATION_ITEM('density measure',
POSITIVE_RATIO_MEASURE(7850.),#9833);
#9851=MEASURE_REPRESENTATION_ITEM('density measure',
POSITIVE_RATIO_MEASURE(7850.),#9834);
#9852=MEASURE_REPRESENTATION_ITEM('density measure',
POSITIVE_RATIO_MEASURE(7850.),#9835);
#9853=PROPERTY_DEFINITION_REPRESENTATION(#9938,#9887);
#9854=PROPERTY_DEFINITION_REPRESENTATION(#9939,#9888);
#9855=PROPERTY_DEFINITION_REPRESENTATION(#9940,#9889);
#9856=PROPERTY_DEFINITION_REPRESENTATION(#9941,#9890);
#9857=PROPERTY_DEFINITION_REPRESENTATION(#9942,#9891);
#9858=PROPERTY_DEFINITION_REPRESENTATION(#9943,#9892);
#9859=PROPERTY_DEFINITION_REPRESENTATION(#9944,#9893);
#9860=PROPERTY_DEFINITION_REPRESENTATION(#9945,#9894);
#9861=PROPERTY_DEFINITION_REPRESENTATION(#9946,#9895);
#9862=PROPERTY_DEFINITION_REPRESENTATION(#9947,#9896);
#9863=PROPERTY_DEFINITION_REPRESENTATION(#9948,#9897);
#9864=PROPERTY_DEFINITION_REPRESENTATION(#9949,#9898);
#9865=PROPERTY_DEFINITION_REPRESENTATION(#9950,#9899);
#9866=PROPERTY_DEFINITION_REPRESENTATION(#9951,#9900);
#9867=PROPERTY_DEFINITION_REPRESENTATION(#9952,#9901);
#9868=PROPERTY_DEFINITION_REPRESENTATION(#9953,#9902);
#9869=PROPERTY_DEFINITION_REPRESENTATION(#9954,#9903);
#9870=PROPERTY_DEFINITION_REPRESENTATION(#9955,#9904);
#9871=PROPERTY_DEFINITION_REPRESENTATION(#9956,#9905);
#9872=PROPERTY_DEFINITION_REPRESENTATION(#9957,#9906);
#9873=PROPERTY_DEFINITION_REPRESENTATION(#9958,#9907);
#9874=PROPERTY_DEFINITION_REPRESENTATION(#9959,#9908);
#9875=PROPERTY_DEFINITION_REPRESENTATION(#9960,#9909);
#9876=PROPERTY_DEFINITION_REPRESENTATION(#9961,#9910);
#9877=PROPERTY_DEFINITION_REPRESENTATION(#9962,#9911);
#9878=PROPERTY_DEFINITION_REPRESENTATION(#9963,#9912);
#9879=PROPERTY_DEFINITION_REPRESENTATION(#9964,#9913);
#9880=PROPERTY_DEFINITION_REPRESENTATION(#9965,#9914);
#9881=PROPERTY_DEFINITION_REPRESENTATION(#9966,#9915);
#9882=PROPERTY_DEFINITION_REPRESENTATION(#9967,#9916);
#9883=PROPERTY_DEFINITION_REPRESENTATION(#9968,#9917);
#9884=PROPERTY_DEFINITION_REPRESENTATION(#9969,#9918);
#9885=PROPERTY_DEFINITION_REPRESENTATION(#9970,#9919);
#9886=PROPERTY_DEFINITION_REPRESENTATION(#9971,#9920);
#9887=REPRESENTATION('material name',(#9921),#36465);
#9888=REPRESENTATION('density',(#9836),#36465);
#9889=REPRESENTATION('material name',(#9922),#36466);
#9890=REPRESENTATION('density',(#9837),#36466);
#9891=REPRESENTATION('material name',(#9923),#36467);
#9892=REPRESENTATION('density',(#9838),#36467);
#9893=REPRESENTATION('material name',(#9924),#36468);
#9894=REPRESENTATION('density',(#9839),#36468);
#9895=REPRESENTATION('material name',(#9925),#36469);
#9896=REPRESENTATION('density',(#9840),#36469);
#9897=REPRESENTATION('material name',(#9926),#36470);
#9898=REPRESENTATION('density',(#9841),#36470);
#9899=REPRESENTATION('material name',(#9927),#36471);
#9900=REPRESENTATION('density',(#9842),#36471);
#9901=REPRESENTATION('material name',(#9928),#36472);
#9902=REPRESENTATION('density',(#9843),#36472);
#9903=REPRESENTATION('material name',(#9929),#36473);
#9904=REPRESENTATION('density',(#9844),#36473);
#9905=REPRESENTATION('material name',(#9930),#36474);
#9906=REPRESENTATION('density',(#9845),#36474);
#9907=REPRESENTATION('material name',(#9931),#36475);
#9908=REPRESENTATION('density',(#9846),#36475);
#9909=REPRESENTATION('material name',(#9932),#36476);
#9910=REPRESENTATION('density',(#9847),#36476);
#9911=REPRESENTATION('material name',(#9933),#36477);
#9912=REPRESENTATION('density',(#9848),#36477);
#9913=REPRESENTATION('material name',(#9934),#36478);
#9914=REPRESENTATION('density',(#9849),#36478);
#9915=REPRESENTATION('material name',(#9935),#36479);
#9916=REPRESENTATION('density',(#9850),#36479);
#9917=REPRESENTATION('material name',(#9936),#36480);
#9918=REPRESENTATION('density',(#9851),#36480);
#9919=REPRESENTATION('material name',(#9937),#36481);
#9920=REPRESENTATION('density',(#9852),#36481);
#9921=DESCRIPTIVE_REPRESENTATION_ITEM('Steel','Steel');
#9922=DESCRIPTIVE_REPRESENTATION_ITEM('Steel','Steel');
#9923=DESCRIPTIVE_REPRESENTATION_ITEM('Rubber, Nitrile',
'Rubber, Nitrile');
#9924=DESCRIPTIVE_REPRESENTATION_ITEM('Acetal Resin, White',
'Acetal Resin, White');
#9925=DESCRIPTIVE_REPRESENTATION_ITEM('Copper, Alloy','Copper, Alloy');
#9926=DESCRIPTIVE_REPRESENTATION_ITEM('Acetal Resin, White',
'Acetal Resin, White');
#9927=DESCRIPTIVE_REPRESENTATION_ITEM('Acetal Resin, White',
'Acetal Resin, White');
#9928=DESCRIPTIVE_REPRESENTATION_ITEM('Copper, Alloy','Copper, Alloy');
#9929=DESCRIPTIVE_REPRESENTATION_ITEM('Copper, Alloy','Copper, Alloy');
#9930=DESCRIPTIVE_REPRESENTATION_ITEM('Copper, Alloy','Copper, Alloy');
#9931=DESCRIPTIVE_REPRESENTATION_ITEM('Steel','Steel');
#9932=DESCRIPTIVE_REPRESENTATION_ITEM('Steel','Steel');
#9933=DESCRIPTIVE_REPRESENTATION_ITEM('Steel','Steel');
#9934=DESCRIPTIVE_REPRESENTATION_ITEM('Steel','Steel');
#9935=DESCRIPTIVE_REPRESENTATION_ITEM('Steel','Steel');
#9936=DESCRIPTIVE_REPRESENTATION_ITEM('Steel','Steel');
#9937=DESCRIPTIVE_REPRESENTATION_ITEM('Steel','Steel');
#9938=PROPERTY_DEFINITION('material property','material name',#36574);
#9939=PROPERTY_DEFINITION('material property','density of part',#36574);
#9940=PROPERTY_DEFINITION('material property','material name',#36575);
#9941=PROPERTY_DEFINITION('material property','density of part',#36575);
#9942=PROPERTY_DEFINITION('material property','material name',#36576);
#9943=PROPERTY_DEFINITION('material property','density of part',#36576);
#9944=PROPERTY_DEFINITION('material property','material name',#36577);
#9945=PROPERTY_DEFINITION('material property','density of part',#36577);
#9946=PROPERTY_DEFINITION('material property','material name',#36578);
#9947=PROPERTY_DEFINITION('material property','density of part',#36578);
#9948=PROPERTY_DEFINITION('material property','material name',#36579);
#9949=PROPERTY_DEFINITION('material property','density of part',#36579);
#9950=PROPERTY_DEFINITION('material property','material name',#36580);
#9951=PROPERTY_DEFINITION('material property','density of part',#36580);
#9952=PROPERTY_DEFINITION('material property','material name',#36581);
#9953=PROPERTY_DEFINITION('material property','density of part',#36581);
#9954=PROPERTY_DEFINITION('material property','material name',#36582);
#9955=PROPERTY_DEFINITION('material property','density of part',#36582);
#9956=PROPERTY_DEFINITION('material property','material name',#36583);
#9957=PROPERTY_DEFINITION('material property','density of part',#36583);
#9958=PROPERTY_DEFINITION('material property','material name',#36584);
#9959=PROPERTY_DEFINITION('material property','density of part',#36584);
#9960=PROPERTY_DEFINITION('material property','material name',#36585);
#9961=PROPERTY_DEFINITION('material property','density of part',#36585);
#9962=PROPERTY_DEFINITION('material property','material name',#36586);
#9963=PROPERTY_DEFINITION('material property','density of part',#36586);
#9964=PROPERTY_DEFINITION('material property','material name',#36587);
#9965=PROPERTY_DEFINITION('material property','density of part',#36587);
#9966=PROPERTY_DEFINITION('material property','material name',#36588);
#9967=PROPERTY_DEFINITION('material property','density of part',#36588);
#9968=PROPERTY_DEFINITION('material property','material name',#36589);
#9969=PROPERTY_DEFINITION('material property','density of part',#36589);
#9970=PROPERTY_DEFINITION('material property','material name',#36590);
#9971=PROPERTY_DEFINITION('material property','density of part',#36590);
#9972=AXIS2_PLACEMENT_3D('',#12700,#10690,#10691);
#9973=AXIS2_PLACEMENT_3D('',#12701,#10692,#10693);
#9974=AXIS2_PLACEMENT_3D('',#12702,#10694,#10695);
#9975=AXIS2_PLACEMENT_3D('',#12730,#10697,#10698);
#9976=AXIS2_PLACEMENT_3D('',#12741,#10700,#10701);
#9977=AXIS2_PLACEMENT_3D('',#12764,#10702,#10703);
#9978=AXIS2_PLACEMENT_3D('',#12815,#10705,#10706);
#9979=AXIS2_PLACEMENT_3D('',#12863,#10708,#10709);
#9980=AXIS2_PLACEMENT_3D('',#12911,#10711,#10712);
#9981=AXIS2_PLACEMENT_3D('',#12962,#10714,#10715);
#9982=AXIS2_PLACEMENT_3D('',#13010,#10717,#10718);
#9983=AXIS2_PLACEMENT_3D('',#13058,#10720,#10721);
#9984=AXIS2_PLACEMENT_3D('',#13109,#10723,#10724);
#9985=AXIS2_PLACEMENT_3D('',#13160,#10726,#10727);
#9986=AXIS2_PLACEMENT_3D('',#13208,#10729,#10730);
#9987=AXIS2_PLACEMENT_3D('',#13259,#10732,#10733);
#9988=AXIS2_PLACEMENT_3D('',#13278,#10735,#10736);
#9989=AXIS2_PLACEMENT_3D('',#13298,#10737,#10738);
#9990=AXIS2_PLACEMENT_3D('',#13311,#10740,#10741);
#9991=AXIS2_PLACEMENT_3D('',#13320,#10742,#10743);
#9992=AXIS2_PLACEMENT_3D('',#13344,#10745,#10746);
#9993=AXIS2_PLACEMENT_3D('',#13369,#10748,#10749);
#9994=AXIS2_PLACEMENT_3D('',#13394,#10751,#10752);
#9995=AXIS2_PLACEMENT_3D('',#13418,#10754,#10755);
#9996=AXIS2_PLACEMENT_3D('',#13443,#10757,#10758);
#9997=AXIS2_PLACEMENT_3D('',#13467,#10760,#10761);
#9998=AXIS2_PLACEMENT_3D('',#13492,#10763,#10764);
#9999=AXIS2_PLACEMENT_3D('',#13516,#10766,#10767);
#10000=AXIS2_PLACEMENT_3D('',#13541,#10769,#10770);
#10001=AXIS2_PLACEMENT_3D('',#13566,#10772,#10773);
#10002=AXIS2_PLACEMENT_3D('',#13590,#10775,#10776);
#10003=AXIS2_PLACEMENT_3D('',#13601,#10778,#10779);
#10004=AXIS2_PLACEMENT_3D('',#13607,#10780,#10781);
#10005=AXIS2_PLACEMENT_3D('',#13635,#10783,#10784);
#10006=AXIS2_PLACEMENT_3D('',#13646,#10786,#10787);
#10007=AXIS2_PLACEMENT_3D('',#13669,#10788,#10789);
#10008=AXIS2_PLACEMENT_3D('',#13720,#10791,#10792);
#10009=AXIS2_PLACEMENT_3D('',#13768,#10794,#10795);
#10010=AXIS2_PLACEMENT_3D('',#13816,#10797,#10798);
#10011=AXIS2_PLACEMENT_3D('',#13867,#10800,#10801);
#10012=AXIS2_PLACEMENT_3D('',#13915,#10803,#10804);
#10013=AXIS2_PLACEMENT_3D('',#13963,#10806,#10807);
#10014=AXIS2_PLACEMENT_3D('',#14014,#10809,#10810);
#10015=AXIS2_PLACEMENT_3D('',#14065,#10812,#10813);
#10016=AXIS2_PLACEMENT_3D('',#14113,#10815,#10816);
#10017=AXIS2_PLACEMENT_3D('',#14164,#10818,#10819);
#10018=AXIS2_PLACEMENT_3D('',#14183,#10821,#10822);
#10019=AXIS2_PLACEMENT_3D('',#14203,#10823,#10824);
#10020=AXIS2_PLACEMENT_3D('',#14216,#10826,#10827);
#10021=AXIS2_PLACEMENT_3D('',#14225,#10828,#10829);
#10022=AXIS2_PLACEMENT_3D('',#14249,#10831,#10832);
#10023=AXIS2_PLACEMENT_3D('',#14274,#10834,#10835);
#10024=AXIS2_PLACEMENT_3D('',#14299,#10837,#10838);
#10025=AXIS2_PLACEMENT_3D('',#14323,#10840,#10841);
#10026=AXIS2_PLACEMENT_3D('',#14348,#10843,#10844);
#10027=AXIS2_PLACEMENT_3D('',#14372,#10846,#10847);
#10028=AXIS2_PLACEMENT_3D('',#14397,#10849,#10850);
#10029=AXIS2_PLACEMENT_3D('',#14421,#10852,#10853);
#10030=AXIS2_PLACEMENT_3D('',#14446,#10855,#10856);
#10031=AXIS2_PLACEMENT_3D('',#14471,#10858,#10859);
#10032=AXIS2_PLACEMENT_3D('',#14495,#10861,#10862);
#10033=AXIS2_PLACEMENT_3D('',#14506,#10864,#10865);
#10034=AXIS2_PLACEMENT_3D('',#14512,#10866,#10867);
#10035=AXIS2_PLACEMENT_3D('',#14540,#10869,#10870);
#10036=AXIS2_PLACEMENT_3D('',#14551,#10872,#10873);
#10037=AXIS2_PLACEMENT_3D('',#14574,#10874,#10875);
#10038=AXIS2_PLACEMENT_3D('',#14625,#10877,#10878);
#10039=AXIS2_PLACEMENT_3D('',#14673,#10880,#10881);
#10040=AXIS2_PLACEMENT_3D('',#14721,#10883,#10884);
#10041=AXIS2_PLACEMENT_3D('',#14772,#10886,#10887);
#10042=AXIS2_PLACEMENT_3D('',#14820,#10889,#10890);
#10043=AXIS2_PLACEMENT_3D('',#14868,#10892,#10893);
#10044=AXIS2_PLACEMENT_3D('',#14919,#10895,#10896);
#10045=AXIS2_PLACEMENT_3D('',#14970,#10898,#10899);
#10046=AXIS2_PLACEMENT_3D('',#15018,#10901,#10902);
#10047=AXIS2_PLACEMENT_3D('',#15069,#10904,#10905);
#10048=AXIS2_PLACEMENT_3D('',#15088,#10907,#10908);
#10049=AXIS2_PLACEMENT_3D('',#15108,#10909,#10910);
#10050=AXIS2_PLACEMENT_3D('',#15121,#10912,#10913);
#10051=AXIS2_PLACEMENT_3D('',#15130,#10914,#10915);
#10052=AXIS2_PLACEMENT_3D('',#15154,#10917,#10918);
#10053=AXIS2_PLACEMENT_3D('',#15179,#10920,#10921);
#10054=AXIS2_PLACEMENT_3D('',#15204,#10923,#10924);
#10055=AXIS2_PLACEMENT_3D('',#15228,#10926,#10927);
#10056=AXIS2_PLACEMENT_3D('',#15253,#10929,#10930);
#10057=AXIS2_PLACEMENT_3D('',#15277,#10932,#10933);
#10058=AXIS2_PLACEMENT_3D('',#15302,#10935,#10936);
#10059=AXIS2_PLACEMENT_3D('',#15326,#10938,#10939);
#10060=AXIS2_PLACEMENT_3D('',#15351,#10941,#10942);
#10061=AXIS2_PLACEMENT_3D('',#15376,#10944,#10945);
#10062=AXIS2_PLACEMENT_3D('',#15400,#10947,#10948);
#10063=AXIS2_PLACEMENT_3D('',#15411,#10950,#10951);
#10064=AXIS2_PLACEMENT_3D('',#15417,#10952,#10953);
#10065=AXIS2_PLACEMENT_3D('',#15445,#10955,#10956);
#10066=AXIS2_PLACEMENT_3D('',#15456,#10958,#10959);
#10067=AXIS2_PLACEMENT_3D('',#15479,#10960,#10961);
#10068=AXIS2_PLACEMENT_3D('',#15530,#10963,#10964);
#10069=AXIS2_PLACEMENT_3D('',#15578,#10966,#10967);
#10070=AXIS2_PLACEMENT_3D('',#15626,#10969,#10970);
#10071=AXIS2_PLACEMENT_3D('',#15677,#10972,#10973);
#10072=AXIS2_PLACEMENT_3D('',#15725,#10975,#10976);
#10073=AXIS2_PLACEMENT_3D('',#15773,#10978,#10979);
#10074=AXIS2_PLACEMENT_3D('',#15824,#10981,#10982);
#10075=AXIS2_PLACEMENT_3D('',#15875,#10984,#10985);
#10076=AXIS2_PLACEMENT_3D('',#15923,#10987,#10988);
#10077=AXIS2_PLACEMENT_3D('',#15974,#10990,#10991);
#10078=AXIS2_PLACEMENT_3D('',#15993,#10993,#10994);
#10079=AXIS2_PLACEMENT_3D('',#16013,#10995,#10996);
#10080=AXIS2_PLACEMENT_3D('',#16026,#10998,#10999);
#10081=AXIS2_PLACEMENT_3D('',#16035,#11000,#11001);
#10082=AXIS2_PLACEMENT_3D('',#16059,#11003,#11004);
#10083=AXIS2_PLACEMENT_3D('',#16084,#11006,#11007);
#10084=AXIS2_PLACEMENT_3D('',#16109,#11009,#11010);
#10085=AXIS2_PLACEMENT_3D('',#16133,#11012,#11013);
#10086=AXIS2_PLACEMENT_3D('',#16158,#11015,#11016);
#10087=AXIS2_PLACEMENT_3D('',#16182,#11018,#11019);
#10088=AXIS2_PLACEMENT_3D('',#16207,#11021,#11022);
#10089=AXIS2_PLACEMENT_3D('',#16231,#11024,#11025);
#10090=AXIS2_PLACEMENT_3D('',#16256,#11027,#11028);
#10091=AXIS2_PLACEMENT_3D('',#16281,#11030,#11031);
#10092=AXIS2_PLACEMENT_3D('',#16305,#11033,#11034);
#10093=AXIS2_PLACEMENT_3D('',#16316,#11036,#11037);
#10094=AXIS2_PLACEMENT_3D('',#16322,#11038,#11039);
#10095=AXIS2_PLACEMENT_3D('',#16325,#11040,#11041);
#10096=AXIS2_PLACEMENT_3D('',#16329,#11043,#11044);
#10097=AXIS2_PLACEMENT_3D('',#16331,#11046,#11047);
#10098=AXIS2_PLACEMENT_3D('',#16337,#11051,#11052);
#10099=AXIS2_PLACEMENT_3D('',#16339,#11053,#11054);
#10100=AXIS2_PLACEMENT_3D('',#16342,#11056,#11057);
#10101=AXIS2_PLACEMENT_3D('',#16343,#11058,#11059);
#10102=AXIS2_PLACEMENT_3D('',#16349,#11063,#11064);
#10103=AXIS2_PLACEMENT_3D('',#16352,#11065,#11066);
#10104=AXIS2_PLACEMENT_3D('',#16356,#11068,#11069);
#10105=AXIS2_PLACEMENT_3D('',#16358,#11071,#11072);
#10106=AXIS2_PLACEMENT_3D('',#16362,#11075,#11076);
#10107=AXIS2_PLACEMENT_3D('',#16364,#11077,#11078);
#10108=AXIS2_PLACEMENT_3D('',#16366,#11079,#11080);
#10109=AXIS2_PLACEMENT_3D('',#16368,#11081,#11082);
#10110=AXIS2_PLACEMENT_3D('',#16369,#11083,#11084);
#10111=AXIS2_PLACEMENT_3D('',#16374,#11087,#11088);
#10112=AXIS2_PLACEMENT_3D('',#16375,#11089,#11090);
#10113=AXIS2_PLACEMENT_3D('',#16376,#11091,#11092);
#10114=AXIS2_PLACEMENT_3D('',#16377,#11093,#11094);
#10115=AXIS2_PLACEMENT_3D('',#16379,#11095,#11096);
#10116=AXIS2_PLACEMENT_3D('',#16381,#11098,#11099);
#10117=AXIS2_PLACEMENT_3D('',#16383,#11100,#11101);
#10118=AXIS2_PLACEMENT_3D('',#16385,#11102,#11103);
#10119=AXIS2_PLACEMENT_3D('',#16386,#11104,#11105);
#10120=AXIS2_PLACEMENT_3D('',#16388,#11106,#11107);
#10121=AXIS2_PLACEMENT_3D('',#16390,#11109,#11110);
#10122=AXIS2_PLACEMENT_3D('',#16392,#11112,#11113);
#10123=AXIS2_PLACEMENT_3D('',#16394,#11114,#11115);
#10124=AXIS2_PLACEMENT_3D('',#16396,#11116,#11117);
#10125=AXIS2_PLACEMENT_3D('',#16397,#11118,#11119);
#10126=AXIS2_PLACEMENT_3D('',#16399,#11120,#11121);
#10127=AXIS2_PLACEMENT_3D('',#16401,#11123,#11124);
#10128=AXIS2_PLACEMENT_3D('',#16403,#11126,#11127);
#10129=AXIS2_PLACEMENT_3D('',#16514,#11128,#11129);
#10130=AXIS2_PLACEMENT_3D('',#17375,#11130,#11131);
#10131=AXIS2_PLACEMENT_3D('',#17376,#11132,#11133);
#10132=AXIS2_PLACEMENT_3D('',#17487,#11134,#11135);
#10133=AXIS2_PLACEMENT_3D('',#18348,#11136,#11137);
#10134=AXIS2_PLACEMENT_3D('',#18349,#11138,#11139);
#10135=AXIS2_PLACEMENT_3D('',#18460,#11140,#11141);
#10136=AXIS2_PLACEMENT_3D('',#19321,#11142,#11143);
#10137=AXIS2_PLACEMENT_3D('',#19322,#11144,#11145);
#10138=AXIS2_PLACEMENT_3D('',#19433,#11146,#11147);
#10139=AXIS2_PLACEMENT_3D('',#20294,#11148,#11149);
#10140=AXIS2_PLACEMENT_3D('',#20295,#11150,#11151);
#10141=AXIS2_PLACEMENT_3D('',#20296,#11152,#11153);
#10142=AXIS2_PLACEMENT_3D('',#20297,#11154,#11155);
#10143=AXIS2_PLACEMENT_3D('',#20298,#11156,#11157);
#10144=AXIS2_PLACEMENT_3D('',#20299,#11158,#11159);
#10145=AXIS2_PLACEMENT_3D('',#20301,#11160,#11161);
#10146=AXIS2_PLACEMENT_3D('',#20304,#11163,#11164);
#10147=AXIS2_PLACEMENT_3D('',#20305,#11165,#11166);
#10148=AXIS2_PLACEMENT_3D('',#20307,#11167,#11168);
#10149=AXIS2_PLACEMENT_3D('',#20310,#11170,#11171);
#10150=AXIS2_PLACEMENT_3D('',#20311,#11172,#11173);
#10151=AXIS2_PLACEMENT_3D('',#20320,#11178,#11179);
#10152=AXIS2_PLACEMENT_3D('',#20326,#11183,#11184);
#10153=AXIS2_PLACEMENT_3D('',#20332,#11188,#11189);
#10154=AXIS2_PLACEMENT_3D('',#20334,#11191,#11192);
#10155=AXIS2_PLACEMENT_3D('',#20343,#11197,#11198);
#10156=AXIS2_PLACEMENT_3D('',#20352,#11203,#11204);
#10157=AXIS2_PLACEMENT_3D('',#20355,#11207,#11208);
#10158=AXIS2_PLACEMENT_3D('',#20357,#11210,#11211);
#10159=AXIS2_PLACEMENT_3D('',#20359,#11212,#11213);
#10160=AXIS2_PLACEMENT_3D('',#20362,#11215,#11216);
#10161=AXIS2_PLACEMENT_3D('',#20363,#11217,#11218);
#10162=AXIS2_PLACEMENT_3D('',#20365,#11219,#11220);
#10163=AXIS2_PLACEMENT_3D('',#20367,#11222,#11223);
#10164=AXIS2_PLACEMENT_3D('',#20368,#11224,#11225);
#10165=AXIS2_PLACEMENT_3D('',#20370,#11227,#11228);
#10166=AXIS2_PLACEMENT_3D('',#20371,#11229,#11230);
#10167=AXIS2_PLACEMENT_3D('',#20380,#11235,#11236);
#10168=AXIS2_PLACEMENT_3D('',#20387,#11241,#11242);
#10169=AXIS2_PLACEMENT_3D('',#20393,#11246,#11247);
#10170=AXIS2_PLACEMENT_3D('',#20397,#11251,#11252);
#10171=AXIS2_PLACEMENT_3D('',#20398,#11253,#11254);
#10172=AXIS2_PLACEMENT_3D('',#20399,#11255,#11256);
#10173=AXIS2_PLACEMENT_3D('',#20400,#11257,#11258);
#10174=AXIS2_PLACEMENT_3D('',#20402,#11259,#11260);
#10175=AXIS2_PLACEMENT_3D('',#20405,#11262,#11263);
#10176=AXIS2_PLACEMENT_3D('',#20406,#11264,#11265);
#10177=AXIS2_PLACEMENT_3D('',#20408,#11266,#11267);
#10178=AXIS2_PLACEMENT_3D('',#20411,#11269,#11270);
#10179=AXIS2_PLACEMENT_3D('',#20412,#11271,#11272);
#10180=AXIS2_PLACEMENT_3D('',#20414,#11273,#11274);
#10181=AXIS2_PLACEMENT_3D('',#20417,#11276,#11277);
#10182=AXIS2_PLACEMENT_3D('',#20418,#11278,#11279);
#10183=AXIS2_PLACEMENT_3D('',#20420,#11280,#11281);
#10184=AXIS2_PLACEMENT_3D('',#20423,#11283,#11284);
#10185=AXIS2_PLACEMENT_3D('',#20424,#11285,#11286);
#10186=AXIS2_PLACEMENT_3D('',#20426,#11287,#11288);
#10187=AXIS2_PLACEMENT_3D('',#20429,#11290,#11291);
#10188=AXIS2_PLACEMENT_3D('',#20430,#11292,#11293);
#10189=AXIS2_PLACEMENT_3D('',#20439,#11298,#11299);
#10190=AXIS2_PLACEMENT_3D('',#20445,#11303,#11304);
#10191=AXIS2_PLACEMENT_3D('',#20451,#11308,#11309);
#10192=AXIS2_PLACEMENT_3D('',#20454,#11312,#11313);
#10193=AXIS2_PLACEMENT_3D('',#20455,#11314,#11315);
#10194=AXIS2_PLACEMENT_3D('',#20456,#11316,#11317);
#10195=AXIS2_PLACEMENT_3D('',#20457,#11318,#11319);
#10196=AXIS2_PLACEMENT_3D('',#20459,#11320,#11321);
#10197=AXIS2_PLACEMENT_3D('',#20461,#11322,#11323);
#10198=AXIS2_PLACEMENT_3D('',#20462,#11324,#11325);
#10199=AXIS2_PLACEMENT_3D('',#20465,#11327,#11328);
#10200=AXIS2_PLACEMENT_3D('',#20466,#11329,#11330);
#10201=AXIS2_PLACEMENT_3D('',#20468,#11331,#11332);
#10202=AXIS2_PLACEMENT_3D('',#20469,#11333,#11334);
#10203=AXIS2_PLACEMENT_3D('',#20471,#11335,#11336);
#10204=AXIS2_PLACEMENT_3D('',#20473,#11338,#11339);
#10205=AXIS2_PLACEMENT_3D('',#20475,#11340,#11341);
#10206=AXIS2_PLACEMENT_3D('',#20477,#11343,#11344);
#10207=AXIS2_PLACEMENT_3D('',#20478,#11345,#11346);
#10208=AXIS2_PLACEMENT_3D('',#20479,#11347,#11348);
#10209=AXIS2_PLACEMENT_3D('',#20489,#11350,#11351);
#10210=AXIS2_PLACEMENT_3D('',#20500,#11352,#11353);
#10211=AXIS2_PLACEMENT_3D('',#20551,#11355,#11356);
#10212=AXIS2_PLACEMENT_3D('',#20602,#11358,#11359);
#10213=AXIS2_PLACEMENT_3D('',#20650,#11361,#11362);
#10214=AXIS2_PLACEMENT_3D('',#20701,#11364,#11365);
#10215=AXIS2_PLACEMENT_3D('',#20752,#11367,#11368);
#10216=AXIS2_PLACEMENT_3D('',#20800,#11370,#11371);
#10217=AXIS2_PLACEMENT_3D('',#20819,#11373,#11374);
#10218=AXIS2_PLACEMENT_3D('',#20839,#11375,#11376);
#10219=AXIS2_PLACEMENT_3D('',#20849,#11378,#11379);
#10220=AXIS2_PLACEMENT_3D('',#20860,#11380,#11381);
#10221=AXIS2_PLACEMENT_3D('',#20911,#11383,#11384);
#10222=AXIS2_PLACEMENT_3D('',#20962,#11386,#11387);
#10223=AXIS2_PLACEMENT_3D('',#21010,#11389,#11390);
#10224=AXIS2_PLACEMENT_3D('',#21061,#11392,#11393);
#10225=AXIS2_PLACEMENT_3D('',#21112,#11395,#11396);
#10226=AXIS2_PLACEMENT_3D('',#21160,#11398,#11399);
#10227=AXIS2_PLACEMENT_3D('',#21179,#11401,#11402);
#10228=AXIS2_PLACEMENT_3D('',#21199,#11403,#11404);
#10229=AXIS2_PLACEMENT_3D('',#21213,#11406,#11407);
#10230=AXIS2_PLACEMENT_3D('',#21223,#11408,#11409);
#10231=AXIS2_PLACEMENT_3D('',#21247,#11411,#11412);
#10232=AXIS2_PLACEMENT_3D('',#21272,#11414,#11415);
#10233=AXIS2_PLACEMENT_3D('',#21297,#11417,#11418);
#10234=AXIS2_PLACEMENT_3D('',#21321,#11420,#11421);
#10235=AXIS2_PLACEMENT_3D('',#21346,#11423,#11424);
#10236=AXIS2_PLACEMENT_3D('',#21371,#11426,#11427);
#10237=AXIS2_PLACEMENT_3D('',#21382,#11429,#11430);
#10238=AXIS2_PLACEMENT_3D('',#21388,#11431,#11432);
#10239=AXIS2_PLACEMENT_3D('',#21402,#11434,#11435);
#10240=AXIS2_PLACEMENT_3D('',#21412,#11436,#11437);
#10241=AXIS2_PLACEMENT_3D('',#21436,#11439,#11440);
#10242=AXIS2_PLACEMENT_3D('',#21461,#11442,#11443);
#10243=AXIS2_PLACEMENT_3D('',#21486,#11445,#11446);
#10244=AXIS2_PLACEMENT_3D('',#21510,#11448,#11449);
#10245=AXIS2_PLACEMENT_3D('',#21535,#11451,#11452);
#10246=AXIS2_PLACEMENT_3D('',#21560,#11454,#11455);
#10247=AXIS2_PLACEMENT_3D('',#21571,#11457,#11458);
#10248=AXIS2_PLACEMENT_3D('',#21577,#11459,#11460);
#10249=AXIS2_PLACEMENT_3D('',#22299,#11461,#11462);
#10250=AXIS2_PLACEMENT_3D('',#22302,#11463,#11464);
#10251=AXIS2_PLACEMENT_3D('',#22413,#11470,#11471);
#10252=AXIS2_PLACEMENT_3D('',#23034,#11472,#11473);
#10253=AXIS2_PLACEMENT_3D('',#23035,#11474,#11475);
#10254=AXIS2_PLACEMENT_3D('',#23036,#11476,#11477);
#10255=AXIS2_PLACEMENT_3D('',#23038,#11478,#11479);
#10256=AXIS2_PLACEMENT_3D('',#23041,#11481,#11482);
#10257=AXIS2_PLACEMENT_3D('',#23042,#11483,#11484);
#10258=AXIS2_PLACEMENT_3D('',#23044,#11485,#11486);
#10259=AXIS2_PLACEMENT_3D('',#23047,#11488,#11489);
#10260=AXIS2_PLACEMENT_3D('',#23048,#11490,#11491);
#10261=AXIS2_PLACEMENT_3D('',#23057,#11496,#11497);
#10262=AXIS2_PLACEMENT_3D('',#23063,#11501,#11502);
#10263=AXIS2_PLACEMENT_3D('',#23077,#11510,#11511);
#10264=AXIS2_PLACEMENT_3D('',#23081,#11514,#11515);
#10265=AXIS2_PLACEMENT_3D('',#23085,#11518,#11519);
#10266=AXIS2_PLACEMENT_3D('',#23089,#11522,#11523);
#10267=AXIS2_PLACEMENT_3D('',#23091,#11524,#11525);
#10268=AXIS2_PLACEMENT_3D('',#23095,#11528,#11529);
#10269=AXIS2_PLACEMENT_3D('',#23097,#11530,#11531);
#10270=AXIS2_PLACEMENT_3D('',#23101,#11534,#11535);
#10271=AXIS2_PLACEMENT_3D('',#23102,#11536,#11537);
#10272=AXIS2_PLACEMENT_3D('',#23105,#11540,#11541);
#10273=AXIS2_PLACEMENT_3D('',#23106,#11542,#11543);
#10274=AXIS2_PLACEMENT_3D('',#23107,#11544,#11545);
#10275=AXIS2_PLACEMENT_3D('',#23113,#11549,#11550);
#10276=AXIS2_PLACEMENT_3D('',#23119,#11554,#11555);
#10277=AXIS2_PLACEMENT_3D('',#23121,#11557,#11558);
#10278=AXIS2_PLACEMENT_3D('',#23127,#11562,#11563);
#10279=AXIS2_PLACEMENT_3D('',#23129,#11565,#11566);
#10280=AXIS2_PLACEMENT_3D('',#23130,#11567,#11568);
#10281=AXIS2_PLACEMENT_3D('',#23131,#11569,#11570);
#10282=AXIS2_PLACEMENT_3D('',#23134,#11572,#11573);
#10283=AXIS2_PLACEMENT_3D('',#23135,#11574,#11575);
#10284=AXIS2_PLACEMENT_3D('',#23136,#11576,#11577);
#10285=AXIS2_PLACEMENT_3D('',#23137,#11578,#11579);
#10286=AXIS2_PLACEMENT_3D('',#23139,#11580,#11581);
#10287=AXIS2_PLACEMENT_3D('',#23142,#11583,#11584);
#10288=AXIS2_PLACEMENT_3D('',#23143,#11585,#11586);
#10289=AXIS2_PLACEMENT_3D('',#23145,#11587,#11588);
#10290=AXIS2_PLACEMENT_3D('',#23148,#11590,#11591);
#10291=AXIS2_PLACEMENT_3D('',#23149,#11592,#11593);
#10292=AXIS2_PLACEMENT_3D('',#23158,#11598,#11599);
#10293=AXIS2_PLACEMENT_3D('',#23164,#11603,#11604);
#10294=AXIS2_PLACEMENT_3D('',#23170,#11608,#11609);
#10295=AXIS2_PLACEMENT_3D('',#23173,#11612,#11613);
#10296=AXIS2_PLACEMENT_3D('',#23174,#11614,#11615);
#10297=AXIS2_PLACEMENT_3D('',#23175,#11616,#11617);
#10298=AXIS2_PLACEMENT_3D('',#23176,#11618,#11619);
#10299=AXIS2_PLACEMENT_3D('',#23178,#11620,#11621);
#10300=AXIS2_PLACEMENT_3D('',#23181,#11623,#11624);
#10301=AXIS2_PLACEMENT_3D('',#23182,#11625,#11626);
#10302=AXIS2_PLACEMENT_3D('',#23184,#11627,#11628);
#10303=AXIS2_PLACEMENT_3D('',#23186,#11630,#11631);
#10304=AXIS2_PLACEMENT_3D('',#23188,#11632,#11633);
#10305=AXIS2_PLACEMENT_3D('',#23189,#11634,#11635);
#10306=AXIS2_PLACEMENT_3D('',#23191,#11636,#11637);
#10307=AXIS2_PLACEMENT_3D('',#23193,#11639,#11640);
#10308=AXIS2_PLACEMENT_3D('',#23195,#11641,#11642);
#10309=AXIS2_PLACEMENT_3D('',#23196,#11643,#11644);
#10310=AXIS2_PLACEMENT_3D('',#23198,#11645,#11646);
#10311=AXIS2_PLACEMENT_3D('',#23200,#11648,#11649);
#10312=AXIS2_PLACEMENT_3D('',#23202,#11650,#11651);
#10313=AXIS2_PLACEMENT_3D('',#23204,#11653,#11654);
#10314=AXIS2_PLACEMENT_3D('',#23206,#11656,#11657);
#10315=AXIS2_PLACEMENT_3D('',#23207,#11658,#11659);
#10316=AXIS2_PLACEMENT_3D('',#23235,#11661,#11662);
#10317=AXIS2_PLACEMENT_3D('',#23246,#11664,#11665);
#10318=AXIS2_PLACEMENT_3D('',#23269,#11666,#11667);
#10319=AXIS2_PLACEMENT_3D('',#23320,#11669,#11670);
#10320=AXIS2_PLACEMENT_3D('',#23368,#11672,#11673);
#10321=AXIS2_PLACEMENT_3D('',#23416,#11675,#11676);
#10322=AXIS2_PLACEMENT_3D('',#23467,#11678,#11679);
#10323=AXIS2_PLACEMENT_3D('',#23515,#11681,#11682);
#10324=AXIS2_PLACEMENT_3D('',#23563,#11684,#11685);
#10325=AXIS2_PLACEMENT_3D('',#23614,#11687,#11688);
#10326=AXIS2_PLACEMENT_3D('',#23665,#11690,#11691);
#10327=AXIS2_PLACEMENT_3D('',#23713,#11693,#11694);
#10328=AXIS2_PLACEMENT_3D('',#23764,#11696,#11697);
#10329=AXIS2_PLACEMENT_3D('',#23783,#11699,#11700);
#10330=AXIS2_PLACEMENT_3D('',#23803,#11701,#11702);
#10331=AXIS2_PLACEMENT_3D('',#23816,#11704,#11705);
#10332=AXIS2_PLACEMENT_3D('',#23825,#11706,#11707);
#10333=AXIS2_PLACEMENT_3D('',#23849,#11709,#11710);
#10334=AXIS2_PLACEMENT_3D('',#23874,#11712,#11713);
#10335=AXIS2_PLACEMENT_3D('',#23899,#11715,#11716);
#10336=AXIS2_PLACEMENT_3D('',#23923,#11718,#11719);
#10337=AXIS2_PLACEMENT_3D('',#23948,#11721,#11722);
#10338=AXIS2_PLACEMENT_3D('',#23972,#11724,#11725);
#10339=AXIS2_PLACEMENT_3D('',#23997,#11727,#11728);
#10340=AXIS2_PLACEMENT_3D('',#24021,#11730,#11731);
#10341=AXIS2_PLACEMENT_3D('',#24046,#11733,#11734);
#10342=AXIS2_PLACEMENT_3D('',#24071,#11736,#11737);
#10343=AXIS2_PLACEMENT_3D('',#24095,#11739,#11740);
#10344=AXIS2_PLACEMENT_3D('',#24106,#11742,#11743);
#10345=AXIS2_PLACEMENT_3D('',#24112,#11744,#11745);
#10346=AXIS2_PLACEMENT_3D('',#24122,#11747,#11748);
#10347=AXIS2_PLACEMENT_3D('',#24125,#11750,#11751);
#10348=AXIS2_PLACEMENT_3D('',#24127,#11752,#11753);
#10349=AXIS2_PLACEMENT_3D('',#24138,#11754,#11755);
#10350=AXIS2_PLACEMENT_3D('',#24189,#11757,#11758);
#10351=AXIS2_PLACEMENT_3D('',#24240,#11760,#11761);
#10352=AXIS2_PLACEMENT_3D('',#24288,#11763,#11764);
#10353=AXIS2_PLACEMENT_3D('',#24339,#11766,#11767);
#10354=AXIS2_PLACEMENT_3D('',#24390,#11769,#11770);
#10355=AXIS2_PLACEMENT_3D('',#24438,#11772,#11773);
#10356=AXIS2_PLACEMENT_3D('',#24489,#11775,#11776);
#10357=AXIS2_PLACEMENT_3D('',#24540,#11778,#11779);
#10358=AXIS2_PLACEMENT_3D('',#24588,#11781,#11782);
#10359=AXIS2_PLACEMENT_3D('',#24639,#11784,#11785);
#10360=AXIS2_PLACEMENT_3D('',#24690,#11787,#11788);
#10361=AXIS2_PLACEMENT_3D('',#24738,#11790,#11791);
#10362=AXIS2_PLACEMENT_3D('',#24789,#11793,#11794);
#10363=AXIS2_PLACEMENT_3D('',#24840,#11796,#11797);
#10364=AXIS2_PLACEMENT_3D('',#24888,#11799,#11800);
#10365=AXIS2_PLACEMENT_3D('',#24939,#11802,#11803);
#10366=AXIS2_PLACEMENT_3D('',#24958,#11805,#11806);
#10367=AXIS2_PLACEMENT_3D('',#24978,#11807,#11808);
#10368=AXIS2_PLACEMENT_3D('',#24992,#11810,#11811);
#10369=AXIS2_PLACEMENT_3D('',#25002,#11812,#11813);
#10370=AXIS2_PLACEMENT_3D('',#25026,#11815,#11816);
#10371=AXIS2_PLACEMENT_3D('',#25051,#11818,#11819);
#10372=AXIS2_PLACEMENT_3D('',#25076,#11821,#11822);
#10373=AXIS2_PLACEMENT_3D('',#25100,#11824,#11825);
#10374=AXIS2_PLACEMENT_3D('',#25125,#11827,#11828);
#10375=AXIS2_PLACEMENT_3D('',#25150,#11830,#11831);
#10376=AXIS2_PLACEMENT_3D('',#25174,#11833,#11834);
#10377=AXIS2_PLACEMENT_3D('',#25199,#11836,#11837);
#10378=AXIS2_PLACEMENT_3D('',#25224,#11839,#11840);
#10379=AXIS2_PLACEMENT_3D('',#25248,#11842,#11843);
#10380=AXIS2_PLACEMENT_3D('',#25273,#11845,#11846);
#10381=AXIS2_PLACEMENT_3D('',#25298,#11848,#11849);
#10382=AXIS2_PLACEMENT_3D('',#25322,#11851,#11852);
#10383=AXIS2_PLACEMENT_3D('',#25347,#11854,#11855);
#10384=AXIS2_PLACEMENT_3D('',#25372,#11857,#11858);
#10385=AXIS2_PLACEMENT_3D('',#25396,#11860,#11861);
#10386=AXIS2_PLACEMENT_3D('',#25407,#11863,#11864);
#10387=AXIS2_PLACEMENT_3D('',#25413,#11865,#11866);
#10388=AXIS2_PLACEMENT_3D('',#25521,#11867,#11868);
#10389=AXIS2_PLACEMENT_3D('',#26640,#11869,#11870);
#10390=AXIS2_PLACEMENT_3D('',#26641,#11871,#11872);
#10391=AXIS2_PLACEMENT_3D('',#26642,#11873,#11874);
#10392=AXIS2_PLACEMENT_3D('',#26753,#11875,#11876);
#10393=AXIS2_PLACEMENT_3D('',#27614,#11877,#11878);
#10394=AXIS2_PLACEMENT_3D('',#27615,#11879,#11880);
#10395=AXIS2_PLACEMENT_3D('',#27616,#11881,#11882);
#10396=AXIS2_PLACEMENT_3D('',#27625,#11887,#11888);
#10397=AXIS2_PLACEMENT_3D('',#27631,#11892,#11893);
#10398=AXIS2_PLACEMENT_3D('',#27637,#11897,#11898);
#10399=AXIS2_PLACEMENT_3D('',#27640,#11901,#11902);
#10400=AXIS2_PLACEMENT_3D('',#27641,#11903,#11904);
#10401=AXIS2_PLACEMENT_3D('',#27642,#11905,#11906);
#10402=AXIS2_PLACEMENT_3D('',#27643,#11907,#11908);
#10403=AXIS2_PLACEMENT_3D('',#27653,#11910,#11911);
#10404=AXIS2_PLACEMENT_3D('',#27656,#11913,#11914);
#10405=AXIS2_PLACEMENT_3D('',#27658,#11915,#11916);
#10406=AXIS2_PLACEMENT_3D('',#27669,#11917,#11918);
#10407=AXIS2_PLACEMENT_3D('',#27720,#11920,#11921);
#10408=AXIS2_PLACEMENT_3D('',#27771,#11923,#11924);
#10409=AXIS2_PLACEMENT_3D('',#27819,#11926,#11927);
#10410=AXIS2_PLACEMENT_3D('',#27867,#11929,#11930);
#10411=AXIS2_PLACEMENT_3D('',#27918,#11932,#11933);
#10412=AXIS2_PLACEMENT_3D('',#27969,#11935,#11936);
#10413=AXIS2_PLACEMENT_3D('',#28017,#11938,#11939);
#10414=AXIS2_PLACEMENT_3D('',#28068,#11941,#11942);
#10415=AXIS2_PLACEMENT_3D('',#28087,#11944,#11945);
#10416=AXIS2_PLACEMENT_3D('',#28107,#11946,#11947);
#10417=AXIS2_PLACEMENT_3D('',#28121,#11949,#11950);
#10418=AXIS2_PLACEMENT_3D('',#28131,#11951,#11952);
#10419=AXIS2_PLACEMENT_3D('',#28155,#11954,#11955);
#10420=AXIS2_PLACEMENT_3D('',#28180,#11957,#11958);
#10421=AXIS2_PLACEMENT_3D('',#28204,#11960,#11961);
#10422=AXIS2_PLACEMENT_3D('',#28229,#11963,#11964);
#10423=AXIS2_PLACEMENT_3D('',#28253,#11966,#11967);
#10424=AXIS2_PLACEMENT_3D('',#28278,#11969,#11970);
#10425=AXIS2_PLACEMENT_3D('',#28303,#11972,#11973);
#10426=AXIS2_PLACEMENT_3D('',#28327,#11975,#11976);
#10427=AXIS2_PLACEMENT_3D('',#28338,#11978,#11979);
#10428=AXIS2_PLACEMENT_3D('',#28344,#11980,#11981);
#10429=AXIS2_PLACEMENT_3D('',#28452,#11982,#11983);
#10430=AXIS2_PLACEMENT_3D('',#29163,#11984,#11985);
#10431=AXIS2_PLACEMENT_3D('',#29164,#11986,#11987);
#10432=AXIS2_PLACEMENT_3D('',#29165,#11988,#11989);
#10433=AXIS2_PLACEMENT_3D('',#29167,#11990,#11991);
#10434=AXIS2_PLACEMENT_3D('',#29170,#11993,#11994);
#10435=AXIS2_PLACEMENT_3D('',#29171,#11995,#11996);
#10436=AXIS2_PLACEMENT_3D('',#29180,#12001,#12002);
#10437=AXIS2_PLACEMENT_3D('',#29186,#12006,#12007);
#10438=AXIS2_PLACEMENT_3D('',#29194,#12012,#12013);
#10439=AXIS2_PLACEMENT_3D('',#29198,#12016,#12017);
#10440=AXIS2_PLACEMENT_3D('',#29204,#12021,#12022);
#10441=AXIS2_PLACEMENT_3D('',#29207,#12025,#12026);
#10442=AXIS2_PLACEMENT_3D('',#29208,#12027,#12028);
#10443=AXIS2_PLACEMENT_3D('',#29209,#12029,#12030);
#10444=AXIS2_PLACEMENT_3D('',#29210,#12031,#12032);
#10445=AXIS2_PLACEMENT_3D('',#29212,#12033,#12034);
#10446=AXIS2_PLACEMENT_3D('',#29215,#12036,#12037);
#10447=AXIS2_PLACEMENT_3D('',#29216,#12038,#12039);
#10448=AXIS2_PLACEMENT_3D('',#29225,#12044,#12045);
#10449=AXIS2_PLACEMENT_3D('',#29231,#12049,#12050);
#10450=AXIS2_PLACEMENT_3D('',#29237,#12054,#12055);
#10451=AXIS2_PLACEMENT_3D('',#29240,#12058,#12059);
#10452=AXIS2_PLACEMENT_3D('',#29241,#12060,#12061);
#10453=AXIS2_PLACEMENT_3D('',#29242,#12062,#12063);
#10454=AXIS2_PLACEMENT_3D('',#29243,#12064,#12065);
#10455=AXIS2_PLACEMENT_3D('',#29245,#12066,#12067);
#10456=AXIS2_PLACEMENT_3D('',#29248,#12069,#12070);
#10457=AXIS2_PLACEMENT_3D('',#29249,#12071,#12072);
#10458=AXIS2_PLACEMENT_3D('',#29251,#12073,#12074);
#10459=AXIS2_PLACEMENT_3D('',#29254,#12076,#12077);
#10460=AXIS2_PLACEMENT_3D('',#29255,#12078,#12079);
#10461=AXIS2_PLACEMENT_3D('',#29256,#12080,#12081);
#10462=AXIS2_PLACEMENT_3D('',#29257,#12082,#12083);
#10463=AXIS2_PLACEMENT_3D('',#29258,#12084,#12085);
#10464=AXIS2_PLACEMENT_3D('',#29260,#12086,#12087);
#10465=AXIS2_PLACEMENT_3D('',#29263,#12089,#12090);
#10466=AXIS2_PLACEMENT_3D('',#29264,#12091,#12092);
#10467=AXIS2_PLACEMENT_3D('',#29266,#12093,#12094);
#10468=AXIS2_PLACEMENT_3D('',#29267,#12095,#12096);
#10469=AXIS2_PLACEMENT_3D('',#29269,#12097,#12098);
#10470=AXIS2_PLACEMENT_3D('',#29270,#12099,#12100);
#10471=AXIS2_PLACEMENT_3D('',#29272,#12101,#12102);
#10472=AXIS2_PLACEMENT_3D('',#29274,#12104,#12105);
#10473=AXIS2_PLACEMENT_3D('',#29276,#12106,#12107);
#10474=AXIS2_PLACEMENT_3D('',#29278,#12108,#12109);
#10475=AXIS2_PLACEMENT_3D('',#29279,#12110,#12111);
#10476=AXIS2_PLACEMENT_3D('',#29282,#12113,#12114);
#10477=AXIS2_PLACEMENT_3D('',#29283,#12115,#12116);
#10478=AXIS2_PLACEMENT_3D('',#29284,#12117,#12118);
#10479=AXIS2_PLACEMENT_3D('',#29286,#12120,#12121);
#10480=AXIS2_PLACEMENT_3D('',#29287,#12122,#12123);
#10481=AXIS2_PLACEMENT_3D('',#29288,#12124,#12125);
#10482=AXIS2_PLACEMENT_3D('',#29297,#12130,#12131);
#10483=AXIS2_PLACEMENT_3D('',#29306,#12136,#12137);
#10484=AXIS2_PLACEMENT_3D('',#29307,#12138,#12139);
#10485=AXIS2_PLACEMENT_3D('',#29308,#12140,#12141);
#10486=AXIS2_PLACEMENT_3D('',#29309,#12142,#12143);
#10487=AXIS2_PLACEMENT_3D('',#29310,#12144,#12145);
#10488=AXIS2_PLACEMENT_3D('',#29311,#12146,#12147);
#10489=AXIS2_PLACEMENT_3D('',#29312,#12148,#12149);
#10490=AXIS2_PLACEMENT_3D('',#29313,#12150,#12151);
#10491=AXIS2_PLACEMENT_3D('',#29314,#12152,#12153);
#10492=AXIS2_PLACEMENT_3D('',#29606,#12154,#12155);
#10493=AXIS2_PLACEMENT_3D('',#29637,#12156,#12157);
#10494=AXIS2_PLACEMENT_3D('',#29638,#12158,#12159);
#10495=AXIS2_PLACEMENT_3D('',#29639,#12160,#12161);
#10496=AXIS2_PLACEMENT_3D('',#29640,#12162,#12163);
#10497=AXIS2_PLACEMENT_3D('',#29641,#12164,#12165);
#10498=AXIS2_PLACEMENT_3D('',#29643,#12166,#12167);
#10499=AXIS2_PLACEMENT_3D('',#29646,#12169,#12170);
#10500=AXIS2_PLACEMENT_3D('',#29647,#12171,#12172);
#10501=AXIS2_PLACEMENT_3D('',#29649,#12173,#12174);
#10502=AXIS2_PLACEMENT_3D('',#29652,#12176,#12177);
#10503=AXIS2_PLACEMENT_3D('',#29653,#12178,#12179);
#10504=AXIS2_PLACEMENT_3D('',#29654,#12180,#12181);
#10505=AXIS2_PLACEMENT_3D('',#29655,#12182,#12183);
#10506=AXIS2_PLACEMENT_3D('',#29656,#12184,#12185);
#10507=AXIS2_PLACEMENT_3D('',#29672,#12187,#12188);
#10508=AXIS2_PLACEMENT_3D('',#29680,#12189,#12190);
#10509=AXIS2_PLACEMENT_3D('',#29728,#12192,#12193);
#10510=AXIS2_PLACEMENT_3D('',#29776,#12195,#12196);
#10511=AXIS2_PLACEMENT_3D('',#29824,#12198,#12199);
#10512=AXIS2_PLACEMENT_3D('',#29872,#12201,#12202);
#10513=AXIS2_PLACEMENT_3D('',#29920,#12204,#12205);
#10514=AXIS2_PLACEMENT_3D('',#29968,#12207,#12208);
#10515=AXIS2_PLACEMENT_3D('',#30022,#12210,#12211);
#10516=AXIS2_PLACEMENT_3D('',#30070,#12213,#12214);
#10517=AXIS2_PLACEMENT_3D('',#30118,#12216,#12217);
#10518=AXIS2_PLACEMENT_3D('',#30172,#12219,#12220);
#10519=AXIS2_PLACEMENT_3D('',#30220,#12222,#12223);
#10520=AXIS2_PLACEMENT_3D('',#30268,#12225,#12226);
#10521=AXIS2_PLACEMENT_3D('',#30316,#12228,#12229);
#10522=AXIS2_PLACEMENT_3D('',#30367,#12231,#12232);
#10523=AXIS2_PLACEMENT_3D('',#30415,#12234,#12235);
#10524=AXIS2_PLACEMENT_3D('',#30429,#12237,#12238);
#10525=AXIS2_PLACEMENT_3D('',#30437,#12239,#12240);
#10526=AXIS2_PLACEMENT_3D('',#30461,#12242,#12243);
#10527=AXIS2_PLACEMENT_3D('',#30485,#12245,#12246);
#10528=AXIS2_PLACEMENT_3D('',#30511,#12248,#12249);
#10529=AXIS2_PLACEMENT_3D('',#30535,#12251,#12252);
#10530=AXIS2_PLACEMENT_3D('',#30559,#12254,#12255);
#10531=AXIS2_PLACEMENT_3D('',#30584,#12257,#12258);
#10532=AXIS2_PLACEMENT_3D('',#30609,#12260,#12261);
#10533=AXIS2_PLACEMENT_3D('',#30633,#12263,#12264);
#10534=AXIS2_PLACEMENT_3D('',#30658,#12266,#12267);
#10535=AXIS2_PLACEMENT_3D('',#30683,#12269,#12270);
#10536=AXIS2_PLACEMENT_3D('',#30707,#12272,#12273);
#10537=AXIS2_PLACEMENT_3D('',#30731,#12275,#12276);
#10538=AXIS2_PLACEMENT_3D('',#30756,#12278,#12279);
#10539=AXIS2_PLACEMENT_3D('',#30781,#12281,#12282);
#10540=AXIS2_PLACEMENT_3D('',#30805,#12284,#12285);
#10541=AXIS2_PLACEMENT_3D('',#30922,#12286,#12287);
#10542=AXIS2_PLACEMENT_3D('',#30989,#12289,#12290);
#10543=AXIS2_PLACEMENT_3D('',#31494,#12291,#12292);
#10544=AXIS2_PLACEMENT_3D('',#31505,#12293,#12294);
#10545=AXIS2_PLACEMENT_3D('',#32006,#12295,#12296);
#10546=AXIS2_PLACEMENT_3D('',#32007,#12297,#12298);
#10547=AXIS2_PLACEMENT_3D('',#32016,#12303,#12304);
#10548=AXIS2_PLACEMENT_3D('',#32022,#12308,#12309);
#10549=AXIS2_PLACEMENT_3D('',#32028,#12313,#12314);
#10550=AXIS2_PLACEMENT_3D('',#32034,#12318,#12319);
#10551=AXIS2_PLACEMENT_3D('',#32040,#12323,#12324);
#10552=AXIS2_PLACEMENT_3D('',#32043,#12327,#12328);
#10553=AXIS2_PLACEMENT_3D('',#32044,#12329,#12330);
#10554=AXIS2_PLACEMENT_3D('',#32046,#12331,#12332);
#10555=AXIS2_PLACEMENT_3D('',#32047,#12333,#12334);
#10556=AXIS2_PLACEMENT_3D('',#32050,#12336,#12337);
#10557=AXIS2_PLACEMENT_3D('',#32051,#12338,#12339);
#10558=AXIS2_PLACEMENT_3D('',#32052,#12340,#12341);
#10559=AXIS2_PLACEMENT_3D('',#32053,#12342,#12343);
#10560=AXIS2_PLACEMENT_3D('',#32054,#12344,#12345);
#10561=AXIS2_PLACEMENT_3D('',#32070,#12347,#12348);
#10562=AXIS2_PLACEMENT_3D('',#32078,#12349,#12350);
#10563=AXIS2_PLACEMENT_3D('',#32126,#12352,#12353);
#10564=AXIS2_PLACEMENT_3D('',#32174,#12355,#12356);
#10565=AXIS2_PLACEMENT_3D('',#32222,#12358,#12359);
#10566=AXIS2_PLACEMENT_3D('',#32276,#12361,#12362);
#10567=AXIS2_PLACEMENT_3D('',#32324,#12364,#12365);
#10568=AXIS2_PLACEMENT_3D('',#32372,#12367,#12368);
#10569=AXIS2_PLACEMENT_3D('',#32426,#12370,#12371);
#10570=AXIS2_PLACEMENT_3D('',#32474,#12373,#12374);
#10571=AXIS2_PLACEMENT_3D('',#32522,#12376,#12377);
#10572=AXIS2_PLACEMENT_3D('',#32538,#12379,#12380);
#10573=AXIS2_PLACEMENT_3D('',#32548,#12381,#12382);
#10574=AXIS2_PLACEMENT_3D('',#32572,#12384,#12385);
#10575=AXIS2_PLACEMENT_3D('',#32596,#12387,#12388);
#10576=AXIS2_PLACEMENT_3D('',#32621,#12390,#12391);
#10577=AXIS2_PLACEMENT_3D('',#32646,#12393,#12394);
#10578=AXIS2_PLACEMENT_3D('',#32670,#12396,#12397);
#10579=AXIS2_PLACEMENT_3D('',#32695,#12399,#12400);
#10580=AXIS2_PLACEMENT_3D('',#32720,#12402,#12403);
#10581=AXIS2_PLACEMENT_3D('',#32744,#12405,#12406);
#10582=AXIS2_PLACEMENT_3D('',#32768,#12408,#12409);
#10583=AXIS2_PLACEMENT_3D('',#32933,#12410,#12411);
#10584=AXIS2_PLACEMENT_3D('',#32952,#12413,#12414);
#10585=AXIS2_PLACEMENT_3D('',#33310,#12415,#12416);
#10586=AXIS2_PLACEMENT_3D('',#33321,#12417,#12418);
#10587=AXIS2_PLACEMENT_3D('',#33684,#12419,#12420);
#10588=AXIS2_PLACEMENT_3D('',#33685,#12421,#12422);
#10589=AXIS2_PLACEMENT_3D('',#33694,#12427,#12428);
#10590=AXIS2_PLACEMENT_3D('',#33700,#12432,#12433);
#10591=AXIS2_PLACEMENT_3D('',#33706,#12437,#12438);
#10592=AXIS2_PLACEMENT_3D('',#33712,#12442,#12443);
#10593=AXIS2_PLACEMENT_3D('',#33718,#12447,#12448);
#10594=AXIS2_PLACEMENT_3D('',#33721,#12451,#12452);
#10595=AXIS2_PLACEMENT_3D('',#33722,#12453,#12454);
#10596=AXIS2_PLACEMENT_3D('',#33724,#12455,#12456);
#10597=AXIS2_PLACEMENT_3D('',#33725,#12457,#12458);
#10598=AXIS2_PLACEMENT_3D('',#33728,#12460,#12461);
#10599=AXIS2_PLACEMENT_3D('',#33729,#12462,#12463);
#10600=AXIS2_PLACEMENT_3D('',#33730,#12464,#12465);
#10601=AXIS2_PLACEMENT_3D('',#33731,#12466,#12467);
#10602=AXIS2_PLACEMENT_3D('',#33732,#12468,#12469);
#10603=AXIS2_PLACEMENT_3D('',#33748,#12471,#12472);
#10604=AXIS2_PLACEMENT_3D('',#33756,#12473,#12474);
#10605=AXIS2_PLACEMENT_3D('',#33804,#12476,#12477);
#10606=AXIS2_PLACEMENT_3D('',#33852,#12479,#12480);
#10607=AXIS2_PLACEMENT_3D('',#33906,#12482,#12483);
#10608=AXIS2_PLACEMENT_3D('',#33954,#12485,#12486);
#10609=AXIS2_PLACEMENT_3D('',#34002,#12488,#12489);
#10610=AXIS2_PLACEMENT_3D('',#34056,#12491,#12492);
#10611=AXIS2_PLACEMENT_3D('',#34104,#12494,#12495);
#10612=AXIS2_PLACEMENT_3D('',#34152,#12497,#12498);
#10613=AXIS2_PLACEMENT_3D('',#34206,#12500,#12501);
#10614=AXIS2_PLACEMENT_3D('',#34254,#12503,#12504);
#10615=AXIS2_PLACEMENT_3D('',#34302,#12506,#12507);
#10616=AXIS2_PLACEMENT_3D('',#34356,#12509,#12510);
#10617=AXIS2_PLACEMENT_3D('',#34404,#12512,#12513);
#10618=AXIS2_PLACEMENT_3D('',#34452,#12515,#12516);
#10619=AXIS2_PLACEMENT_3D('',#34503,#12518,#12519);
#10620=AXIS2_PLACEMENT_3D('',#34551,#12521,#12522);
#10621=AXIS2_PLACEMENT_3D('',#34599,#12524,#12525);
#10622=AXIS2_PLACEMENT_3D('',#34615,#12527,#12528);
#10623=AXIS2_PLACEMENT_3D('',#34625,#12529,#12530);
#10624=AXIS2_PLACEMENT_3D('',#34649,#12532,#12533);
#10625=AXIS2_PLACEMENT_3D('',#34673,#12535,#12536);
#10626=AXIS2_PLACEMENT_3D('',#34699,#12538,#12539);
#10627=AXIS2_PLACEMENT_3D('',#34723,#12541,#12542);
#10628=AXIS2_PLACEMENT_3D('',#34747,#12544,#12545);
#10629=AXIS2_PLACEMENT_3D('',#34772,#12547,#12548);
#10630=AXIS2_PLACEMENT_3D('',#34797,#12550,#12551);
#10631=AXIS2_PLACEMENT_3D('',#34821,#12553,#12554);
#10632=AXIS2_PLACEMENT_3D('',#34846,#12556,#12557);
#10633=AXIS2_PLACEMENT_3D('',#34871,#12559,#12560);
#10634=AXIS2_PLACEMENT_3D('',#34895,#12562,#12563);
#10635=AXIS2_PLACEMENT_3D('',#34920,#12565,#12566);
#10636=AXIS2_PLACEMENT_3D('',#34945,#12568,#12569);
#10637=AXIS2_PLACEMENT_3D('',#34969,#12571,#12572);
#10638=AXIS2_PLACEMENT_3D('',#34994,#12574,#12575);
#10639=AXIS2_PLACEMENT_3D('',#35019,#12577,#12578);
#10640=AXIS2_PLACEMENT_3D('',#35043,#12580,#12581);
#10641=AXIS2_PLACEMENT_3D('',#35202,#12582,#12583);
#10642=AXIS2_PLACEMENT_3D('',#35221,#12585,#12586);
#10643=AXIS2_PLACEMENT_3D('',#35789,#12587,#12588);
#10644=AXIS2_PLACEMENT_3D('',#35800,#12589,#12590);
#10645=AXIS2_PLACEMENT_3D('',#36367,#12591,#12592);
#10646=AXIS2_PLACEMENT_3D('',#36368,#12593,#12594);
#10647=AXIS2_PLACEMENT_3D('',#36377,#12599,#12600);
#10648=AXIS2_PLACEMENT_3D('',#36383,#12604,#12605);
#10649=AXIS2_PLACEMENT_3D('',#36389,#12609,#12610);
#10650=AXIS2_PLACEMENT_3D('',#36395,#12614,#12615);
#10651=AXIS2_PLACEMENT_3D('',#36401,#12619,#12620);
#10652=AXIS2_PLACEMENT_3D('',#36404,#12623,#12624);
#10653=AXIS2_PLACEMENT_3D('',#36405,#12625,#12626);
#10654=AXIS2_PLACEMENT_3D('',#36407,#12627,#12628);
#10655=AXIS2_PLACEMENT_3D('',#36408,#12629,#12630);
#10656=AXIS2_PLACEMENT_3D('',#36411,#12632,#12633);
#10657=AXIS2_PLACEMENT_3D('',#36412,#12634,#12635);
#10658=AXIS2_PLACEMENT_3D('',#36413,#12636,#12637);
#10659=AXIS2_PLACEMENT_3D('',#36414,#12638,#12639);
#10660=AXIS2_PLACEMENT_3D('',#36415,#12640,#12641);
#10661=AXIS2_PLACEMENT_3D('',#36416,#12642,#12643);
#10662=AXIS2_PLACEMENT_3D('',#36417,#12644,#12645);
#10663=AXIS2_PLACEMENT_3D('',#36418,#12646,#12647);
#10664=AXIS2_PLACEMENT_3D('',#36419,#12648,#12649);
#10665=AXIS2_PLACEMENT_3D('',#36420,#12650,#12651);
#10666=AXIS2_PLACEMENT_3D('',#36421,#12652,#12653);
#10667=AXIS2_PLACEMENT_3D('',#36422,#12654,#12655);
#10668=AXIS2_PLACEMENT_3D('',#36423,#12656,#12657);
#10669=AXIS2_PLACEMENT_3D('',#36424,#12658,#12659);
#10670=AXIS2_PLACEMENT_3D('',#36425,#12660,#12661);
#10671=AXIS2_PLACEMENT_3D('',#36426,#12662,#12663);
#10672=AXIS2_PLACEMENT_3D('',#36427,#12664,#12665);
#10673=AXIS2_PLACEMENT_3D('',#36428,#12666,#12667);
#10674=AXIS2_PLACEMENT_3D('',#36429,#12668,#12669);
#10675=AXIS2_PLACEMENT_3D('',#36430,#12670,#12671);
#10676=AXIS2_PLACEMENT_3D('',#36431,#12672,#12673);
#10677=AXIS2_PLACEMENT_3D('',#36432,#12674,#12675);
#10678=AXIS2_PLACEMENT_3D('',#36433,#12676,#12677);
#10679=AXIS2_PLACEMENT_3D('',#36434,#12678,#12679);
#10680=AXIS2_PLACEMENT_3D('',#36435,#12680,#12681);
#10681=AXIS2_PLACEMENT_3D('',#36436,#12682,#12683);
#10682=AXIS2_PLACEMENT_3D('',#36437,#12684,#12685);
#10683=AXIS2_PLACEMENT_3D('',#36438,#12686,#12687);
#10684=AXIS2_PLACEMENT_3D('',#36439,#12688,#12689);
#10685=AXIS2_PLACEMENT_3D('',#36440,#12690,#12691);
#10686=AXIS2_PLACEMENT_3D('',#36441,#12692,#12693);
#10687=AXIS2_PLACEMENT_3D('',#36442,#12694,#12695);
#10688=AXIS2_PLACEMENT_3D('',#36443,#12696,#12697);
#10689=AXIS2_PLACEMENT_3D('',#36444,#12698,#12699);
#10690=DIRECTION('axis',(0.,0.,1.));
#10691=DIRECTION('refdir',(1.,0.,0.));
#10692=DIRECTION('axis',(0.,0.,1.));
#10693=DIRECTION('refdir',(1.,0.,0.));
#10694=DIRECTION('center_axis',(0.,0.,-1.));
#10695=DIRECTION('ref_axis',(1.,0.,0.));
#10696=DIRECTION('',(0.,0.,-1.));
#10697=DIRECTION('center_axis',(0.,0.,1.));
#10698=DIRECTION('ref_axis',(1.,0.,0.));
#10699=DIRECTION('',(0.,0.,-1.));
#10700=DIRECTION('center_axis',(0.,0.,1.));
#10701=DIRECTION('ref_axis',(1.,0.,0.));
#10702=DIRECTION('center_axis',(0.,0.,-1.));
#10703=DIRECTION('ref_axis',(1.,0.,0.));
#10704=DIRECTION('',(0.,0.,-1.));
#10705=DIRECTION('center_axis',(0.,0.,-1.));
#10706=DIRECTION('ref_axis',(1.,0.,0.));
#10707=DIRECTION('',(0.,0.,-1.));
#10708=DIRECTION('center_axis',(0.,0.,-1.));
#10709=DIRECTION('ref_axis',(1.,0.,0.));
#10710=DIRECTION('',(0.,0.,-1.));
#10711=DIRECTION('center_axis',(0.,0.,-1.));
#10712=DIRECTION('ref_axis',(1.,0.,0.));
#10713=DIRECTION('',(0.,0.,-1.));
#10714=DIRECTION('center_axis',(0.,0.,-1.));
#10715=DIRECTION('ref_axis',(1.,0.,0.));
#10716=DIRECTION('',(0.,0.,-1.));
#10717=DIRECTION('center_axis',(0.,0.,-1.));
#10718=DIRECTION('ref_axis',(1.,0.,0.));
#10719=DIRECTION('',(0.,0.,-1.));
#10720=DIRECTION('center_axis',(0.,0.,-1.));
#10721=DIRECTION('ref_axis',(1.,0.,0.));
#10722=DIRECTION('',(0.,0.,-1.));
#10723=DIRECTION('center_axis',(0.,0.,-1.));
#10724=DIRECTION('ref_axis',(1.,0.,0.));
#10725=DIRECTION('',(0.,0.,-1.));
#10726=DIRECTION('center_axis',(0.,0.,-1.));
#10727=DIRECTION('ref_axis',(1.,0.,0.));
#10728=DIRECTION('',(0.,0.,-1.));
#10729=DIRECTION('center_axis',(0.,0.,-1.));
#10730=DIRECTION('ref_axis',(1.,0.,0.));
#10731=DIRECTION('',(0.,0.,-1.));
#10732=DIRECTION('center_axis',(0.,0.,-1.));
#10733=DIRECTION('ref_axis',(0.938438601292299,-0.345446076261625,0.));
#10734=DIRECTION('',(0.,0.,-1.));
#10735=DIRECTION('center_axis',(0.,0.,-1.));
#10736=DIRECTION('ref_axis',(1.,0.,0.));
#10737=DIRECTION('center_axis',(0.,0.,-1.));
#10738=DIRECTION('ref_axis',(0.450153040552508,0.892951420896642,0.));
#10739=DIRECTION('',(1.22464679914735E-16,-7.42605394171526E-30,-1.));
#10740=DIRECTION('center_axis',(0.,0.,1.));
#10741=DIRECTION('ref_axis',(1.,-6.05158675060312E-14,0.));
#10742=DIRECTION('center_axis',(0.,0.,-1.));
#10743=DIRECTION('ref_axis',(1.,-6.05158675060312E-14,0.));
#10744=DIRECTION('',(1.22464679914735E-16,-7.42605394171526E-30,-1.));
#10745=DIRECTION('center_axis',(0.,0.,-1.));
#10746=DIRECTION('ref_axis',(1.,-6.05158675060312E-14,0.));
#10747=DIRECTION('',(1.22464679914735E-16,-7.42605394171526E-30,-1.));
#10748=DIRECTION('center_axis',(0.,0.,-1.));
#10749=DIRECTION('ref_axis',(1.,-6.05158675060312E-14,0.));
#10750=DIRECTION('',(1.22464679914735E-16,-7.42605394171526E-30,-1.));
#10751=DIRECTION('center_axis',(0.,0.,-1.));
#10752=DIRECTION('ref_axis',(1.,-6.05158675060312E-14,0.));
#10753=DIRECTION('',(1.22464679914735E-16,-7.42605394171526E-30,-1.));
#10754=DIRECTION('center_axis',(0.,0.,-1.));
#10755=DIRECTION('ref_axis',(1.,-6.05158675060312E-14,0.));
#10756=DIRECTION('',(1.22464679914735E-16,-7.42605394171526E-30,-1.));
#10757=DIRECTION('center_axis',(0.,0.,-1.));
#10758=DIRECTION('ref_axis',(1.,-6.05158675060312E-14,0.));
#10759=DIRECTION('',(1.22464679914735E-16,-7.42605394171526E-30,-1.));
#10760=DIRECTION('center_axis',(0.,0.,-1.));
#10761=DIRECTION('ref_axis',(1.,-6.05158675060312E-14,0.));
#10762=DIRECTION('',(1.22464679914735E-16,-7.42605394171526E-30,-1.));
#10763=DIRECTION('center_axis',(0.,0.,-1.));
#10764=DIRECTION('ref_axis',(1.,-6.05158675060312E-14,0.));
#10765=DIRECTION('',(1.22464679914735E-16,-7.42605394171526E-30,-1.));
#10766=DIRECTION('center_axis',(0.,0.,-1.));
#10767=DIRECTION('ref_axis',(1.,-6.05158675060312E-14,0.));
#10768=DIRECTION('',(1.22464679914735E-16,-7.42605394171526E-30,-1.));
#10769=DIRECTION('center_axis',(0.,0.,-1.));
#10770=DIRECTION('ref_axis',(1.,-6.05158675060312E-14,0.));
#10771=DIRECTION('',(1.22464679914735E-16,-7.42605394171526E-30,-1.));
#10772=DIRECTION('center_axis',(0.,0.,-1.));
#10773=DIRECTION('ref_axis',(1.,-6.05158675060312E-14,0.));
#10774=DIRECTION('',(1.22464679914735E-16,-7.42605394171526E-30,-1.));
#10775=DIRECTION('center_axis',(0.,0.,-1.));
#10776=DIRECTION('ref_axis',(-0.609341503082739,-0.792907896682123,0.));
#10777=DIRECTION('',(1.22464679914735E-16,-7.42605394171526E-30,-1.));
#10778=DIRECTION('center_axis',(0.,0.,-1.));
#10779=DIRECTION('ref_axis',(1.,-6.05158675060312E-14,0.));
#10780=DIRECTION('center_axis',(0.,0.,-1.));
#10781=DIRECTION('ref_axis',(1.,0.,0.));
#10782=DIRECTION('',(0.,0.,-1.));
#10783=DIRECTION('center_axis',(0.,0.,1.));
#10784=DIRECTION('ref_axis',(1.,0.,0.));
#10785=DIRECTION('',(0.,0.,-1.));
#10786=DIRECTION('center_axis',(0.,0.,1.));
#10787=DIRECTION('ref_axis',(1.,0.,0.));
#10788=DIRECTION('center_axis',(0.,0.,-1.));
#10789=DIRECTION('ref_axis',(1.,0.,0.));
#10790=DIRECTION('',(0.,0.,-1.));
#10791=DIRECTION('center_axis',(0.,0.,-1.));
#10792=DIRECTION('ref_axis',(1.,0.,0.));
#10793=DIRECTION('',(0.,0.,-1.));
#10794=DIRECTION('center_axis',(0.,0.,-1.));
#10795=DIRECTION('ref_axis',(1.,0.,0.));
#10796=DIRECTION('',(0.,0.,-1.));
#10797=DIRECTION('center_axis',(0.,0.,-1.));
#10798=DIRECTION('ref_axis',(1.,0.,0.));
#10799=DIRECTION('',(0.,0.,-1.));
#10800=DIRECTION('center_axis',(0.,0.,-1.));
#10801=DIRECTION('ref_axis',(1.,0.,0.));
#10802=DIRECTION('',(0.,0.,-1.));
#10803=DIRECTION('center_axis',(0.,0.,-1.));
#10804=DIRECTION('ref_axis',(1.,0.,0.));
#10805=DIRECTION('',(0.,0.,-1.));
#10806=DIRECTION('center_axis',(0.,0.,-1.));
#10807=DIRECTION('ref_axis',(1.,0.,0.));
#10808=DIRECTION('',(0.,0.,-1.));
#10809=DIRECTION('center_axis',(0.,0.,-1.));
#10810=DIRECTION('ref_axis',(1.,0.,0.));
#10811=DIRECTION('',(0.,0.,-1.));
#10812=DIRECTION('center_axis',(0.,0.,-1.));
#10813=DIRECTION('ref_axis',(1.,0.,0.));
#10814=DIRECTION('',(0.,0.,-1.));
#10815=DIRECTION('center_axis',(0.,0.,-1.));
#10816=DIRECTION('ref_axis',(1.,0.,0.));
#10817=DIRECTION('',(0.,0.,-1.));
#10818=DIRECTION('center_axis',(0.,0.,-1.));
#10819=DIRECTION('ref_axis',(0.938438595705222,-0.345446091439475,0.));
#10820=DIRECTION('',(0.,0.,-1.));
#10821=DIRECTION('center_axis',(0.,0.,-1.));
#10822=DIRECTION('ref_axis',(1.,0.,0.));
#10823=DIRECTION('center_axis',(0.,0.,-1.));
#10824=DIRECTION('ref_axis',(0.450153019553355,0.892951431482697,0.));
#10825=DIRECTION('',(1.22464679914735E-16,-6.89669277429462E-30,-1.));
#10826=DIRECTION('center_axis',(0.,0.,1.));
#10827=DIRECTION('ref_axis',(1.,-5.61933055413145E-14,0.));
#10828=DIRECTION('center_axis',(0.,0.,-1.));
#10829=DIRECTION('ref_axis',(1.,-5.61933055413145E-14,0.));
#10830=DIRECTION('',(1.22464679914735E-16,-6.89669277429462E-30,-1.));
#10831=DIRECTION('center_axis',(0.,0.,-1.));
#10832=DIRECTION('ref_axis',(1.,-5.61933055413145E-14,0.));
#10833=DIRECTION('',(1.22464679914735E-16,-6.89669277429462E-30,-1.));
#10834=DIRECTION('center_axis',(0.,0.,-1.));
#10835=DIRECTION('ref_axis',(1.,-5.61933055413145E-14,0.));
#10836=DIRECTION('',(1.22464679914735E-16,-6.89669277429462E-30,-1.));
#10837=DIRECTION('center_axis',(0.,0.,-1.));
#10838=DIRECTION('ref_axis',(1.,-5.61933055413145E-14,0.));
#10839=DIRECTION('',(1.22464679914735E-16,-6.89669277429462E-30,-1.));
#10840=DIRECTION('center_axis',(0.,0.,-1.));
#10841=DIRECTION('ref_axis',(1.,-5.61933055413145E-14,0.));
#10842=DIRECTION('',(1.22464679914735E-16,-6.89669277429462E-30,-1.));
#10843=DIRECTION('center_axis',(0.,0.,-1.));
#10844=DIRECTION('ref_axis',(1.,-5.61933055413145E-14,0.));
#10845=DIRECTION('',(1.22464679914735E-16,-6.89669277429462E-30,-1.));
#10846=DIRECTION('center_axis',(0.,0.,-1.));
#10847=DIRECTION('ref_axis',(1.,-5.61933055413145E-14,0.));
#10848=DIRECTION('',(1.22464679914735E-16,-6.89669277429462E-30,-1.));
#10849=DIRECTION('center_axis',(0.,0.,-1.));
#10850=DIRECTION('ref_axis',(1.,-5.61933055413145E-14,0.));
#10851=DIRECTION('',(1.22464679914735E-16,-6.89669277429462E-30,-1.));
#10852=DIRECTION('center_axis',(0.,0.,-1.));
#10853=DIRECTION('ref_axis',(1.,-5.61933055413145E-14,0.));
#10854=DIRECTION('',(1.22464679914735E-16,-6.89669277429462E-30,-1.));
#10855=DIRECTION('center_axis',(0.,0.,-1.));
#10856=DIRECTION('ref_axis',(1.,-5.61933055413145E-14,0.));
#10857=DIRECTION('',(1.22464679914735E-16,-6.89669277429462E-30,-1.));
#10858=DIRECTION('center_axis',(0.,0.,-1.));
#10859=DIRECTION('ref_axis',(1.,-5.61933055413145E-14,0.));
#10860=DIRECTION('',(1.22464679914735E-16,-6.89669277429462E-30,-1.));
#10861=DIRECTION('center_axis',(0.,0.,-1.));
#10862=DIRECTION('ref_axis',(-0.609341511570002,-0.792907890159749,0.));
#10863=DIRECTION('',(1.22464679914735E-16,-6.89669277429462E-30,-1.));
#10864=DIRECTION('center_axis',(0.,0.,-1.));
#10865=DIRECTION('ref_axis',(1.,-5.61933055413145E-14,0.));
#10866=DIRECTION('center_axis',(0.,0.,-1.));
#10867=DIRECTION('ref_axis',(1.,0.,0.));
#10868=DIRECTION('',(0.,0.,-1.));
#10869=DIRECTION('center_axis',(0.,0.,1.));
#10870=DIRECTION('ref_axis',(1.,0.,0.));
#10871=DIRECTION('',(0.,0.,-1.));
#10872=DIRECTION('center_axis',(0.,0.,1.));
#10873=DIRECTION('ref_axis',(1.,0.,0.));
#10874=DIRECTION('center_axis',(0.,0.,-1.));
#10875=DIRECTION('ref_axis',(1.,0.,0.));
#10876=DIRECTION('',(0.,0.,-1.));
#10877=DIRECTION('center_axis',(0.,0.,-1.));
#10878=DIRECTION('ref_axis',(1.,0.,0.));
#10879=DIRECTION('',(0.,0.,-1.));
#10880=DIRECTION('center_axis',(0.,0.,-1.));
#10881=DIRECTION('ref_axis',(1.,0.,0.));
#10882=DIRECTION('',(0.,0.,-1.));
#10883=DIRECTION('center_axis',(0.,0.,-1.));
#10884=DIRECTION('ref_axis',(1.,0.,0.));
#10885=DIRECTION('',(0.,0.,-1.));
#10886=DIRECTION('center_axis',(0.,0.,-1.));
#10887=DIRECTION('ref_axis',(1.,0.,0.));
#10888=DIRECTION('',(0.,0.,-1.));
#10889=DIRECTION('center_axis',(0.,0.,-1.));
#10890=DIRECTION('ref_axis',(1.,0.,0.));
#10891=DIRECTION('',(0.,0.,-1.));
#10892=DIRECTION('center_axis',(0.,0.,-1.));
#10893=DIRECTION('ref_axis',(1.,0.,0.));
#10894=DIRECTION('',(0.,0.,-1.));
#10895=DIRECTION('center_axis',(0.,0.,-1.));
#10896=DIRECTION('ref_axis',(1.,0.,0.));
#10897=DIRECTION('',(0.,0.,-1.));
#10898=DIRECTION('center_axis',(0.,0.,-1.));
#10899=DIRECTION('ref_axis',(1.,0.,0.));
#10900=DIRECTION('',(0.,0.,-1.));
#10901=DIRECTION('center_axis',(0.,0.,-1.));
#10902=DIRECTION('ref_axis',(1.,0.,0.));
#10903=DIRECTION('',(0.,0.,-1.));
#10904=DIRECTION('center_axis',(0.,0.,-1.));
#10905=DIRECTION('ref_axis',(0.938438617144983,-0.345446033196231,0.));
#10906=DIRECTION('',(0.,0.,-1.));
#10907=DIRECTION('center_axis',(0.,0.,-1.));
#10908=DIRECTION('ref_axis',(1.,0.,0.));
#10909=DIRECTION('center_axis',(0.,0.,-1.));
#10910=DIRECTION('ref_axis',(0.450153067737633,0.892951407192126,0.));
#10911=DIRECTION('',(1.22464679914735E-16,-6.89669277429462E-30,-1.));
#10912=DIRECTION('center_axis',(0.,0.,1.));
#10913=DIRECTION('ref_axis',(1.,-5.61933055413145E-14,0.));
#10914=DIRECTION('center_axis',(0.,0.,-1.));
#10915=DIRECTION('ref_axis',(1.,-5.61933055413145E-14,0.));
#10916=DIRECTION('',(1.22464679914735E-16,-6.89669277429462E-30,-1.));
#10917=DIRECTION('center_axis',(0.,0.,-1.));
#10918=DIRECTION('ref_axis',(1.,-5.61933055413145E-14,0.));
#10919=DIRECTION('',(1.22464679914735E-16,-6.89669277429462E-30,-1.));
#10920=DIRECTION('center_axis',(0.,0.,-1.));
#10921=DIRECTION('ref_axis',(1.,-5.61933055413145E-14,0.));
#10922=DIRECTION('',(1.22464679914735E-16,-6.89669277429462E-30,-1.));
#10923=DIRECTION('center_axis',(0.,0.,-1.));
#10924=DIRECTION('ref_axis',(1.,-5.61933055413145E-14,0.));
#10925=DIRECTION('',(1.22464679914735E-16,-6.89669277429462E-30,-1.));
#10926=DIRECTION('center_axis',(0.,0.,-1.));
#10927=DIRECTION('ref_axis',(1.,-5.61933055413145E-14,0.));
#10928=DIRECTION('',(1.22464679914735E-16,-6.89669277429462E-30,-1.));
#10929=DIRECTION('center_axis',(0.,0.,-1.));
#10930=DIRECTION('ref_axis',(1.,-5.61933055413145E-14,0.));
#10931=DIRECTION('',(1.22464679914735E-16,-6.89669277429462E-30,-1.));
#10932=DIRECTION('center_axis',(0.,0.,-1.));
#10933=DIRECTION('ref_axis',(1.,-5.61933055413145E-14,0.));
#10934=DIRECTION('',(1.22464679914735E-16,-6.89669277429462E-30,-1.));
#10935=DIRECTION('center_axis',(0.,0.,-1.));
#10936=DIRECTION('ref_axis',(1.,-5.61933055413145E-14,0.));
#10937=DIRECTION('',(1.22464679914735E-16,-6.89669277429462E-30,-1.));
#10938=DIRECTION('center_axis',(0.,0.,-1.));
#10939=DIRECTION('ref_axis',(1.,-5.61933055413145E-14,0.));
#10940=DIRECTION('',(1.22464679914735E-16,-6.89669277429462E-30,-1.));
#10941=DIRECTION('center_axis',(0.,0.,-1.));
#10942=DIRECTION('ref_axis',(1.,-5.61933055413145E-14,0.));
#10943=DIRECTION('',(1.22464679914735E-16,-6.89669277429462E-30,-1.));
#10944=DIRECTION('center_axis',(0.,0.,-1.));
#10945=DIRECTION('ref_axis',(1.,-5.61933055413145E-14,0.));
#10946=DIRECTION('',(1.22464679914735E-16,-6.89669277429462E-30,-1.));
#10947=DIRECTION('center_axis',(0.,0.,-1.));
#10948=DIRECTION('ref_axis',(-0.609341520949359,-0.79290788295181,0.));
#10949=DIRECTION('',(1.22464679914735E-16,-6.89669277429462E-30,-1.));
#10950=DIRECTION('center_axis',(0.,0.,-1.));
#10951=DIRECTION('ref_axis',(1.,-5.61933055413145E-14,0.));
#10952=DIRECTION('center_axis',(0.,0.,-1.));
#10953=DIRECTION('ref_axis',(1.,0.,0.));
#10954=DIRECTION('',(0.,0.,-1.));
#10955=DIRECTION('center_axis',(0.,0.,1.));
#10956=DIRECTION('ref_axis',(1.,0.,0.));
#10957=DIRECTION('',(0.,0.,-1.));
#10958=DIRECTION('center_axis',(0.,0.,1.));
#10959=DIRECTION('ref_axis',(1.,0.,0.));
#10960=DIRECTION('center_axis',(0.,0.,-1.));
#10961=DIRECTION('ref_axis',(1.,0.,0.));
#10962=DIRECTION('',(0.,0.,-1.));
#10963=DIRECTION('center_axis',(0.,0.,-1.));
#10964=DIRECTION('ref_axis',(1.,0.,0.));
#10965=DIRECTION('',(0.,0.,-1.));
#10966=DIRECTION('center_axis',(0.,0.,-1.));
#10967=DIRECTION('ref_axis',(1.,0.,0.));
#10968=DIRECTION('',(0.,0.,-1.));
#10969=DIRECTION('center_axis',(0.,0.,-1.));
#10970=DIRECTION('ref_axis',(1.,0.,0.));
#10971=DIRECTION('',(0.,0.,-1.));
#10972=DIRECTION('center_axis',(0.,0.,-1.));
#10973=DIRECTION('ref_axis',(1.,0.,0.));
#10974=DIRECTION('',(0.,0.,-1.));
#10975=DIRECTION('center_axis',(0.,0.,-1.));
#10976=DIRECTION('ref_axis',(1.,0.,0.));
#10977=DIRECTION('',(0.,0.,-1.));
#10978=DIRECTION('center_axis',(0.,0.,-1.));
#10979=DIRECTION('ref_axis',(1.,0.,0.));
#10980=DIRECTION('',(0.,0.,-1.));
#10981=DIRECTION('center_axis',(0.,0.,-1.));
#10982=DIRECTION('ref_axis',(1.,0.,0.));
#10983=DIRECTION('',(0.,0.,-1.));
#10984=DIRECTION('center_axis',(0.,0.,-1.));
#10985=DIRECTION('ref_axis',(1.,0.,0.));
#10986=DIRECTION('',(0.,0.,-1.));
#10987=DIRECTION('center_axis',(0.,0.,-1.));
#10988=DIRECTION('ref_axis',(1.,0.,0.));
#10989=DIRECTION('',(0.,0.,-1.));
#10990=DIRECTION('center_axis',(0.,0.,-1.));
#10991=DIRECTION('ref_axis',(0.938438612980319,-0.345446044509957,0.));
#10992=DIRECTION('',(0.,0.,-1.));
#10993=DIRECTION('center_axis',(0.,0.,-1.));
#10994=DIRECTION('ref_axis',(1.,0.,0.));
#10995=DIRECTION('center_axis',(0.,0.,-1.));
#10996=DIRECTION('ref_axis',(0.450153049056661,0.892951416609544,0.));
#10997=DIRECTION('',(1.22464679914735E-16,-7.42605394171526E-30,-1.));
#10998=DIRECTION('center_axis',(0.,0.,1.));
#10999=DIRECTION('ref_axis',(1.,-6.05158675060312E-14,0.));
#11000=DIRECTION('center_axis',(0.,0.,-1.));
#11001=DIRECTION('ref_axis',(1.,-6.05158675060312E-14,0.));
#11002=DIRECTION('',(1.22464679914735E-16,-7.42605394171526E-30,-1.));
#11003=DIRECTION('center_axis',(0.,0.,-1.));
#11004=DIRECTION('ref_axis',(1.,-6.05158675060312E-14,0.));
#11005=DIRECTION('',(1.22464679914735E-16,-7.42605394171526E-30,-1.));
#11006=DIRECTION('center_axis',(0.,0.,-1.));
#11007=DIRECTION('ref_axis',(1.,-6.05158675060312E-14,0.));
#11008=DIRECTION('',(1.22464679914735E-16,-7.42605394171526E-30,-1.));
#11009=DIRECTION('center_axis',(0.,0.,-1.));
#11010=DIRECTION('ref_axis',(1.,-6.05158675060312E-14,0.));
#11011=DIRECTION('',(1.22464679914735E-16,-7.42605394171526E-30,-1.));
#11012=DIRECTION('center_axis',(0.,0.,-1.));
#11013=DIRECTION('ref_axis',(1.,-6.05158675060312E-14,0.));
#11014=DIRECTION('',(1.22464679914735E-16,-7.42605394171526E-30,-1.));
#11015=DIRECTION('center_axis',(0.,0.,-1.));
#11016=DIRECTION('ref_axis',(1.,-6.05158675060312E-14,0.));
#11017=DIRECTION('',(1.22464679914735E-16,-7.42605394171526E-30,-1.));
#11018=DIRECTION('center_axis',(0.,0.,-1.));
#11019=DIRECTION('ref_axis',(1.,-6.05158675060312E-14,0.));
#11020=DIRECTION('',(1.22464679914735E-16,-7.42605394171526E-30,-1.));
#11021=DIRECTION('center_axis',(0.,0.,-1.));
#11022=DIRECTION('ref_axis',(1.,-6.05158675060312E-14,0.));
#11023=DIRECTION('',(1.22464679914735E-16,-7.42605394171526E-30,-1.));
#11024=DIRECTION('center_axis',(0.,0.,-1.));
#11025=DIRECTION('ref_axis',(1.,-6.05158675060312E-14,0.));
#11026=DIRECTION('',(1.22464679914735E-16,-7.42605394171526E-30,-1.));
#11027=DIRECTION('center_axis',(0.,0.,-1.));
#11028=DIRECTION('ref_axis',(1.,-6.05158675060312E-14,0.));
#11029=DIRECTION('',(1.22464679914735E-16,-7.42605394171526E-30,-1.));
#11030=DIRECTION('center_axis',(0.,0.,-1.));
#11031=DIRECTION('ref_axis',(1.,-6.05158675060312E-14,0.));
#11032=DIRECTION('',(1.22464679914735E-16,-7.42605394171526E-30,-1.));
#11033=DIRECTION('center_axis',(0.,0.,-1.));
#11034=DIRECTION('ref_axis',(-0.609341531225801,-0.792907875054471,0.));
#11035=DIRECTION('',(1.22464679914735E-16,-7.42605394171526E-30,-1.));
#11036=DIRECTION('center_axis',(0.,0.,-1.));
#11037=DIRECTION('ref_axis',(1.,-6.05158675060312E-14,0.));
#11038=DIRECTION('center_axis',(0.,0.,-1.));
#11039=DIRECTION('ref_axis',(-0.707106781186547,0.707106781186547,0.));
#11040=DIRECTION('center_axis',(0.,0.,1.));
#11041=DIRECTION('ref_axis',(-0.707106781186547,0.707106781186547,0.));
#11042=DIRECTION('',(0.,0.,1.));
#11043=DIRECTION('center_axis',(0.,0.,1.));
#11044=DIRECTION('ref_axis',(-0.707106781186547,0.707106781186547,0.));
#11045=DIRECTION('',(0.,0.,-1.));
#11046=DIRECTION('center_axis',(0.,1.,0.));
#11047=DIRECTION('ref_axis',(1.,0.,0.));
#11048=DIRECTION('',(1.,0.,0.));
#11049=DIRECTION('',(0.,0.,-1.));
#11050=DIRECTION('',(1.,0.,0.));
#11051=DIRECTION('center_axis',(0.,0.,-1.));
#11052=DIRECTION('ref_axis',(0.707106781186548,0.707106781186547,0.));
#11053=DIRECTION('center_axis',(0.,0.,1.));
#11054=DIRECTION('ref_axis',(0.707106781186548,0.707106781186547,0.));
#11055=DIRECTION('',(0.,0.,1.));
#11056=DIRECTION('center_axis',(0.,0.,1.));
#11057=DIRECTION('ref_axis',(0.707106781186548,0.707106781186547,0.));
#11058=DIRECTION('center_axis',(1.,0.,0.));
#11059=DIRECTION('ref_axis',(0.,-1.,0.));
#11060=DIRECTION('',(0.,-1.,0.));
#11061=DIRECTION('',(0.,0.,-1.));
#11062=DIRECTION('',(0.,-1.,0.));
#11063=DIRECTION('center_axis',(0.,0.,-1.));
#11064=DIRECTION('ref_axis',(-0.707106781186548,-0.707106781186547,0.));
#11065=DIRECTION('center_axis',(0.,0.,1.));
#11066=DIRECTION('ref_axis',(-0.707106781186548,-0.707106781186547,0.));
#11067=DIRECTION('',(0.,0.,1.));
#11068=DIRECTION('center_axis',(0.,0.,1.));
#11069=DIRECTION('ref_axis',(-0.707106781186548,-0.707106781186547,0.));
#11070=DIRECTION('',(0.,0.,-1.));
#11071=DIRECTION('center_axis',(0.,0.,-1.));
#11072=DIRECTION('ref_axis',(-1.,0.,0.));
#11073=DIRECTION('',(0.,1.,0.));
#11074=DIRECTION('',(-1.,0.,0.));
#11075=DIRECTION('center_axis',(0.,0.,1.));
#11076=DIRECTION('ref_axis',(0.707106781186547,-0.707106781186547,0.));
#11077=DIRECTION('center_axis',(0.,0.,-1.));
#11078=DIRECTION('ref_axis',(1.,0.,0.));
#11079=DIRECTION('center_axis',(0.,0.,-1.));
#11080=DIRECTION('ref_axis',(-1.,0.,0.));
#11081=DIRECTION('center_axis',(0.,0.,-1.));
#11082=DIRECTION('ref_axis',(-1.,0.,0.));
#11083=DIRECTION('center_axis',(0.,-1.,0.));
#11084=DIRECTION('ref_axis',(-1.,0.,0.));
#11085=DIRECTION('',(-1.,0.,0.));
#11086=DIRECTION('',(0.,0.,1.));
#11087=DIRECTION('center_axis',(0.,-1.,0.));
#11088=DIRECTION('ref_axis',(0.,0.,-1.));
#11089=DIRECTION('center_axis',(0.,0.,-1.));
#11090=DIRECTION('ref_axis',(0.707106781186547,-0.707106781186547,0.));
#11091=DIRECTION('center_axis',(0.,0.,1.));
#11092=DIRECTION('ref_axis',(0.707106781186547,-0.707106781186547,0.));
#11093=DIRECTION('center_axis',(0.,1.,0.));
#11094=DIRECTION('ref_axis',(0.,0.,-1.));
#11095=DIRECTION('center_axis',(0.,1.,0.));
#11096=DIRECTION('ref_axis',(0.,0.,-1.));
#11097=DIRECTION('',(0.,1.,0.));
#11098=DIRECTION('center_axis',(0.,0.,1.));
#11099=DIRECTION('ref_axis',(-1.,0.,0.));
#11100=DIRECTION('center_axis',(0.,0.,1.));
#11101=DIRECTION('ref_axis',(-1.,0.,0.));
#11102=DIRECTION('center_axis',(0.,0.,1.));
#11103=DIRECTION('ref_axis',(-1.,0.,0.));
#11104=DIRECTION('center_axis',(0.,0.,1.));
#11105=DIRECTION('ref_axis',(-1.,0.,0.));
#11106=DIRECTION('center_axis',(0.,0.,1.));
#11107=DIRECTION('ref_axis',(-1.,0.,0.));
#11108=DIRECTION('',(0.,0.,1.));
#11109=DIRECTION('center_axis',(0.,0.,1.));
#11110=DIRECTION('ref_axis',(-1.,0.,0.));
#11111=DIRECTION('',(0.,0.,1.));
#11112=DIRECTION('center_axis',(0.,0.,1.));
#11113=DIRECTION('ref_axis',(-1.,0.,0.));
#11114=DIRECTION('center_axis',(0.,0.,1.));
#11115=DIRECTION('ref_axis',(-1.,0.,0.));
#11116=DIRECTION('center_axis',(0.,0.,1.));
#11117=DIRECTION('ref_axis',(-1.,0.,0.));
#11118=DIRECTION('center_axis',(0.,0.,1.));
#11119=DIRECTION('ref_axis',(-1.,0.,0.));
#11120=DIRECTION('center_axis',(0.,0.,1.));
#11121=DIRECTION('ref_axis',(-1.,0.,0.));
#11122=DIRECTION('',(0.,0.,1.));
#11123=DIRECTION('center_axis',(0.,0.,1.));
#11124=DIRECTION('ref_axis',(-1.,0.,0.));
#11125=DIRECTION('',(0.,0.,1.));
#11126=DIRECTION('center_axis',(0.,0.,1.));
#11127=DIRECTION('ref_axis',(1.,0.,0.));
#11128=DIRECTION('center_axis',(0.,0.,-1.));
#11129=DIRECTION('ref_axis',(1.,-6.05158675060312E-14,0.));
#11130=DIRECTION('center_axis',(0.,0.,-1.));
#11131=DIRECTION('ref_axis',(1.,0.,0.));
#11132=DIRECTION('center_axis',(0.,0.,1.));
#11133=DIRECTION('ref_axis',(1.,0.,0.));
#11134=DIRECTION('center_axis',(0.,0.,-1.));
#11135=DIRECTION('ref_axis',(1.,-5.61933055413145E-14,0.));
#11136=DIRECTION('center_axis',(0.,0.,-1.));
#11137=DIRECTION('ref_axis',(1.,0.,0.));
#11138=DIRECTION('center_axis',(0.,0.,1.));
#11139=DIRECTION('ref_axis',(1.,0.,0.));
#11140=DIRECTION('center_axis',(0.,0.,-1.));
#11141=DIRECTION('ref_axis',(1.,-5.61933055413145E-14,0.));
#11142=DIRECTION('center_axis',(0.,0.,-1.));
#11143=DIRECTION('ref_axis',(1.,0.,0.));
#11144=DIRECTION('center_axis',(0.,0.,1.));
#11145=DIRECTION('ref_axis',(1.,0.,0.));
#11146=DIRECTION('center_axis',(0.,0.,-1.));
#11147=DIRECTION('ref_axis',(1.,-6.05158675060312E-14,0.));
#11148=DIRECTION('center_axis',(0.,0.,-1.));
#11149=DIRECTION('ref_axis',(1.,0.,0.));
#11150=DIRECTION('center_axis',(0.,0.,-1.));
#11151=DIRECTION('ref_axis',(1.,0.,0.));
#11152=DIRECTION('center_axis',(0.,0.,-1.));
#11153=DIRECTION('ref_axis',(1.,0.,0.));
#11154=DIRECTION('center_axis',(0.,0.,-1.));
#11155=DIRECTION('ref_axis',(1.,0.,0.));
#11156=DIRECTION('center_axis',(0.,0.,-1.));
#11157=DIRECTION('ref_axis',(1.,0.,0.));
#11158=DIRECTION('center_axis',(0.,0.,-1.));
#11159=DIRECTION('ref_axis',(1.,0.,0.));
#11160=DIRECTION('center_axis',(0.,0.,-1.));
#11161=DIRECTION('ref_axis',(1.,0.,0.));
#11162=DIRECTION('',(0.,0.,-1.));
#11163=DIRECTION('center_axis',(0.,0.,1.));
#11164=DIRECTION('ref_axis',(1.,0.,0.));
#11165=DIRECTION('center_axis',(0.,0.,-1.));
#11166=DIRECTION('ref_axis',(1.,0.,0.));
#11167=DIRECTION('center_axis',(0.,0.,-1.));
#11168=DIRECTION('ref_axis',(1.,0.,0.));
#11169=DIRECTION('',(0.,0.,-1.));
#11170=DIRECTION('center_axis',(0.,0.,1.));
#11171=DIRECTION('ref_axis',(1.,0.,0.));
#11172=DIRECTION('center_axis',(0.,1.,0.));
#11173=DIRECTION('ref_axis',(-1.,0.,0.));
#11174=DIRECTION('',(-1.,0.,0.));
#11175=DIRECTION('',(0.,0.,-1.));
#11176=DIRECTION('',(-1.,0.,0.));
#11177=DIRECTION('',(0.,0.,1.));
#11178=DIRECTION('center_axis',(1.,0.,0.));
#11179=DIRECTION('ref_axis',(0.,1.,0.));
#11180=DIRECTION('',(0.,1.,0.));
#11181=DIRECTION('',(0.,1.,0.));
#11182=DIRECTION('',(0.,0.,1.));
#11183=DIRECTION('center_axis',(0.,-1.,0.));
#11184=DIRECTION('ref_axis',(1.,0.,0.));
#11185=DIRECTION('',(1.,0.,0.));
#11186=DIRECTION('',(1.,0.,0.));
#11187=DIRECTION('',(0.,0.,1.));
#11188=DIRECTION('center_axis',(0.,0.,1.));
#11189=DIRECTION('ref_axis',(1.,0.,0.));
#11190=DIRECTION('',(0.,1.,0.));
#11191=DIRECTION('center_axis',(0.,1.,0.));
#11192=DIRECTION('ref_axis',(-1.,0.,0.));
#11193=DIRECTION('',(-1.,0.,0.));
#11194=DIRECTION('',(0.,0.,1.));
#11195=DIRECTION('',(-1.,0.,0.));
#11196=DIRECTION('',(0.,0.,1.));
#11197=DIRECTION('center_axis',(0.,-1.,0.));
#11198=DIRECTION('ref_axis',(1.,0.,0.));
#11199=DIRECTION('',(1.,0.,0.));
#11200=DIRECTION('',(0.,0.,-1.));
#11201=DIRECTION('',(1.,0.,0.));
#11202=DIRECTION('',(0.,0.,1.));
#11203=DIRECTION('center_axis',(-1.,0.,0.));
#11204=DIRECTION('ref_axis',(0.,-1.,0.));
#11205=DIRECTION('',(0.,-1.,0.));
#11206=DIRECTION('',(0.,-1.,0.));
#11207=DIRECTION('center_axis',(0.,0.,1.));
#11208=DIRECTION('ref_axis',(1.,0.,0.));
#11209=DIRECTION('',(0.,-1.,0.));
#11210=DIRECTION('center_axis',(0.,0.,1.));
#11211=DIRECTION('ref_axis',(1.,0.,0.));
#11212=DIRECTION('center_axis',(0.,0.,-1.));
#11213=DIRECTION('ref_axis',(1.,0.,0.));
#11214=DIRECTION('',(0.,0.,-1.));
#11215=DIRECTION('center_axis',(0.,0.,1.));
#11216=DIRECTION('ref_axis',(1.,0.,0.));
#11217=DIRECTION('center_axis',(0.,0.,1.));
#11218=DIRECTION('ref_axis',(1.,0.,0.));
#11219=DIRECTION('center_axis',(0.,0.,1.));
#11220=DIRECTION('ref_axis',(1.,0.,0.));
#11221=DIRECTION('',(0.,0.,-1.));
#11222=DIRECTION('center_axis',(0.,0.,1.));
#11223=DIRECTION('ref_axis',(1.,0.,0.));
#11224=DIRECTION('center_axis',(-1.,0.,0.));
#11225=DIRECTION('ref_axis',(0.,1.,0.));
#11226=DIRECTION('',(0.,1.,0.));
#11227=DIRECTION('center_axis',(0.,0.,-1.));
#11228=DIRECTION('ref_axis',(-1.,0.,0.));
#11229=DIRECTION('center_axis',(0.,1.,0.));
#11230=DIRECTION('ref_axis',(-1.,0.,0.));
#11231=DIRECTION('',(-1.,0.,0.));
#11232=DIRECTION('',(0.,0.,1.));
#11233=DIRECTION('',(-1.,0.,0.));
#11234=DIRECTION('',(0.,0.,1.));
#11235=DIRECTION('center_axis',(1.,0.,0.));
#11236=DIRECTION('ref_axis',(0.,1.,0.));
#11237=DIRECTION('',(0.,1.,0.));
#11238=DIRECTION('',(0.,1.,0.));
#11239=DIRECTION('',(0.,0.,1.));
#11240=DIRECTION('',(0.,1.,0.));
#11241=DIRECTION('center_axis',(0.,-1.,0.));
#11242=DIRECTION('ref_axis',(1.,0.,0.));
#11243=DIRECTION('',(1.,0.,0.));
#11244=DIRECTION('',(1.,0.,0.));
#11245=DIRECTION('',(0.,0.,1.));
#11246=DIRECTION('center_axis',(-1.,0.,0.));
#11247=DIRECTION('ref_axis',(0.,-1.,0.));
#11248=DIRECTION('',(0.,-1.,0.));
#11249=DIRECTION('',(0.,-1.,0.));
#11250=DIRECTION('',(0.,-1.,0.));
#11251=DIRECTION('center_axis',(0.,0.,1.));
#11252=DIRECTION('ref_axis',(1.,0.,0.));
#11253=DIRECTION('center_axis',(0.,0.,1.));
#11254=DIRECTION('ref_axis',(1.,0.,0.));
#11255=DIRECTION('axis',(0.,0.,1.));
#11256=DIRECTION('refdir',(1.,0.,0.));
#11257=DIRECTION('center_axis',(0.,0.,-1.));
#11258=DIRECTION('ref_axis',(1.,0.,0.));
#11259=DIRECTION('center_axis',(0.,0.,-1.));
#11260=DIRECTION('ref_axis',(1.,0.,0.));
#11261=DIRECTION('',(0.,0.,-1.));
#11262=DIRECTION('center_axis',(0.,0.,1.));
#11263=DIRECTION('ref_axis',(1.,0.,0.));
#11264=DIRECTION('center_axis',(0.,0.,-1.));
#11265=DIRECTION('ref_axis',(1.,0.,0.));
#11266=DIRECTION('center_axis',(0.,0.,-1.));
#11267=DIRECTION('ref_axis',(1.,0.,0.));
#11268=DIRECTION('',(0.,0.,-1.));
#11269=DIRECTION('center_axis',(0.,0.,1.));
#11270=DIRECTION('ref_axis',(1.,0.,0.));
#11271=DIRECTION('center_axis',(0.,0.,-1.));
#11272=DIRECTION('ref_axis',(1.,0.,0.));
#11273=DIRECTION('center_axis',(0.,0.,-1.));
#11274=DIRECTION('ref_axis',(1.,0.,0.));
#11275=DIRECTION('',(0.,0.,-1.));
#11276=DIRECTION('center_axis',(0.,0.,1.));
#11277=DIRECTION('ref_axis',(1.,0.,0.));
#11278=DIRECTION('center_axis',(0.,0.,-1.));
#11279=DIRECTION('ref_axis',(1.,0.,0.));
#11280=DIRECTION('center_axis',(0.,0.,-1.));
#11281=DIRECTION('ref_axis',(1.,0.,0.));
#11282=DIRECTION('',(0.,0.,-1.));
#11283=DIRECTION('center_axis',(0.,0.,1.));
#11284=DIRECTION('ref_axis',(1.,0.,0.));
#11285=DIRECTION('center_axis',(0.,0.,-1.));
#11286=DIRECTION('ref_axis',(1.,0.,0.));
#11287=DIRECTION('center_axis',(0.,0.,-1.));
#11288=DIRECTION('ref_axis',(1.,0.,0.));
#11289=DIRECTION('',(0.,0.,-1.));
#11290=DIRECTION('center_axis',(0.,0.,1.));
#11291=DIRECTION('ref_axis',(1.,0.,0.));
#11292=DIRECTION('center_axis',(0.,1.,0.));
#11293=DIRECTION('ref_axis',(-1.,0.,0.));
#11294=DIRECTION('',(-1.,0.,0.));
#11295=DIRECTION('',(0.,0.,1.));
#11296=DIRECTION('',(-1.,0.,0.));
#11297=DIRECTION('',(0.,0.,1.));
#11298=DIRECTION('center_axis',(1.,0.,0.));
#11299=DIRECTION('ref_axis',(0.,1.,0.));
#11300=DIRECTION('',(0.,1.,0.));
#11301=DIRECTION('',(0.,1.,0.));
#11302=DIRECTION('',(0.,0.,1.));
#11303=DIRECTION('center_axis',(0.,-1.,0.));
#11304=DIRECTION('ref_axis',(1.,0.,0.));
#11305=DIRECTION('',(1.,0.,0.));
#11306=DIRECTION('',(1.,0.,0.));
#11307=DIRECTION('',(0.,0.,1.));
#11308=DIRECTION('center_axis',(-1.,0.,0.));
#11309=DIRECTION('ref_axis',(0.,-1.,0.));
#11310=DIRECTION('',(0.,-1.,0.));
#11311=DIRECTION('',(0.,-1.,0.));
#11312=DIRECTION('center_axis',(0.,0.,1.));
#11313=DIRECTION('ref_axis',(1.,0.,0.));
#11314=DIRECTION('center_axis',(0.,0.,1.));
#11315=DIRECTION('ref_axis',(1.,0.,0.));
#11316=DIRECTION('axis',(0.,0.,1.));
#11317=DIRECTION('refdir',(1.,0.,0.));
#11318=DIRECTION('center_axis',(0.,0.,1.));
#11319=DIRECTION('ref_axis',(1.,0.,0.));
#11320=DIRECTION('center_axis',(0.,0.,1.));
#11321=DIRECTION('ref_axis',(1.,0.,0.));
#11322=DIRECTION('center_axis',(0.,0.,1.));
#11323=DIRECTION('ref_axis',(1.,0.,0.));
#11324=DIRECTION('center_axis',(0.,0.,1.));
#11325=DIRECTION('ref_axis',(1.,0.,0.));
#11326=DIRECTION('',(0.,0.,-1.));
#11327=DIRECTION('center_axis',(0.,0.,1.));
#11328=DIRECTION('ref_axis',(1.,0.,0.));
#11329=DIRECTION('center_axis',(0.,0.,1.));
#11330=DIRECTION('ref_axis',(1.,0.,0.));
#11331=DIRECTION('center_axis',(0.,0.,-1.));
#11332=DIRECTION('ref_axis',(1.,0.,0.));
#11333=DIRECTION('center_axis',(0.,0.,1.));
#11334=DIRECTION('ref_axis',(1.,0.,0.));
#11335=DIRECTION('center_axis',(0.,0.,-1.));
#11336=DIRECTION('ref_axis',(1.,0.,0.));
#11337=DIRECTION('',(0.,0.,-1.));
#11338=DIRECTION('center_axis',(0.,0.,1.));
#11339=DIRECTION('ref_axis',(1.,0.,0.));
#11340=DIRECTION('center_axis',(0.,0.,1.));
#11341=DIRECTION('ref_axis',(1.,0.,0.));
#11342=DIRECTION('',(0.,0.,-1.));
#11343=DIRECTION('center_axis',(0.,0.,1.));
#11344=DIRECTION('ref_axis',(1.,0.,0.));
#11345=DIRECTION('axis',(0.,0.,1.));
#11346=DIRECTION('refdir',(1.,0.,0.));
#11347=DIRECTION('center_axis',(0.,0.,-1.));
#11348=DIRECTION('ref_axis',(-0.348549200809368,0.937290485716755,0.));
#11349=DIRECTION('',(0.,0.,-1.));
#11350=DIRECTION('center_axis',(0.,0.,-1.));
#11351=DIRECTION('ref_axis',(1.,0.,0.));
#11352=DIRECTION('center_axis',(0.,0.,-1.));
#11353=DIRECTION('ref_axis',(1.,0.,0.));
#11354=DIRECTION('',(0.,0.,-1.));
#11355=DIRECTION('center_axis',(0.,0.,-1.));
#11356=DIRECTION('ref_axis',(1.,0.,0.));
#11357=DIRECTION('',(0.,0.,-1.));
#11358=DIRECTION('center_axis',(0.,0.,-1.));
#11359=DIRECTION('ref_axis',(1.,0.,0.));
#11360=DIRECTION('',(0.,0.,-1.));
#11361=DIRECTION('center_axis',(0.,0.,-1.));
#11362=DIRECTION('ref_axis',(1.,0.,0.));
#11363=DIRECTION('',(0.,0.,-1.));
#11364=DIRECTION('center_axis',(0.,0.,-1.));
#11365=DIRECTION('ref_axis',(1.,0.,0.));
#11366=DIRECTION('',(0.,0.,-1.));
#11367=DIRECTION('center_axis',(0.,0.,-1.));
#11368=DIRECTION('ref_axis',(1.,0.,0.));
#11369=DIRECTION('',(0.,0.,-1.));
#11370=DIRECTION('center_axis',(0.,0.,-1.));
#11371=DIRECTION('ref_axis',(0.93737235570927,-0.348328963412538,0.));
#11372=DIRECTION('',(0.,0.,-1.));
#11373=DIRECTION('center_axis',(0.,0.,-1.));
#11374=DIRECTION('ref_axis',(1.,0.,0.));
#11375=DIRECTION('center_axis',(0.,0.,-1.));
#11376=DIRECTION('ref_axis',(-0.348549399150009,0.937290411960011,0.));
#11377=DIRECTION('',(0.,0.,-1.));
#11378=DIRECTION('center_axis',(0.,0.,-1.));
#11379=DIRECTION('ref_axis',(1.,0.,0.));
#11380=DIRECTION('center_axis',(0.,0.,-1.));
#11381=DIRECTION('ref_axis',(1.,0.,0.));
#11382=DIRECTION('',(0.,0.,-1.));
#11383=DIRECTION('center_axis',(0.,0.,-1.));
#11384=DIRECTION('ref_axis',(1.,0.,0.));
#11385=DIRECTION('',(0.,0.,-1.));
#11386=DIRECTION('center_axis',(0.,0.,-1.));
#11387=DIRECTION('ref_axis',(1.,0.,0.));
#11388=DIRECTION('',(0.,0.,-1.));
#11389=DIRECTION('center_axis',(0.,0.,-1.));
#11390=DIRECTION('ref_axis',(1.,0.,0.));
#11391=DIRECTION('',(0.,0.,-1.));
#11392=DIRECTION('center_axis',(0.,0.,-1.));
#11393=DIRECTION('ref_axis',(1.,0.,0.));
#11394=DIRECTION('',(0.,0.,-1.));
#11395=DIRECTION('center_axis',(0.,0.,-1.));
#11396=DIRECTION('ref_axis',(1.,0.,0.));
#11397=DIRECTION('',(0.,0.,-1.));
#11398=DIRECTION('center_axis',(0.,0.,-1.));
#11399=DIRECTION('ref_axis',(0.937372370252713,-0.348328924275332,0.));
#11400=DIRECTION('',(0.,0.,-1.));
#11401=DIRECTION('center_axis',(0.,0.,-1.));
#11402=DIRECTION('ref_axis',(1.,0.,0.));
#11403=DIRECTION('center_axis',(0.,0.,-1.));
#11404=DIRECTION('ref_axis',(0.793241641674985,0.608906969834288,0.));
#11405=DIRECTION('',(1.22464679914735E-16,-2.74659599554882E-30,-1.));
#11406=DIRECTION('center_axis',(0.,0.,1.));
#11407=DIRECTION('ref_axis',(1.,-2.23051936250031E-14,0.));
#11408=DIRECTION('center_axis',(0.,0.,-1.));
#11409=DIRECTION('ref_axis',(1.,-2.23051936250031E-14,0.));
#11410=DIRECTION('',(1.22464679914735E-16,-2.74659599554882E-30,-1.));
#11411=DIRECTION('center_axis',(0.,0.,-1.));
#11412=DIRECTION('ref_axis',(1.,-2.23051936250031E-14,0.));
#11413=DIRECTION('',(1.22464679914735E-16,-2.74659599554882E-30,-1.));
#11414=DIRECTION('center_axis',(0.,0.,-1.));
#11415=DIRECTION('ref_axis',(1.,-2.23051936250031E-14,0.));
#11416=DIRECTION('',(1.22464679914735E-16,-2.74659599554882E-30,-1.));
#11417=DIRECTION('center_axis',(0.,0.,-1.));
#11418=DIRECTION('ref_axis',(1.,-2.23051936250031E-14,0.));
#11419=DIRECTION('',(1.22464679914735E-16,-2.74659599554882E-30,-1.));
#11420=DIRECTION('center_axis',(0.,0.,-1.));
#11421=DIRECTION('ref_axis',(1.,-2.23051936250031E-14,0.));
#11422=DIRECTION('',(1.22464679914735E-16,-2.74659599554882E-30,-1.));
#11423=DIRECTION('center_axis',(0.,0.,-1.));
#11424=DIRECTION('ref_axis',(1.,-2.23051936250031E-14,0.));
#11425=DIRECTION('',(1.22464679914735E-16,-2.74659599554882E-30,-1.));
#11426=DIRECTION('center_axis',(0.,0.,-1.));
#11427=DIRECTION('ref_axis',(-0.609084174586186,-0.793105584565299,0.));
#11428=DIRECTION('',(1.22464679914735E-16,-2.74659599554882E-30,-1.));
#11429=DIRECTION('center_axis',(0.,0.,-1.));
#11430=DIRECTION('ref_axis',(1.,-2.23051936250031E-14,0.));
#11431=DIRECTION('center_axis',(0.,0.,-1.));
#11432=DIRECTION('ref_axis',(0.793241683023816,0.608906915967904,0.));
#11433=DIRECTION('',(1.22464679914735E-16,-2.65847991820295E-30,-1.));
#11434=DIRECTION('center_axis',(0.,0.,1.));
#11435=DIRECTION('ref_axis',(1.,-2.15856712500031E-14,0.));
#11436=DIRECTION('center_axis',(0.,0.,-1.));
#11437=DIRECTION('ref_axis',(1.,-2.15856712500031E-14,0.));
#11438=DIRECTION('',(1.22464679914735E-16,-2.65847991820295E-30,-1.));
#11439=DIRECTION('center_axis',(0.,0.,-1.));
#11440=DIRECTION('ref_axis',(1.,-2.15856712500031E-14,0.));
#11441=DIRECTION('',(1.22464679914735E-16,-2.65847991820295E-30,-1.));
#11442=DIRECTION('center_axis',(0.,0.,-1.));
#11443=DIRECTION('ref_axis',(1.,-2.15856712500031E-14,0.));
#11444=DIRECTION('',(1.22464679914735E-16,-2.65847991820295E-30,-1.));
#11445=DIRECTION('center_axis',(0.,0.,-1.));
#11446=DIRECTION('ref_axis',(1.,-2.15856712500031E-14,0.));
#11447=DIRECTION('',(1.22464679914735E-16,-2.65847991820295E-30,-1.));
#11448=DIRECTION('center_axis',(0.,0.,-1.));
#11449=DIRECTION('ref_axis',(1.,-2.15856712500031E-14,0.));
#11450=DIRECTION('',(1.22464679914735E-16,-2.65847991820295E-30,-1.));
#11451=DIRECTION('center_axis',(0.,0.,-1.));
#11452=DIRECTION('ref_axis',(1.,-2.15856712500031E-14,0.));
#11453=DIRECTION('',(1.22464679914735E-16,-2.65847991820295E-30,-1.));
#11454=DIRECTION('center_axis',(0.,0.,-1.));
#11455=DIRECTION('ref_axis',(-0.609084235810543,-0.793105537546604,0.));
#11456=DIRECTION('',(1.22464679914735E-16,-2.65847991820295E-30,-1.));
#11457=DIRECTION('center_axis',(0.,0.,-1.));
#11458=DIRECTION('ref_axis',(1.,-2.15856712500031E-14,0.));
#11459=DIRECTION('center_axis',(0.,0.,-1.));
#11460=DIRECTION('ref_axis',(1.,-2.15856712500031E-14,0.));
#11461=DIRECTION('center_axis',(0.,0.,1.));
#11462=DIRECTION('ref_axis',(1.,0.,0.));
#11463=DIRECTION('center_axis',(0.,0.,1.));
#11464=DIRECTION('ref_axis',(1.,0.,0.));
#11465=DIRECTION('',(1.,0.,0.));
#11466=DIRECTION('',(0.,-1.,0.));
#11467=DIRECTION('',(-1.,0.,0.));
#11468=DIRECTION('',(0.,1.,0.));
#11469=DIRECTION('',(1.,0.,0.));
#11470=DIRECTION('center_axis',(0.,0.,-1.));
#11471=DIRECTION('ref_axis',(1.,-2.23051936250031E-14,0.));
#11472=DIRECTION('center_axis',(0.,0.,-1.));
#11473=DIRECTION('ref_axis',(1.,0.,0.));
#11474=DIRECTION('center_axis',(0.,0.,-1.));
#11475=DIRECTION('ref_axis',(1.,0.,0.));
#11476=DIRECTION('center_axis',(-1.,0.,0.));
#11477=DIRECTION('ref_axis',(0.,1.,0.));
#11478=DIRECTION('center_axis',(-1.,0.,0.));
#11479=DIRECTION('ref_axis',(0.,1.,0.));
#11480=DIRECTION('',(-1.,0.,0.));
#11481=DIRECTION('center_axis',(1.,0.,0.));
#11482=DIRECTION('ref_axis',(0.,1.,0.));
#11483=DIRECTION('center_axis',(-1.,0.,0.));
#11484=DIRECTION('ref_axis',(0.,1.,0.));
#11485=DIRECTION('center_axis',(-1.,0.,0.));
#11486=DIRECTION('ref_axis',(0.,1.,0.));
#11487=DIRECTION('',(-1.,0.,0.));
#11488=DIRECTION('center_axis',(1.,0.,0.));
#11489=DIRECTION('ref_axis',(0.,1.,0.));
#11490=DIRECTION('center_axis',(-1.,0.,0.));
#11491=DIRECTION('ref_axis',(0.,-1.,0.));
#11492=DIRECTION('',(0.,1.,0.));
#11493=DIRECTION('',(0.,0.,1.));
#11494=DIRECTION('',(0.,-1.,0.));
#11495=DIRECTION('',(0.,0.,1.));
#11496=DIRECTION('center_axis',(0.,0.,1.));
#11497=DIRECTION('ref_axis',(1.,0.,0.));
#11498=DIRECTION('',(1.,0.,0.));
#11499=DIRECTION('',(0.,1.,0.));
#11500=DIRECTION('',(-1.,0.,0.));
#11501=DIRECTION('center_axis',(0.,-1.,0.));
#11502=DIRECTION('ref_axis',(1.,0.,0.));
#11503=DIRECTION('',(0.,0.,1.));
#11504=DIRECTION('',(1.,0.,0.));
#11505=DIRECTION('',(0.,0.,1.));
#11506=DIRECTION('',(1.,0.,0.));
#11507=DIRECTION('',(0.,0.,1.));
#11508=DIRECTION('',(1.,0.,0.));
#11509=DIRECTION('',(1.,0.,0.));
#11510=DIRECTION('center_axis',(0.,0.,1.));
#11511=DIRECTION('ref_axis',(1.,0.,0.));
#11512=DIRECTION('',(-1.,0.,0.));
#11513=DIRECTION('',(0.,-1.,0.));
#11514=DIRECTION('center_axis',(1.,0.,0.));
#11515=DIRECTION('ref_axis',(0.,1.,0.));
#11516=DIRECTION('',(0.,0.,1.));
#11517=DIRECTION('',(0.,1.,0.));
#11518=DIRECTION('center_axis',(0.,0.,1.));
#11519=DIRECTION('ref_axis',(1.,0.,0.));
#11520=DIRECTION('',(0.,-1.,0.));
#11521=DIRECTION('',(-1.,0.,0.));
#11522=DIRECTION('center_axis',(0.,0.,1.));
#11523=DIRECTION('ref_axis',(1.,0.,0.));
#11524=DIRECTION('center_axis',(0.,0.,-1.));
#11525=DIRECTION('ref_axis',(1.,0.,0.));
#11526=DIRECTION('',(-1.,0.,0.));
#11527=DIRECTION('',(0.,1.,0.));
#11528=DIRECTION('center_axis',(0.,0.,1.));
#11529=DIRECTION('ref_axis',(1.,0.,0.));
#11530=DIRECTION('center_axis',(0.,0.,-1.));
#11531=DIRECTION('ref_axis',(1.,0.,0.));
#11532=DIRECTION('',(0.,-1.,0.));
#11533=DIRECTION('',(-1.,0.,0.));
#11534=DIRECTION('center_axis',(0.,0.,-1.));
#11535=DIRECTION('ref_axis',(1.,0.,0.));
#11536=DIRECTION('center_axis',(0.,1.,0.));
#11537=DIRECTION('ref_axis',(-1.,0.,0.));
#11538=DIRECTION('',(0.,0.,1.));
#11539=DIRECTION('',(0.,0.,1.));
#11540=DIRECTION('center_axis',(1.,0.,0.));
#11541=DIRECTION('ref_axis',(0.,1.,0.));
#11542=DIRECTION('center_axis',(-1.,0.,0.));
#11543=DIRECTION('ref_axis',(0.,-1.,0.));
#11544=DIRECTION('center_axis',(0.,-1.,0.));
#11545=DIRECTION('ref_axis',(1.,0.,0.));
#11546=DIRECTION('',(0.,0.,1.));
#11547=DIRECTION('',(0.,0.,1.));
#11548=DIRECTION('',(1.,0.,0.));
#11549=DIRECTION('center_axis',(0.,1.,0.));
#11550=DIRECTION('ref_axis',(-1.,0.,0.));
#11551=DIRECTION('',(0.,0.,1.));
#11552=DIRECTION('',(-1.,0.,0.));
#11553=DIRECTION('',(0.,0.,1.));
#11554=DIRECTION('center_axis',(1.,0.,0.));
#11555=DIRECTION('ref_axis',(0.,1.,0.));
#11556=DIRECTION('',(0.,1.,0.));
#11557=DIRECTION('center_axis',(0.,-1.,0.));
#11558=DIRECTION('ref_axis',(1.,0.,0.));
#11559=DIRECTION('',(0.,0.,-1.));
#11560=DIRECTION('',(1.,0.,0.));
#11561=DIRECTION('',(0.,0.,1.));
#11562=DIRECTION('center_axis',(-1.,0.,0.));
#11563=DIRECTION('ref_axis',(0.,-1.,0.));
#11564=DIRECTION('',(0.,-1.,0.));
#11565=DIRECTION('center_axis',(0.,0.,1.));
#11566=DIRECTION('ref_axis',(-1.83697019872103E-16,-1.,0.));
#11567=DIRECTION('center_axis',(0.,0.,1.));
#11568=DIRECTION('ref_axis',(1.,0.,0.));
#11569=DIRECTION('center_axis',(0.,0.,1.));
#11570=DIRECTION('ref_axis',(1.,0.,0.));
#11571=DIRECTION('',(0.,0.,-1.));
#11572=DIRECTION('center_axis',(0.,0.,-1.));
#11573=DIRECTION('ref_axis',(1.,0.,0.));
#11574=DIRECTION('center_axis',(0.,0.,1.));
#11575=DIRECTION('ref_axis',(1.,0.,0.));
#11576=DIRECTION('axis',(0.,0.,1.));
#11577=DIRECTION('refdir',(1.,0.,0.));
#11578=DIRECTION('center_axis',(0.,0.,-1.));
#11579=DIRECTION('ref_axis',(1.,0.,0.));
#11580=DIRECTION('center_axis',(0.,0.,-1.));
#11581=DIRECTION('ref_axis',(1.,0.,0.));
#11582=DIRECTION('',(0.,0.,-1.));
#11583=DIRECTION('center_axis',(0.,0.,1.));
#11584=DIRECTION('ref_axis',(1.,0.,0.));
#11585=DIRECTION('center_axis',(0.,0.,-1.));
#11586=DIRECTION('ref_axis',(1.,0.,0.));
#11587=DIRECTION('center_axis',(0.,0.,-1.));
#11588=DIRECTION('ref_axis',(1.,0.,0.));
#11589=DIRECTION('',(0.,0.,-1.));
#11590=DIRECTION('center_axis',(0.,0.,1.));
#11591=DIRECTION('ref_axis',(1.,0.,0.));
#11592=DIRECTION('center_axis',(0.,1.,0.));
#11593=DIRECTION('ref_axis',(-1.,0.,0.));
#11594=DIRECTION('',(-1.,0.,0.));
#11595=DIRECTION('',(0.,0.,1.));
#11596=DIRECTION('',(-1.,0.,0.));
#11597=DIRECTION('',(0.,0.,1.));
#11598=DIRECTION('center_axis',(1.,0.,0.));
#11599=DIRECTION('ref_axis',(0.,1.,0.));
#11600=DIRECTION('',(0.,1.,0.));
#11601=DIRECTION('',(0.,1.,0.));
#11602=DIRECTION('',(0.,0.,1.));
#11603=DIRECTION('center_axis',(0.,-1.,0.));
#11604=DIRECTION('ref_axis',(1.,0.,0.));
#11605=DIRECTION('',(1.,0.,0.));
#11606=DIRECTION('',(1.,0.,0.));
#11607=DIRECTION('',(0.,0.,1.));
#11608=DIRECTION('center_axis',(-1.,0.,0.));
#11609=DIRECTION('ref_axis',(0.,-1.,0.));
#11610=DIRECTION('',(0.,-1.,0.));
#11611=DIRECTION('',(0.,-1.,0.));
#11612=DIRECTION('center_axis',(0.,0.,1.));
#11613=DIRECTION('ref_axis',(1.,0.,0.));
#11614=DIRECTION('center_axis',(0.,0.,1.));
#11615=DIRECTION('ref_axis',(1.,0.,0.));
#11616=DIRECTION('axis',(0.,0.,1.));
#11617=DIRECTION('refdir',(1.,0.,0.));
#11618=DIRECTION('center_axis',(0.,0.,1.));
#11619=DIRECTION('ref_axis',(1.,0.,0.));
#11620=DIRECTION('center_axis',(0.,0.,-1.));
#11621=DIRECTION('ref_axis',(1.,0.,0.));
#11622=DIRECTION('',(0.707106781186547,8.65956056235493E-17,-0.707106781186548));
#11623=DIRECTION('center_axis',(0.,0.,1.));
#11624=DIRECTION('ref_axis',(1.,0.,0.));
#11625=DIRECTION('center_axis',(0.,0.,1.));
#11626=DIRECTION('ref_axis',(1.,0.,0.));
#11627=DIRECTION('center_axis',(0.,0.,1.));
#11628=DIRECTION('ref_axis',(1.,0.,0.));
#11629=DIRECTION('',(0.,0.,-1.));
#11630=DIRECTION('center_axis',(0.,0.,1.));
#11631=DIRECTION('ref_axis',(1.,0.,0.));
#11632=DIRECTION('center_axis',(0.,0.,-1.));
#11633=DIRECTION('ref_axis',(1.,0.,0.));
#11634=DIRECTION('center_axis',(0.,0.,-1.));
#11635=DIRECTION('ref_axis',(1.,0.,0.));
#11636=DIRECTION('center_axis',(0.,0.,-1.));
#11637=DIRECTION('ref_axis',(1.,0.,0.));
#11638=DIRECTION('',(-0.707106781186548,-8.65956056235494E-17,-0.707106781186548));
#11639=DIRECTION('center_axis',(0.,0.,1.));
#11640=DIRECTION('ref_axis',(1.,0.,0.));
#11641=DIRECTION('center_axis',(0.,0.,1.));
#11642=DIRECTION('ref_axis',(1.,0.,0.));
#11643=DIRECTION('center_axis',(0.,0.,-1.));
#11644=DIRECTION('ref_axis',(1.,0.,0.));
#11645=DIRECTION('center_axis',(0.,0.,1.));
#11646=DIRECTION('ref_axis',(1.,0.,0.));
#11647=DIRECTION('',(-0.707106781186547,-8.65956056235493E-17,-0.707106781186548));
#11648=DIRECTION('center_axis',(0.,0.,1.));
#11649=DIRECTION('ref_axis',(1.,0.,0.));
#11650=DIRECTION('center_axis',(0.,0.,-1.));
#11651=DIRECTION('ref_axis',(1.,0.,0.));
#11652=DIRECTION('',(0.,0.,-1.));
#11653=DIRECTION('center_axis',(0.,0.,1.));
#11654=DIRECTION('ref_axis',(1.,0.,0.));
#11655=DIRECTION('',(0.707106781186547,8.65956056235493E-17,-0.707106781186547));
#11656=DIRECTION('axis',(0.,0.,1.));
#11657=DIRECTION('refdir',(1.,0.,0.));
#11658=DIRECTION('center_axis',(0.,0.,1.));
#11659=DIRECTION('ref_axis',(-1.,0.,0.));
#11660=DIRECTION('',(0.,0.,1.));
#11661=DIRECTION('center_axis',(0.,0.,-1.));
#11662=DIRECTION('ref_axis',(-1.,0.,0.));
#11663=DIRECTION('',(0.,0.,1.));
#11664=DIRECTION('center_axis',(0.,0.,-1.));
#11665=DIRECTION('ref_axis',(-1.,0.,0.));
#11666=DIRECTION('center_axis',(0.,0.,1.));
#11667=DIRECTION('ref_axis',(-1.,0.,0.));
#11668=DIRECTION('',(0.,0.,1.));
#11669=DIRECTION('center_axis',(0.,0.,1.));
#11670=DIRECTION('ref_axis',(-1.,0.,0.));
#11671=DIRECTION('',(0.,0.,1.));
#11672=DIRECTION('center_axis',(0.,0.,1.));
#11673=DIRECTION('ref_axis',(-1.,0.,0.));
#11674=DIRECTION('',(0.,0.,1.));
#11675=DIRECTION('center_axis',(0.,0.,1.));
#11676=DIRECTION('ref_axis',(-1.,0.,0.));
#11677=DIRECTION('',(0.,0.,1.));
#11678=DIRECTION('center_axis',(0.,0.,1.));
#11679=DIRECTION('ref_axis',(-1.,0.,0.));
#11680=DIRECTION('',(0.,0.,1.));
#11681=DIRECTION('center_axis',(0.,0.,1.));
#11682=DIRECTION('ref_axis',(-1.,0.,0.));
#11683=DIRECTION('',(0.,0.,1.));
#11684=DIRECTION('center_axis',(0.,0.,1.));
#11685=DIRECTION('ref_axis',(-1.,0.,0.));
#11686=DIRECTION('',(0.,0.,1.));
#11687=DIRECTION('center_axis',(0.,0.,1.));
#11688=DIRECTION('ref_axis',(-1.,0.,0.));
#11689=DIRECTION('',(0.,0.,1.));
#11690=DIRECTION('center_axis',(0.,0.,1.));
#11691=DIRECTION('ref_axis',(-1.,0.,0.));
#11692=DIRECTION('',(0.,0.,1.));
#11693=DIRECTION('center_axis',(0.,0.,1.));
#11694=DIRECTION('ref_axis',(-1.,0.,0.));
#11695=DIRECTION('',(0.,0.,1.));
#11696=DIRECTION('center_axis',(0.,0.,1.));
#11697=DIRECTION('ref_axis',(-0.938434237953747,-0.345457929473576,0.));
#11698=DIRECTION('',(0.,0.,1.));
#11699=DIRECTION('center_axis',(0.,0.,-1.));
#11700=DIRECTION('ref_axis',(-1.,0.,0.));
#11701=DIRECTION('center_axis',(0.,0.,1.));
#11702=DIRECTION('ref_axis',(-0.450135889590755,0.892960066801612,0.));
#11703=DIRECTION('',(-1.22464679914735E-16,-7.02543712147503E-30,1.));
#11704=DIRECTION('center_axis',(0.,0.,-1.));
#11705=DIRECTION('ref_axis',(-1.,-5.72445829159016E-14,0.));
#11706=DIRECTION('center_axis',(0.,0.,1.));
#11707=DIRECTION('ref_axis',(-1.,-5.72445829159016E-14,0.));
#11708=DIRECTION('',(-1.22464679914735E-16,-7.02543712147503E-30,1.));
#11709=DIRECTION('center_axis',(0.,0.,1.));
#11710=DIRECTION('ref_axis',(-1.,-5.72445829159016E-14,0.));
#11711=DIRECTION('',(-1.22464679914735E-16,-7.02543712147503E-30,1.));
#11712=DIRECTION('center_axis',(0.,0.,1.));
#11713=DIRECTION('ref_axis',(-1.,-5.72445829159016E-14,0.));
#11714=DIRECTION('',(-1.22464679914735E-16,-7.02543712147503E-30,1.));
#11715=DIRECTION('center_axis',(0.,0.,1.));
#11716=DIRECTION('ref_axis',(-1.,-5.72445829159016E-14,0.));
#11717=DIRECTION('',(-1.22464679914735E-16,-7.02543712147503E-30,1.));
#11718=DIRECTION('center_axis',(0.,0.,1.));
#11719=DIRECTION('ref_axis',(-1.,-5.72445829159016E-14,0.));
#11720=DIRECTION('',(-1.22464679914735E-16,-7.02543712147503E-30,1.));
#11721=DIRECTION('center_axis',(0.,0.,1.));
#11722=DIRECTION('ref_axis',(-1.,-5.72445829159016E-14,0.));
#11723=DIRECTION('',(-1.22464679914735E-16,-7.02543712147503E-30,1.));
#11724=DIRECTION('center_axis',(0.,0.,1.));
#11725=DIRECTION('ref_axis',(-1.,-5.72445829159016E-14,0.));
#11726=DIRECTION('',(-1.22464679914735E-16,-7.02543712147503E-30,1.));
#11727=DIRECTION('center_axis',(0.,0.,1.));
#11728=DIRECTION('ref_axis',(-1.,-5.72445829159016E-14,0.));
#11729=DIRECTION('',(-1.22464679914735E-16,-7.02543712147503E-30,1.));
#11730=DIRECTION('center_axis',(0.,0.,1.));
#11731=DIRECTION('ref_axis',(-1.,-5.72445829159016E-14,0.));
#11732=DIRECTION('',(-1.22464679914735E-16,-7.02543712147503E-30,1.));
#11733=DIRECTION('center_axis',(0.,0.,1.));
#11734=DIRECTION('ref_axis',(-1.,-5.72445829159016E-14,0.));
#11735=DIRECTION('',(-1.22464679914735E-16,-7.02543712147503E-30,1.));
#11736=DIRECTION('center_axis',(0.,0.,1.));
#11737=DIRECTION('ref_axis',(-1.,-5.72445829159016E-14,0.));
#11738=DIRECTION('',(-1.22464679914735E-16,-7.02543712147503E-30,1.));
#11739=DIRECTION('center_axis',(0.,0.,1.));
#11740=DIRECTION('ref_axis',(0.609351642559645,-0.79290010449606,0.));
#11741=DIRECTION('',(-1.22464679914735E-16,-7.02543712147503E-30,1.));
#11742=DIRECTION('center_axis',(0.,0.,1.));
#11743=DIRECTION('ref_axis',(-1.,-5.72445829159016E-14,0.));
#11744=DIRECTION('center_axis',(0.,0.,-1.));
#11745=DIRECTION('ref_axis',(1.,0.,0.));
#11746=DIRECTION('',(0.,0.,-1.));
#11747=DIRECTION('center_axis',(0.,0.,1.));
#11748=DIRECTION('ref_axis',(1.,0.,0.));
#11749=DIRECTION('',(0.,0.,-1.));
#11750=DIRECTION('center_axis',(0.,0.,1.));
#11751=DIRECTION('ref_axis',(1.,0.,0.));
#11752=DIRECTION('center_axis',(0.,0.,1.));
#11753=DIRECTION('ref_axis',(1.,0.,0.));
#11754=DIRECTION('center_axis',(0.,0.,-1.));
#11755=DIRECTION('ref_axis',(1.,0.,0.));
#11756=DIRECTION('',(0.,0.,-1.));
#11757=DIRECTION('center_axis',(0.,0.,-1.));
#11758=DIRECTION('ref_axis',(1.,0.,0.));
#11759=DIRECTION('',(0.,0.,-1.));
#11760=DIRECTION('center_axis',(0.,0.,-1.));
#11761=DIRECTION('ref_axis',(1.,0.,0.));
#11762=DIRECTION('',(0.,0.,-1.));
#11763=DIRECTION('center_axis',(0.,0.,-1.));
#11764=DIRECTION('ref_axis',(1.,0.,0.));
#11765=DIRECTION('',(0.,0.,-1.));
#11766=DIRECTION('center_axis',(0.,0.,-1.));
#11767=DIRECTION('ref_axis',(1.,0.,0.));
#11768=DIRECTION('',(0.,0.,-1.));
#11769=DIRECTION('center_axis',(0.,0.,-1.));
#11770=DIRECTION('ref_axis',(1.,0.,0.));
#11771=DIRECTION('',(0.,0.,-1.));
#11772=DIRECTION('center_axis',(0.,0.,-1.));
#11773=DIRECTION('ref_axis',(1.,0.,0.));
#11774=DIRECTION('',(0.,0.,-1.));
#11775=DIRECTION('center_axis',(0.,0.,-1.));
#11776=DIRECTION('ref_axis',(1.,0.,0.));
#11777=DIRECTION('',(0.,0.,-1.));
#11778=DIRECTION('center_axis',(0.,0.,-1.));
#11779=DIRECTION('ref_axis',(1.,0.,0.));
#11780=DIRECTION('',(0.,0.,-1.));
#11781=DIRECTION('center_axis',(0.,0.,-1.));
#11782=DIRECTION('ref_axis',(1.,0.,0.));
#11783=DIRECTION('',(0.,0.,-1.));
#11784=DIRECTION('center_axis',(0.,0.,-1.));
#11785=DIRECTION('ref_axis',(1.,0.,0.));
#11786=DIRECTION('',(0.,0.,-1.));
#11787=DIRECTION('center_axis',(0.,0.,-1.));
#11788=DIRECTION('ref_axis',(1.,0.,0.));
#11789=DIRECTION('',(0.,0.,-1.));
#11790=DIRECTION('center_axis',(0.,0.,-1.));
#11791=DIRECTION('ref_axis',(1.,0.,0.));
#11792=DIRECTION('',(0.,0.,-1.));
#11793=DIRECTION('center_axis',(0.,0.,-1.));
#11794=DIRECTION('ref_axis',(1.,0.,0.));
#11795=DIRECTION('',(0.,0.,-1.));
#11796=DIRECTION('center_axis',(0.,0.,-1.));
#11797=DIRECTION('ref_axis',(1.,0.,0.));
#11798=DIRECTION('',(0.,0.,-1.));
#11799=DIRECTION('center_axis',(0.,0.,-1.));
#11800=DIRECTION('ref_axis',(1.,0.,0.));
#11801=DIRECTION('',(0.,0.,-1.));
#11802=DIRECTION('center_axis',(0.,0.,-1.));
#11803=DIRECTION('ref_axis',(0.937376106323228,-0.348318870138132,0.));
#11804=DIRECTION('',(0.,0.,-1.));
#11805=DIRECTION('center_axis',(0.,0.,-1.));
#11806=DIRECTION('ref_axis',(1.,0.,0.));
#11807=DIRECTION('center_axis',(0.,0.,-1.));
#11808=DIRECTION('ref_axis',(1.,-9.27379496885572E-14,0.));
#11809=DIRECTION('',(1.22464679914735E-16,-1.13721209223846E-29,-1.));
#11810=DIRECTION('center_axis',(0.,0.,1.));
#11811=DIRECTION('ref_axis',(1.,-9.27379496885572E-14,0.));
#11812=DIRECTION('center_axis',(0.,0.,-1.));
#11813=DIRECTION('ref_axis',(1.,-9.27379496885572E-14,0.));
#11814=DIRECTION('',(1.22464679914735E-16,-1.13721209223846E-29,-1.));
#11815=DIRECTION('center_axis',(0.,0.,-1.));
#11816=DIRECTION('ref_axis',(1.,-9.27379496885572E-14,0.));
#11817=DIRECTION('',(1.22464679914735E-16,-1.13721209223846E-29,-1.));
#11818=DIRECTION('center_axis',(0.,0.,-1.));
#11819=DIRECTION('ref_axis',(1.,-9.27379496885572E-14,0.));
#11820=DIRECTION('',(1.22464679914735E-16,-1.13721209223846E-29,-1.));
#11821=DIRECTION('center_axis',(0.,0.,-1.));
#11822=DIRECTION('ref_axis',(1.,-9.27379496885572E-14,0.));
#11823=DIRECTION('',(1.22464679914735E-16,-1.13721209223846E-29,-1.));
#11824=DIRECTION('center_axis',(0.,0.,-1.));
#11825=DIRECTION('ref_axis',(1.,-9.27379496885572E-14,0.));
#11826=DIRECTION('',(1.22464679914735E-16,-1.13721209223846E-29,-1.));
#11827=DIRECTION('center_axis',(0.,0.,-1.));
#11828=DIRECTION('ref_axis',(1.,-9.27379496885572E-14,0.));
#11829=DIRECTION('',(1.22464679914735E-16,-1.13721209223846E-29,-1.));
#11830=DIRECTION('center_axis',(0.,0.,-1.));
#11831=DIRECTION('ref_axis',(1.,-9.27379496885572E-14,0.));
#11832=DIRECTION('',(1.22464679914735E-16,-1.13721209223846E-29,-1.));
#11833=DIRECTION('center_axis',(0.,0.,-1.));
#11834=DIRECTION('ref_axis',(1.,-9.27379496885572E-14,0.));
#11835=DIRECTION('',(1.22464679914735E-16,-1.13721209223846E-29,-1.));
#11836=DIRECTION('center_axis',(0.,0.,-1.));
#11837=DIRECTION('ref_axis',(1.,-9.27379496885572E-14,0.));
#11838=DIRECTION('',(1.22464679914735E-16,-1.13721209223846E-29,-1.));
#11839=DIRECTION('center_axis',(0.,0.,-1.));
#11840=DIRECTION('ref_axis',(1.,-9.27379496885572E-14,0.));
#11841=DIRECTION('',(1.22464679914735E-16,-1.13721209223846E-29,-1.));
#11842=DIRECTION('center_axis',(0.,0.,-1.));
#11843=DIRECTION('ref_axis',(1.,-9.27379496885572E-14,0.));
#11844=DIRECTION('',(1.22464679914735E-16,-1.13721209223846E-29,-1.));
#11845=DIRECTION('center_axis',(0.,0.,-1.));
#11846=DIRECTION('ref_axis',(1.,-9.27379496885572E-14,0.));
#11847=DIRECTION('',(1.22464679914735E-16,-1.13721209223846E-29,-1.));
#11848=DIRECTION('center_axis',(0.,0.,-1.));
#11849=DIRECTION('ref_axis',(1.,-9.27379496885572E-14,0.));
#11850=DIRECTION('',(1.22464679914735E-16,-1.13721209223846E-29,-1.));
#11851=DIRECTION('center_axis',(0.,0.,-1.));
#11852=DIRECTION('ref_axis',(1.,-9.27379496885572E-14,0.));
#11853=DIRECTION('',(1.22464679914735E-16,-1.13721209223846E-29,-1.));
#11854=DIRECTION('center_axis',(0.,0.,-1.));
#11855=DIRECTION('ref_axis',(1.,-9.27379496885572E-14,0.));
#11856=DIRECTION('',(1.22464679914735E-16,-1.13721209223846E-29,-1.));
#11857=DIRECTION('center_axis',(0.,0.,-1.));
#11858=DIRECTION('ref_axis',(1.,-9.27379496885572E-14,0.));
#11859=DIRECTION('',(1.22464679914735E-16,-1.13721209223846E-29,-1.));
#11860=DIRECTION('center_axis',(0.,0.,-1.));
#11861=DIRECTION('ref_axis',(-0.609161390867883,-0.793046278520936,0.));
#11862=DIRECTION('',(1.22464679914735E-16,-1.13721209223846E-29,-1.));
#11863=DIRECTION('center_axis',(0.,0.,-1.));
#11864=DIRECTION('ref_axis',(1.,-9.27379496885572E-14,0.));
#11865=DIRECTION('center_axis',(0.,0.,1.));
#11866=DIRECTION('ref_axis',(1.,0.,0.));
#11867=DIRECTION('center_axis',(0.,0.,-1.));
#11868=DIRECTION('ref_axis',(1.,-9.27379496885572E-14,0.));
#11869=DIRECTION('center_axis',(0.,0.,-1.));
#11870=DIRECTION('ref_axis',(1.,0.,0.));
#11871=DIRECTION('center_axis',(0.,0.,-1.));
#11872=DIRECTION('ref_axis',(1.,0.,0.));
#11873=DIRECTION('center_axis',(0.,0.,1.));
#11874=DIRECTION('ref_axis',(1.,0.,0.));
#11875=DIRECTION('center_axis',(0.,0.,1.));
#11876=DIRECTION('ref_axis',(-1.,-5.72445829159016E-14,0.));
#11877=DIRECTION('center_axis',(0.,0.,1.));
#11878=DIRECTION('ref_axis',(-1.,0.,0.));
#11879=DIRECTION('center_axis',(0.,0.,1.));
#11880=DIRECTION('ref_axis',(-1.,0.,0.));
#11881=DIRECTION('center_axis',(0.,1.,0.));
#11882=DIRECTION('ref_axis',(-1.,0.,0.));
#11883=DIRECTION('',(-1.,0.,0.));
#11884=DIRECTION('',(0.,0.,1.));
#11885=DIRECTION('',(-1.,0.,0.));
#11886=DIRECTION('',(0.,0.,1.));
#11887=DIRECTION('center_axis',(1.,0.,0.));
#11888=DIRECTION('ref_axis',(0.,1.,0.));
#11889=DIRECTION('',(0.,1.,0.));
#11890=DIRECTION('',(0.,1.,0.));
#11891=DIRECTION('',(0.,0.,1.));
#11892=DIRECTION('center_axis',(0.,-1.,0.));
#11893=DIRECTION('ref_axis',(1.,0.,0.));
#11894=DIRECTION('',(1.,0.,0.));
#11895=DIRECTION('',(1.,0.,0.));
#11896=DIRECTION('',(0.,0.,1.));
#11897=DIRECTION('center_axis',(-1.,0.,0.));
#11898=DIRECTION('ref_axis',(0.,-1.,0.));
#11899=DIRECTION('',(0.,-1.,0.));
#11900=DIRECTION('',(0.,-1.,0.));
#11901=DIRECTION('center_axis',(0.,0.,1.));
#11902=DIRECTION('ref_axis',(1.,0.,0.));
#11903=DIRECTION('center_axis',(0.,0.,1.));
#11904=DIRECTION('ref_axis',(1.,0.,0.));
#11905=DIRECTION('axis',(0.,0.,1.));
#11906=DIRECTION('refdir',(1.,0.,0.));
#11907=DIRECTION('center_axis',(0.,0.,-1.));
#11908=DIRECTION('ref_axis',(1.,0.,0.));
#11909=DIRECTION('',(0.,0.,-1.));
#11910=DIRECTION('center_axis',(0.,0.,1.));
#11911=DIRECTION('ref_axis',(1.,0.,0.));
#11912=DIRECTION('',(0.,0.,-1.));
#11913=DIRECTION('center_axis',(0.,0.,1.));
#11914=DIRECTION('ref_axis',(1.,0.,0.));
#11915=DIRECTION('center_axis',(0.,0.,1.));
#11916=DIRECTION('ref_axis',(1.,0.,0.));
#11917=DIRECTION('center_axis',(0.,0.,-1.));
#11918=DIRECTION('ref_axis',(1.,0.,0.));
#11919=DIRECTION('',(0.,0.,-1.));
#11920=DIRECTION('center_axis',(0.,0.,-1.));
#11921=DIRECTION('ref_axis',(1.,0.,0.));
#11922=DIRECTION('',(0.,0.,-1.));
#11923=DIRECTION('center_axis',(0.,0.,-1.));
#11924=DIRECTION('ref_axis',(1.,0.,0.));
#11925=DIRECTION('',(0.,0.,-1.));
#11926=DIRECTION('center_axis',(0.,0.,-1.));
#11927=DIRECTION('ref_axis',(1.,0.,0.));
#11928=DIRECTION('',(0.,0.,-1.));
#11929=DIRECTION('center_axis',(0.,0.,-1.));
#11930=DIRECTION('ref_axis',(1.,0.,0.));
#11931=DIRECTION('',(0.,0.,-1.));
#11932=DIRECTION('center_axis',(0.,0.,-1.));
#11933=DIRECTION('ref_axis',(1.,0.,0.));
#11934=DIRECTION('',(0.,0.,-1.));
#11935=DIRECTION('center_axis',(0.,0.,-1.));
#11936=DIRECTION('ref_axis',(1.,0.,0.));
#11937=DIRECTION('',(0.,0.,-1.));
#11938=DIRECTION('center_axis',(0.,0.,-1.));
#11939=DIRECTION('ref_axis',(1.,0.,0.));
#11940=DIRECTION('',(0.,0.,-1.));
#11941=DIRECTION('center_axis',(0.,0.,-1.));
#11942=DIRECTION('ref_axis',(0.937367309351136,-0.348342543137946,0.));
#11943=DIRECTION('',(0.,0.,-1.));
#11944=DIRECTION('center_axis',(0.,0.,-1.));
#11945=DIRECTION('ref_axis',(1.,0.,0.));
#11946=DIRECTION('center_axis',(0.,0.,-1.));
#11947=DIRECTION('ref_axis',(1.,-4.8329028703551E-14,0.));
#11948=DIRECTION('',(1.22464679914735E-16,-5.93359662859705E-30,-1.));
#11949=DIRECTION('center_axis',(0.,0.,1.));
#11950=DIRECTION('ref_axis',(1.,-4.8329028703551E-14,0.));
#11951=DIRECTION('center_axis',(0.,0.,-1.));
#11952=DIRECTION('ref_axis',(1.,-4.8329028703551E-14,0.));
#11953=DIRECTION('',(1.22464679914735E-16,-5.93359662859705E-30,-1.));
#11954=DIRECTION('center_axis',(0.,0.,-1.));
#11955=DIRECTION('ref_axis',(1.,-4.8329028703551E-14,0.));
#11956=DIRECTION('',(1.22464679914735E-16,-5.93359662859705E-30,-1.));
#11957=DIRECTION('center_axis',(0.,0.,-1.));
#11958=DIRECTION('ref_axis',(1.,-4.8329028703551E-14,0.));
#11959=DIRECTION('',(1.22464679914735E-16,-5.93359662859705E-30,-1.));
#11960=DIRECTION('center_axis',(0.,0.,-1.));
#11961=DIRECTION('ref_axis',(1.,-4.8329028703551E-14,0.));
#11962=DIRECTION('',(1.22464679914735E-16,-5.93359662859705E-30,-1.));
#11963=DIRECTION('center_axis',(0.,0.,-1.));
#11964=DIRECTION('ref_axis',(1.,-4.8329028703551E-14,0.));
#11965=DIRECTION('',(1.22464679914735E-16,-5.93359662859705E-30,-1.));
#11966=DIRECTION('center_axis',(0.,0.,-1.));
#11967=DIRECTION('ref_axis',(1.,-4.8329028703551E-14,0.));
#11968=DIRECTION('',(1.22464679914735E-16,-5.93359662859705E-30,-1.));
#11969=DIRECTION('center_axis',(0.,0.,-1.));
#11970=DIRECTION('ref_axis',(1.,-4.8329028703551E-14,0.));
#11971=DIRECTION('',(1.22464679914735E-16,-5.93359662859705E-30,-1.));
#11972=DIRECTION('center_axis',(0.,0.,-1.));
#11973=DIRECTION('ref_axis',(1.,-4.8329028703551E-14,0.));
#11974=DIRECTION('',(1.22464679914735E-16,-5.93359662859705E-30,-1.));
#11975=DIRECTION('center_axis',(0.,0.,-1.));
#11976=DIRECTION('ref_axis',(-0.609222020738255,-0.792999703308644,0.));
#11977=DIRECTION('',(1.22464679914735E-16,-5.93359662859705E-30,-1.));
#11978=DIRECTION('center_axis',(0.,0.,-1.));
#11979=DIRECTION('ref_axis',(1.,-4.8329028703551E-14,0.));
#11980=DIRECTION('center_axis',(0.,0.,1.));
#11981=DIRECTION('ref_axis',(1.,0.,0.));
#11982=DIRECTION('center_axis',(0.,0.,-1.));
#11983=DIRECTION('ref_axis',(1.,-4.8329028703551E-14,0.));
#11984=DIRECTION('center_axis',(0.,0.,-1.));
#11985=DIRECTION('ref_axis',(1.,0.,0.));
#11986=DIRECTION('center_axis',(0.,0.,-1.));
#11987=DIRECTION('ref_axis',(1.,0.,0.));
#11988=DIRECTION('center_axis',(0.,0.,-1.));
#11989=DIRECTION('ref_axis',(1.,0.,0.));
#11990=DIRECTION('center_axis',(0.,0.,-1.));
#11991=DIRECTION('ref_axis',(1.,0.,0.));
#11992=DIRECTION('',(0.,0.,-1.));
#11993=DIRECTION('center_axis',(0.,0.,1.));
#11994=DIRECTION('ref_axis',(1.,0.,0.));
#11995=DIRECTION('center_axis',(1.,0.,0.));
#11996=DIRECTION('ref_axis',(0.,1.,0.));
#11997=DIRECTION('',(0.,1.,0.));
#11998=DIRECTION('',(0.,0.,1.));
#11999=DIRECTION('',(0.,1.,0.));
#12000=DIRECTION('',(0.,0.,1.));
#12001=DIRECTION('center_axis',(0.,0.,1.));
#12002=DIRECTION('ref_axis',(1.,0.,0.));
#12003=DIRECTION('',(0.,-1.,0.));
#12004=DIRECTION('',(-1.,0.,0.));
#12005=DIRECTION('',(1.,0.,0.));
#12006=DIRECTION('center_axis',(0.,1.,0.));
#12007=DIRECTION('ref_axis',(-1.,0.,0.));
#12008=DIRECTION('',(-1.,0.,0.));
#12009=DIRECTION('',(0.,0.,1.));
#12010=DIRECTION('',(-1.,0.,0.));
#12011=DIRECTION('',(0.,0.,1.));
#12012=DIRECTION('center_axis',(1.,0.,0.));
#12013=DIRECTION('ref_axis',(0.,1.,0.));
#12014=DIRECTION('',(0.,0.,1.));
#12015=DIRECTION('',(0.,1.,0.));
#12016=DIRECTION('center_axis',(0.,-1.,0.));
#12017=DIRECTION('ref_axis',(1.,0.,0.));
#12018=DIRECTION('',(1.,0.,0.));
#12019=DIRECTION('',(0.,0.,1.));
#12020=DIRECTION('',(1.,0.,0.));
#12021=DIRECTION('center_axis',(-1.,0.,0.));
#12022=DIRECTION('ref_axis',(0.,-1.,0.));
#12023=DIRECTION('',(0.,-1.,0.));
#12024=DIRECTION('',(0.,-1.,0.));
#12025=DIRECTION('center_axis',(0.,0.,1.));
#12026=DIRECTION('ref_axis',(1.,0.,0.));
#12027=DIRECTION('center_axis',(0.,0.,1.));
#12028=DIRECTION('ref_axis',(1.,0.,0.));
#12029=DIRECTION('axis',(0.,0.,1.));
#12030=DIRECTION('refdir',(1.,0.,0.));
#12031=DIRECTION('center_axis',(0.,0.,-1.));
#12032=DIRECTION('ref_axis',(1.,0.,0.));
#12033=DIRECTION('center_axis',(0.,0.,-1.));
#12034=DIRECTION('ref_axis',(1.,0.,0.));
#12035=DIRECTION('',(0.,0.,-1.));
#12036=DIRECTION('center_axis',(0.,0.,1.));
#12037=DIRECTION('ref_axis',(1.,0.,0.));
#12038=DIRECTION('center_axis',(0.,1.,0.));
#12039=DIRECTION('ref_axis',(-1.,0.,0.));
#12040=DIRECTION('',(-1.,0.,0.));
#12041=DIRECTION('',(0.,0.,1.));
#12042=DIRECTION('',(-1.,0.,0.));
#12043=DIRECTION('',(0.,0.,1.));
#12044=DIRECTION('center_axis',(1.,0.,0.));
#12045=DIRECTION('ref_axis',(0.,1.,0.));
#12046=DIRECTION('',(0.,1.,0.));
#12047=DIRECTION('',(0.,1.,0.));
#12048=DIRECTION('',(0.,0.,1.));
#12049=DIRECTION('center_axis',(0.,-1.,0.));
#12050=DIRECTION('ref_axis',(1.,0.,0.));
#12051=DIRECTION('',(1.,0.,0.));
#12052=DIRECTION('',(1.,0.,0.));
#12053=DIRECTION('',(0.,0.,1.));
#12054=DIRECTION('center_axis',(-1.,0.,0.));
#12055=DIRECTION('ref_axis',(0.,-1.,0.));
#12056=DIRECTION('',(0.,-1.,0.));
#12057=DIRECTION('',(0.,-1.,0.));
#12058=DIRECTION('center_axis',(0.,0.,1.));
#12059=DIRECTION('ref_axis',(1.,0.,0.));
#12060=DIRECTION('center_axis',(0.,0.,1.));
#12061=DIRECTION('ref_axis',(1.,0.,0.));
#12062=DIRECTION('axis',(0.,0.,1.));
#12063=DIRECTION('refdir',(1.,0.,0.));
#12064=DIRECTION('center_axis',(0.,0.,1.));
#12065=DIRECTION('ref_axis',(1.,0.,0.));
#12066=DIRECTION('center_axis',(0.,0.,-1.));
#12067=DIRECTION('ref_axis',(1.,0.,0.));
#12068=DIRECTION('',(0.,0.,-1.));
#12069=DIRECTION('center_axis',(0.,0.,-1.));
#12070=DIRECTION('ref_axis',(1.,0.,0.));
#12071=DIRECTION('center_axis',(0.,0.,1.));
#12072=DIRECTION('ref_axis',(1.,0.,0.));
#12073=DIRECTION('center_axis',(0.,0.,1.));
#12074=DIRECTION('ref_axis',(1.,0.,0.));
#12075=DIRECTION('',(0.,0.,-1.));
#12076=DIRECTION('center_axis',(0.,0.,1.));
#12077=DIRECTION('ref_axis',(1.,0.,0.));
#12078=DIRECTION('center_axis',(0.,0.,1.));
#12079=DIRECTION('ref_axis',(1.,0.,0.));
#12080=DIRECTION('center_axis',(0.,0.,1.));
#12081=DIRECTION('ref_axis',(1.,0.,0.));
#12082=DIRECTION('axis',(0.,0.,1.));
#12083=DIRECTION('refdir',(1.,0.,0.));
#12084=DIRECTION('center_axis',(0.,0.,1.));
#12085=DIRECTION('ref_axis',(1.,0.,0.));
#12086=DIRECTION('center_axis',(0.,0.,1.));
#12087=DIRECTION('ref_axis',(1.,0.,0.));
#12088=DIRECTION('',(0.,0.,1.));
#12089=DIRECTION('center_axis',(0.,0.,1.));
#12090=DIRECTION('ref_axis',(1.,0.,0.));
#12091=DIRECTION('center_axis',(0.,0.,-1.));
#12092=DIRECTION('ref_axis',(-1.,0.,0.));
#12093=DIRECTION('center_axis',(0.,0.,-1.));
#12094=DIRECTION('ref_axis',(1.,0.,0.));
#12095=DIRECTION('center_axis',(0.,0.,1.));
#12096=DIRECTION('ref_axis',(1.,0.,0.));
#12097=DIRECTION('center_axis',(0.,0.,1.));
#12098=DIRECTION('ref_axis',(1.,0.,0.));
#12099=DIRECTION('center_axis',(0.,0.,1.));
#12100=DIRECTION('ref_axis',(1.,0.,0.));
#12101=DIRECTION('center_axis',(0.,0.,1.));
#12102=DIRECTION('ref_axis',(1.,0.,0.));
#12103=DIRECTION('',(0.,0.,-1.));
#12104=DIRECTION('center_axis',(0.,0.,1.));
#12105=DIRECTION('ref_axis',(1.,0.,0.));
#12106=DIRECTION('center_axis',(0.,0.,1.));
#12107=DIRECTION('ref_axis',(1.,0.,0.));
#12108=DIRECTION('center_axis',(0.,0.,1.));
#12109=DIRECTION('ref_axis',(1.,0.,0.));
#12110=DIRECTION('center_axis',(0.,0.,1.));
#12111=DIRECTION('ref_axis',(1.,0.,0.));
#12112=DIRECTION('',(0.,0.,-1.));
#12113=DIRECTION('center_axis',(0.,0.,1.));
#12114=DIRECTION('ref_axis',(1.,0.,0.));
#12115=DIRECTION('center_axis',(0.,0.,1.));
#12116=DIRECTION('ref_axis',(1.,0.,0.));
#12117=DIRECTION('center_axis',(0.,0.,1.));
#12118=DIRECTION('ref_axis',(1.,0.,0.));
#12119=DIRECTION('',(0.,0.,-1.));
#12120=DIRECTION('center_axis',(0.,0.,1.));
#12121=DIRECTION('ref_axis',(1.,0.,0.));
#12122=DIRECTION('axis',(0.,0.,1.));
#12123=DIRECTION('refdir',(1.,0.,0.));
#12124=DIRECTION('center_axis',(-1.,0.,0.));
#12125=DIRECTION('ref_axis',(0.,1.,0.));
#12126=DIRECTION('',(0.,0.,1.));
#12127=DIRECTION('',(0.,-1.,0.));
#12128=DIRECTION('',(0.,0.,-1.));
#12129=DIRECTION('',(0.,1.,0.));
#12130=DIRECTION('center_axis',(1.,0.,0.));
#12131=DIRECTION('ref_axis',(0.,-1.,0.));
#12132=DIRECTION('',(0.,0.,-1.));
#12133=DIRECTION('',(0.,-1.,0.));
#12134=DIRECTION('',(0.,0.,1.));
#12135=DIRECTION('',(0.,1.,0.));
#12136=DIRECTION('center_axis',(0.,0.,1.));
#12137=DIRECTION('ref_axis',(1.,0.,0.));
#12138=DIRECTION('center_axis',(0.,0.,1.));
#12139=DIRECTION('ref_axis',(1.,0.,0.));
#12140=DIRECTION('center_axis',(0.,0.,-1.));
#12141=DIRECTION('ref_axis',(1.,0.,0.));
#12142=DIRECTION('center_axis',(0.,0.,1.));
#12143=DIRECTION('ref_axis',(6.12323399573677E-17,-1.,0.));
#12144=DIRECTION('center_axis',(0.,0.,-1.));
#12145=DIRECTION('ref_axis',(1.,0.,0.));
#12146=DIRECTION('center_axis',(0.,0.,1.));
#12147=DIRECTION('ref_axis',(6.12323399573677E-17,-1.,0.));
#12148=DIRECTION('center_axis',(0.,0.,1.));
#12149=DIRECTION('ref_axis',(1.,0.,0.));
#12150=DIRECTION('center_axis',(0.,0.,1.));
#12151=DIRECTION('ref_axis',(1.,0.,0.));
#12152=DIRECTION('axis',(0.,0.,1.));
#12153=DIRECTION('refdir',(1.,0.,0.));
#12154=DIRECTION('center_axis',(0.,0.,-1.));
#12155=DIRECTION('ref_axis',(-1.,0.,0.));
#12156=DIRECTION('center_axis',(4.89858719658941E-16,0.,-1.));
#12157=DIRECTION('ref_axis',(-1.,0.,-4.89858719658941E-16));
#12158=DIRECTION('center_axis',(-4.89858719658941E-16,0.,1.));
#12159=DIRECTION('ref_axis',(1.,0.,4.89858719658941E-16));
#12160=DIRECTION('center_axis',(0.,0.,1.));
#12161=DIRECTION('ref_axis',(1.,0.,0.));
#12162=DIRECTION('axis',(0.,0.,1.));
#12163=DIRECTION('refdir',(1.,0.,0.));
#12164=DIRECTION('center_axis',(0.,0.,1.));
#12165=DIRECTION('ref_axis',(1.,0.,0.));
#12166=DIRECTION('center_axis',(0.,0.,-1.));
#12167=DIRECTION('ref_axis',(1.,0.,0.));
#12168=DIRECTION('',(0.,0.,-1.));
#12169=DIRECTION('center_axis',(0.,0.,-1.));
#12170=DIRECTION('ref_axis',(1.,0.,0.));
#12171=DIRECTION('center_axis',(0.,0.,1.));
#12172=DIRECTION('ref_axis',(1.,0.,0.));
#12173=DIRECTION('center_axis',(0.,0.,1.));
#12174=DIRECTION('ref_axis',(1.,0.,0.));
#12175=DIRECTION('',(0.,0.,-1.));
#12176=DIRECTION('center_axis',(0.,0.,1.));
#12177=DIRECTION('ref_axis',(1.,0.,0.));
#12178=DIRECTION('center_axis',(0.,0.,1.));
#12179=DIRECTION('ref_axis',(1.,0.,0.));
#12180=DIRECTION('center_axis',(0.,0.,1.));
#12181=DIRECTION('ref_axis',(1.,0.,0.));
#12182=DIRECTION('axis',(0.,0.,1.));
#12183=DIRECTION('refdir',(1.,0.,0.));
#12184=DIRECTION('center_axis',(0.,0.,1.));
#12185=DIRECTION('ref_axis',(1.,0.,0.));
#12186=DIRECTION('',(0.,0.,-1.));
#12187=DIRECTION('center_axis',(0.,0.,-1.));
#12188=DIRECTION('ref_axis',(1.,0.,0.));
#12189=DIRECTION('center_axis',(0.,0.,1.));
#12190=DIRECTION('ref_axis',(1.,0.,0.));
#12191=DIRECTION('',(0.,0.,-1.));
#12192=DIRECTION('center_axis',(0.,0.,1.));
#12193=DIRECTION('ref_axis',(1.,0.,0.));
#12194=DIRECTION('',(0.,0.,-1.));
#12195=DIRECTION('center_axis',(0.,0.,1.));
#12196=DIRECTION('ref_axis',(1.,0.,0.));
#12197=DIRECTION('',(0.,0.,-1.));
#12198=DIRECTION('center_axis',(0.,0.,1.));
#12199=DIRECTION('ref_axis',(1.,0.,0.));
#12200=DIRECTION('',(0.,0.,-1.));
#12201=DIRECTION('center_axis',(0.,0.,1.));
#12202=DIRECTION('ref_axis',(1.,0.,0.));
#12203=DIRECTION('',(0.,0.,-1.));
#12204=DIRECTION('center_axis',(0.,0.,1.));
#12205=DIRECTION('ref_axis',(1.,0.,0.));
#12206=DIRECTION('',(0.,0.,-1.));
#12207=DIRECTION('center_axis',(0.,0.,1.));
#12208=DIRECTION('ref_axis',(1.,0.,0.));
#12209=DIRECTION('',(0.,0.,-1.));
#12210=DIRECTION('center_axis',(0.,0.,1.));
#12211=DIRECTION('ref_axis',(1.,0.,0.));
#12212=DIRECTION('',(0.,0.,-1.));
#12213=DIRECTION('center_axis',(0.,0.,1.));
#12214=DIRECTION('ref_axis',(1.,0.,0.));
#12215=DIRECTION('',(0.,0.,-1.));
#12216=DIRECTION('center_axis',(0.,0.,1.));
#12217=DIRECTION('ref_axis',(1.,0.,0.));
#12218=DIRECTION('',(0.,0.,-1.));
#12219=DIRECTION('center_axis',(0.,0.,1.));
#12220=DIRECTION('ref_axis',(1.,0.,0.));
#12221=DIRECTION('',(0.,0.,-1.));
#12222=DIRECTION('center_axis',(0.,0.,1.));
#12223=DIRECTION('ref_axis',(1.,0.,0.));
#12224=DIRECTION('',(0.,0.,-1.));
#12225=DIRECTION('center_axis',(0.,0.,1.));
#12226=DIRECTION('ref_axis',(1.,0.,0.));
#12227=DIRECTION('',(0.,0.,-1.));
#12228=DIRECTION('center_axis',(0.,0.,1.));
#12229=DIRECTION('ref_axis',(1.,0.,0.));
#12230=DIRECTION('',(0.,0.,-1.));
#12231=DIRECTION('center_axis',(0.,0.,1.));
#12232=DIRECTION('ref_axis',(1.,0.,0.));
#12233=DIRECTION('',(0.,0.,-1.));
#12234=DIRECTION('center_axis',(0.,0.,1.));
#12235=DIRECTION('ref_axis',(1.,1.29731060939901E-13,0.));
#12236=DIRECTION('',(0.,0.,1.));
#12237=DIRECTION('center_axis',(0.,0.,-1.));
#12238=DIRECTION('ref_axis',(1.,1.29731060939901E-13,0.));
#12239=DIRECTION('center_axis',(0.,0.,1.));
#12240=DIRECTION('ref_axis',(1.,1.29731060939901E-13,0.));
#12241=DIRECTION('',(0.,0.,1.));
#12242=DIRECTION('center_axis',(0.,0.,1.));
#12243=DIRECTION('ref_axis',(1.,1.29731060939901E-13,0.));
#12244=DIRECTION('',(0.,0.,1.));
#12245=DIRECTION('center_axis',(0.,0.,1.));
#12246=DIRECTION('ref_axis',(1.,1.29731060939901E-13,0.));
#12247=DIRECTION('',(0.,0.,1.));
#12248=DIRECTION('center_axis',(0.,0.,1.));
#12249=DIRECTION('ref_axis',(1.,1.29731060939901E-13,0.));
#12250=DIRECTION('',(0.,0.,1.));
#12251=DIRECTION('center_axis',(0.,0.,1.));
#12252=DIRECTION('ref_axis',(1.,1.29731060939901E-13,0.));
#12253=DIRECTION('',(0.,0.,1.));
#12254=DIRECTION('center_axis',(0.,0.,1.));
#12255=DIRECTION('ref_axis',(1.,1.29731060939901E-13,0.));
#12256=DIRECTION('',(0.,0.,1.));
#12257=DIRECTION('center_axis',(0.,0.,1.));
#12258=DIRECTION('ref_axis',(1.,1.29731060939901E-13,0.));
#12259=DIRECTION('',(0.,0.,1.));
#12260=DIRECTION('center_axis',(0.,0.,1.));
#12261=DIRECTION('ref_axis',(1.,1.29731060939901E-13,0.));
#12262=DIRECTION('',(0.,0.,1.));
#12263=DIRECTION('center_axis',(0.,0.,1.));
#12264=DIRECTION('ref_axis',(1.,1.29731060939901E-13,0.));
#12265=DIRECTION('',(0.,0.,1.));
#12266=DIRECTION('center_axis',(0.,0.,1.));
#12267=DIRECTION('ref_axis',(1.,1.29731060939901E-13,0.));
#12268=DIRECTION('',(0.,0.,1.));
#12269=DIRECTION('center_axis',(0.,0.,1.));
#12270=DIRECTION('ref_axis',(1.,1.29731060939901E-13,0.));
#12271=DIRECTION('',(0.,0.,1.));
#12272=DIRECTION('center_axis',(0.,0.,1.));
#12273=DIRECTION('ref_axis',(1.,1.29731060939901E-13,0.));
#12274=DIRECTION('',(0.,0.,1.));
#12275=DIRECTION('center_axis',(0.,0.,1.));
#12276=DIRECTION('ref_axis',(1.,1.29731060939901E-13,0.));
#12277=DIRECTION('',(0.,0.,1.));
#12278=DIRECTION('center_axis',(0.,0.,1.));
#12279=DIRECTION('ref_axis',(1.,1.29731060939901E-13,0.));
#12280=DIRECTION('',(0.,0.,1.));
#12281=DIRECTION('center_axis',(0.,0.,1.));
#12282=DIRECTION('ref_axis',(1.,1.29731060939901E-13,0.));
#12283=DIRECTION('',(0.,0.,1.));
#12284=DIRECTION('center_axis',(0.,0.,-1.));
#12285=DIRECTION('ref_axis',(1.,0.,0.));
#12286=DIRECTION('center_axis',(0.,0.,-1.));
#12287=DIRECTION('ref_axis',(1.,0.,0.));
#12288=DIRECTION('',(0.707106781186548,8.65956056235494E-17,0.707106781186547));
#12289=DIRECTION('center_axis',(0.,0.,1.));
#12290=DIRECTION('ref_axis',(1.,0.,0.));
#12291=DIRECTION('center_axis',(0.,0.,1.));
#12292=DIRECTION('ref_axis',(1.,1.29731060939901E-13,0.));
#12293=DIRECTION('center_axis',(0.,0.,-1.));
#12294=DIRECTION('ref_axis',(1.,1.29731060939901E-13,0.));
#12295=DIRECTION('center_axis',(0.,0.,1.));
#12296=DIRECTION('ref_axis',(1.,0.,0.));
#12297=DIRECTION('center_axis',(-1.60246890531964E-16,-1.,0.));
#12298=DIRECTION('ref_axis',(1.,-1.60246890531964E-16,0.));
#12299=DIRECTION('',(1.,-1.60246890531964E-16,0.));
#12300=DIRECTION('',(0.,0.,1.));
#12301=DIRECTION('',(1.,-1.60246890531964E-16,0.));
#12302=DIRECTION('',(0.,0.,1.));
#12303=DIRECTION('center_axis',(-0.866025403784439,-0.5,0.));
#12304=DIRECTION('ref_axis',(0.5,-0.866025403784439,0.));
#12305=DIRECTION('',(0.5,-0.866025403784439,0.));
#12306=DIRECTION('',(0.,0.,1.));
#12307=DIRECTION('',(0.5,-0.866025403784439,0.));
#12308=DIRECTION('center_axis',(-0.866025403784439,0.5,0.));
#12309=DIRECTION('ref_axis',(-0.5,-0.866025403784439,0.));
#12310=DIRECTION('',(-0.5,-0.866025403784439,0.));
#12311=DIRECTION('',(0.,0.,1.));
#12312=DIRECTION('',(-0.5,-0.866025403784439,0.));
#12313=DIRECTION('center_axis',(1.60246890531964E-16,1.,0.));
#12314=DIRECTION('ref_axis',(-1.,1.60246890531964E-16,0.));
#12315=DIRECTION('',(-1.,1.60246890531964E-16,0.));
#12316=DIRECTION('',(0.,0.,1.));
#12317=DIRECTION('',(-1.,1.60246890531964E-16,0.));
#12318=DIRECTION('center_axis',(0.866025403784439,0.5,0.));
#12319=DIRECTION('ref_axis',(-0.5,0.866025403784439,0.));
#12320=DIRECTION('',(-0.5,0.866025403784439,0.));
#12321=DIRECTION('',(0.,0.,1.));
#12322=DIRECTION('',(-0.5,0.866025403784439,0.));
#12323=DIRECTION('center_axis',(0.866025403784439,-0.5,0.));
#12324=DIRECTION('ref_axis',(0.5,0.866025403784439,0.));
#12325=DIRECTION('',(0.5,0.866025403784439,0.));
#12326=DIRECTION('',(0.5,0.866025403784439,0.));
#12327=DIRECTION('center_axis',(0.,0.,1.));
#12328=DIRECTION('ref_axis',(1.,0.,0.));
#12329=DIRECTION('center_axis',(0.,0.,1.));
#12330=DIRECTION('ref_axis',(1.,0.,0.));
#12331=DIRECTION('center_axis',(0.,0.,1.));
#12332=DIRECTION('ref_axis',(1.,0.,0.));
#12333=DIRECTION('center_axis',(0.,0.,1.));
#12334=DIRECTION('ref_axis',(1.,0.,0.));
#12335=DIRECTION('',(0.,0.,-1.));
#12336=DIRECTION('center_axis',(0.,0.,1.));
#12337=DIRECTION('ref_axis',(1.,0.,0.));
#12338=DIRECTION('center_axis',(0.,0.,1.));
#12339=DIRECTION('ref_axis',(1.,0.,0.));
#12340=DIRECTION('center_axis',(0.,0.,1.));
#12341=DIRECTION('ref_axis',(1.,0.,0.));
#12342=DIRECTION('axis',(0.,0.,1.));
#12343=DIRECTION('refdir',(1.,0.,0.));
#12344=DIRECTION('center_axis',(0.,0.,1.));
#12345=DIRECTION('ref_axis',(1.,0.,0.));
#12346=DIRECTION('',(0.,0.,-1.));
#12347=DIRECTION('center_axis',(0.,0.,-1.));
#12348=DIRECTION('ref_axis',(1.,0.,0.));
#12349=DIRECTION('center_axis',(0.,0.,1.));
#12350=DIRECTION('ref_axis',(1.,0.,0.));
#12351=DIRECTION('',(0.,0.,-1.));
#12352=DIRECTION('center_axis',(0.,0.,1.));
#12353=DIRECTION('ref_axis',(1.,0.,0.));
#12354=DIRECTION('',(0.,0.,-1.));
#12355=DIRECTION('center_axis',(0.,0.,1.));
#12356=DIRECTION('ref_axis',(1.,0.,0.));
#12357=DIRECTION('',(0.,0.,-1.));
#12358=DIRECTION('center_axis',(0.,0.,1.));
#12359=DIRECTION('ref_axis',(1.,0.,0.));
#12360=DIRECTION('',(0.,0.,-1.));
#12361=DIRECTION('center_axis',(0.,0.,1.));
#12362=DIRECTION('ref_axis',(1.,0.,0.));
#12363=DIRECTION('',(0.,0.,-1.));
#12364=DIRECTION('center_axis',(0.,0.,1.));
#12365=DIRECTION('ref_axis',(1.,0.,0.));
#12366=DIRECTION('',(0.,0.,-1.));
#12367=DIRECTION('center_axis',(0.,0.,1.));
#12368=DIRECTION('ref_axis',(1.,0.,0.));
#12369=DIRECTION('',(0.,0.,-1.));
#12370=DIRECTION('center_axis',(0.,0.,1.));
#12371=DIRECTION('ref_axis',(1.,0.,0.));
#12372=DIRECTION('',(0.,0.,-1.));
#12373=DIRECTION('center_axis',(0.,0.,1.));
#12374=DIRECTION('ref_axis',(1.,0.,0.));
#12375=DIRECTION('',(0.,0.,-1.));
#12376=DIRECTION('center_axis',(0.,0.,1.));
#12377=DIRECTION('ref_axis',(1.,7.53540174823413E-14,0.));
#12378=DIRECTION('',(0.,0.,1.));
#12379=DIRECTION('center_axis',(0.,0.,-1.));
#12380=DIRECTION('ref_axis',(1.,7.53540174823413E-14,0.));
#12381=DIRECTION('center_axis',(0.,0.,1.));
#12382=DIRECTION('ref_axis',(1.,7.53540174823413E-14,0.));
#12383=DIRECTION('',(0.,0.,1.));
#12384=DIRECTION('center_axis',(0.,0.,1.));
#12385=DIRECTION('ref_axis',(1.,7.53540174823413E-14,0.));
#12386=DIRECTION('',(0.,0.,1.));
#12387=DIRECTION('center_axis',(0.,0.,1.));
#12388=DIRECTION('ref_axis',(1.,7.53540174823413E-14,0.));
#12389=DIRECTION('',(0.,0.,1.));
#12390=DIRECTION('center_axis',(0.,0.,1.));
#12391=DIRECTION('ref_axis',(1.,7.53540174823413E-14,0.));
#12392=DIRECTION('',(0.,0.,1.));
#12393=DIRECTION('center_axis',(0.,0.,1.));
#12394=DIRECTION('ref_axis',(1.,7.53540174823413E-14,0.));
#12395=DIRECTION('',(0.,0.,1.));
#12396=DIRECTION('center_axis',(0.,0.,1.));
#12397=DIRECTION('ref_axis',(1.,7.53540174823413E-14,0.));
#12398=DIRECTION('',(0.,0.,1.));
#12399=DIRECTION('center_axis',(0.,0.,1.));
#12400=DIRECTION('ref_axis',(1.,7.53540174823413E-14,0.));
#12401=DIRECTION('',(0.,0.,1.));
#12402=DIRECTION('center_axis',(0.,0.,1.));
#12403=DIRECTION('ref_axis',(1.,7.53540174823413E-14,0.));
#12404=DIRECTION('',(0.,0.,1.));
#12405=DIRECTION('center_axis',(0.,0.,1.));
#12406=DIRECTION('ref_axis',(1.,7.53540174823413E-14,0.));
#12407=DIRECTION('',(0.,0.,1.));
#12408=DIRECTION('center_axis',(0.,0.,-1.));
#12409=DIRECTION('ref_axis',(1.,0.,0.));
#12410=DIRECTION('center_axis',(0.,0.,-1.));
#12411=DIRECTION('ref_axis',(1.,0.,0.));
#12412=DIRECTION('',(0.707106781186548,8.65956056235493E-17,0.707106781186547));
#12413=DIRECTION('center_axis',(0.,0.,1.));
#12414=DIRECTION('ref_axis',(1.,0.,0.));
#12415=DIRECTION('center_axis',(0.,0.,1.));
#12416=DIRECTION('ref_axis',(1.,7.53540174823413E-14,0.));
#12417=DIRECTION('center_axis',(0.,0.,-1.));
#12418=DIRECTION('ref_axis',(1.,7.53540174823413E-14,0.));
#12419=DIRECTION('center_axis',(0.,0.,1.));
#12420=DIRECTION('ref_axis',(1.,0.,0.));
#12421=DIRECTION('center_axis',(-2.40370335797945E-16,-1.,0.));
#12422=DIRECTION('ref_axis',(1.,-2.40370335797945E-16,0.));
#12423=DIRECTION('',(1.,-2.40370335797945E-16,0.));
#12424=DIRECTION('',(0.,0.,1.));
#12425=DIRECTION('',(1.,-2.40370335797945E-16,0.));
#12426=DIRECTION('',(0.,0.,1.));
#12427=DIRECTION('center_axis',(-0.866025403784439,-0.5,0.));
#12428=DIRECTION('ref_axis',(0.5,-0.866025403784439,0.));
#12429=DIRECTION('',(0.5,-0.866025403784439,0.));
#12430=DIRECTION('',(0.,0.,1.));
#12431=DIRECTION('',(0.5,-0.866025403784439,0.));
#12432=DIRECTION('center_axis',(-0.866025403784439,0.5,0.));
#12433=DIRECTION('ref_axis',(-0.5,-0.866025403784439,0.));
#12434=DIRECTION('',(-0.5,-0.866025403784439,0.));
#12435=DIRECTION('',(0.,0.,1.));
#12436=DIRECTION('',(-0.5,-0.866025403784439,0.));
#12437=DIRECTION('center_axis',(1.20185167898973E-16,1.,0.));
#12438=DIRECTION('ref_axis',(-1.,1.20185167898973E-16,0.));
#12439=DIRECTION('',(-1.,1.20185167898973E-16,0.));
#12440=DIRECTION('',(0.,0.,1.));
#12441=DIRECTION('',(-1.,1.20185167898973E-16,0.));
#12442=DIRECTION('center_axis',(0.866025403784439,0.5,0.));
#12443=DIRECTION('ref_axis',(-0.5,0.866025403784439,0.));
#12444=DIRECTION('',(-0.5,0.866025403784439,0.));
#12445=DIRECTION('',(0.,0.,1.));
#12446=DIRECTION('',(-0.5,0.866025403784439,0.));
#12447=DIRECTION('center_axis',(0.866025403784439,-0.5,0.));
#12448=DIRECTION('ref_axis',(0.5,0.866025403784439,0.));
#12449=DIRECTION('',(0.5,0.866025403784439,0.));
#12450=DIRECTION('',(0.5,0.866025403784439,0.));
#12451=DIRECTION('center_axis',(0.,0.,1.));
#12452=DIRECTION('ref_axis',(1.,0.,0.));
#12453=DIRECTION('center_axis',(0.,0.,1.));
#12454=DIRECTION('ref_axis',(1.,0.,0.));
#12455=DIRECTION('center_axis',(0.,0.,1.));
#12456=DIRECTION('ref_axis',(1.,0.,0.));
#12457=DIRECTION('center_axis',(0.,0.,1.));
#12458=DIRECTION('ref_axis',(1.,0.,0.));
#12459=DIRECTION('',(0.,0.,-1.));
#12460=DIRECTION('center_axis',(0.,0.,1.));
#12461=DIRECTION('ref_axis',(1.,0.,0.));
#12462=DIRECTION('center_axis',(0.,0.,1.));
#12463=DIRECTION('ref_axis',(1.,0.,0.));
#12464=DIRECTION('center_axis',(0.,0.,1.));
#12465=DIRECTION('ref_axis',(1.,0.,0.));
#12466=DIRECTION('axis',(0.,0.,1.));
#12467=DIRECTION('refdir',(1.,0.,0.));
#12468=DIRECTION('center_axis',(0.,0.,1.));
#12469=DIRECTION('ref_axis',(1.,0.,0.));
#12470=DIRECTION('',(0.,0.,-1.));
#12471=DIRECTION('center_axis',(0.,0.,-1.));
#12472=DIRECTION('ref_axis',(1.,0.,0.));
#12473=DIRECTION('center_axis',(0.,0.,1.));
#12474=DIRECTION('ref_axis',(1.,0.,0.));
#12475=DIRECTION('',(0.,0.,-1.));
#12476=DIRECTION('center_axis',(0.,0.,1.));
#12477=DIRECTION('ref_axis',(1.,0.,0.));
#12478=DIRECTION('',(0.,0.,-1.));
#12479=DIRECTION('center_axis',(0.,0.,1.));
#12480=DIRECTION('ref_axis',(1.,0.,0.));
#12481=DIRECTION('',(0.,0.,-1.));
#12482=DIRECTION('center_axis',(0.,0.,1.));
#12483=DIRECTION('ref_axis',(1.,0.,0.));
#12484=DIRECTION('',(0.,0.,-1.));
#12485=DIRECTION('center_axis',(0.,0.,1.));
#12486=DIRECTION('ref_axis',(1.,0.,0.));
#12487=DIRECTION('',(0.,0.,-1.));
#12488=DIRECTION('center_axis',(0.,0.,1.));
#12489=DIRECTION('ref_axis',(1.,0.,0.));
#12490=DIRECTION('',(0.,0.,-1.));
#12491=DIRECTION('center_axis',(0.,0.,1.));
#12492=DIRECTION('ref_axis',(1.,0.,0.));
#12493=DIRECTION('',(0.,0.,-1.));
#12494=DIRECTION('center_axis',(0.,0.,1.));
#12495=DIRECTION('ref_axis',(1.,0.,0.));
#12496=DIRECTION('',(0.,0.,-1.));
#12497=DIRECTION('center_axis',(0.,0.,1.));
#12498=DIRECTION('ref_axis',(1.,0.,0.));
#12499=DIRECTION('',(0.,0.,-1.));
#12500=DIRECTION('center_axis',(0.,0.,1.));
#12501=DIRECTION('ref_axis',(1.,0.,0.));
#12502=DIRECTION('',(0.,0.,-1.));
#12503=DIRECTION('center_axis',(0.,0.,1.));
#12504=DIRECTION('ref_axis',(1.,0.,0.));
#12505=DIRECTION('',(0.,0.,-1.));
#12506=DIRECTION('center_axis',(0.,0.,1.));
#12507=DIRECTION('ref_axis',(1.,0.,0.));
#12508=DIRECTION('',(0.,0.,-1.));
#12509=DIRECTION('center_axis',(0.,0.,1.));
#12510=DIRECTION('ref_axis',(1.,0.,0.));
#12511=DIRECTION('',(0.,0.,-1.));
#12512=DIRECTION('center_axis',(0.,0.,1.));
#12513=DIRECTION('ref_axis',(1.,0.,0.));
#12514=DIRECTION('',(0.,0.,-1.));
#12515=DIRECTION('center_axis',(0.,0.,1.));
#12516=DIRECTION('ref_axis',(1.,0.,0.));
#12517=DIRECTION('',(0.,0.,-1.));
#12518=DIRECTION('center_axis',(0.,0.,1.));
#12519=DIRECTION('ref_axis',(1.,0.,0.));
#12520=DIRECTION('',(0.,0.,-1.));
#12521=DIRECTION('center_axis',(0.,0.,1.));
#12522=DIRECTION('ref_axis',(1.,0.,0.));
#12523=DIRECTION('',(0.,0.,-1.));
#12524=DIRECTION('center_axis',(0.,0.,1.));
#12525=DIRECTION('ref_axis',(1.,1.10671505702589E-13,0.));
#12526=DIRECTION('',(0.,0.,1.));
#12527=DIRECTION('center_axis',(0.,0.,-1.));
#12528=DIRECTION('ref_axis',(1.,1.10671505702589E-13,0.));
#12529=DIRECTION('center_axis',(0.,0.,1.));
#12530=DIRECTION('ref_axis',(1.,1.10671505702589E-13,0.));
#12531=DIRECTION('',(0.,0.,1.));
#12532=DIRECTION('center_axis',(0.,0.,1.));
#12533=DIRECTION('ref_axis',(1.,1.10671505702589E-13,0.));
#12534=DIRECTION('',(0.,0.,1.));
#12535=DIRECTION('center_axis',(0.,0.,1.));
#12536=DIRECTION('ref_axis',(1.,1.10671505702589E-13,0.));
#12537=DIRECTION('',(0.,0.,1.));
#12538=DIRECTION('center_axis',(0.,0.,1.));
#12539=DIRECTION('ref_axis',(1.,1.10671505702589E-13,0.));
#12540=DIRECTION('',(0.,0.,1.));
#12541=DIRECTION('center_axis',(0.,0.,1.));
#12542=DIRECTION('ref_axis',(1.,1.10671505702589E-13,0.));
#12543=DIRECTION('',(0.,0.,1.));
#12544=DIRECTION('center_axis',(0.,0.,1.));
#12545=DIRECTION('ref_axis',(1.,1.10671505702589E-13,0.));
#12546=DIRECTION('',(0.,0.,1.));
#12547=DIRECTION('center_axis',(0.,0.,1.));
#12548=DIRECTION('ref_axis',(1.,1.10671505702589E-13,0.));
#12549=DIRECTION('',(0.,0.,1.));
#12550=DIRECTION('center_axis',(0.,0.,1.));
#12551=DIRECTION('ref_axis',(1.,1.10671505702589E-13,0.));
#12552=DIRECTION('',(0.,0.,1.));
#12553=DIRECTION('center_axis',(0.,0.,1.));
#12554=DIRECTION('ref_axis',(1.,1.10671505702589E-13,0.));
#12555=DIRECTION('',(0.,0.,1.));
#12556=DIRECTION('center_axis',(0.,0.,1.));
#12557=DIRECTION('ref_axis',(1.,1.10671505702589E-13,0.));
#12558=DIRECTION('',(0.,0.,1.));
#12559=DIRECTION('center_axis',(0.,0.,1.));
#12560=DIRECTION('ref_axis',(1.,1.10671505702589E-13,0.));
#12561=DIRECTION('',(0.,0.,1.));
#12562=DIRECTION('center_axis',(0.,0.,1.));
#12563=DIRECTION('ref_axis',(1.,1.10671505702589E-13,0.));
#12564=DIRECTION('',(0.,0.,1.));
#12565=DIRECTION('center_axis',(0.,0.,1.));
#12566=DIRECTION('ref_axis',(1.,1.10671505702589E-13,0.));
#12567=DIRECTION('',(0.,0.,1.));
#12568=DIRECTION('center_axis',(0.,0.,1.));
#12569=DIRECTION('ref_axis',(1.,1.10671505702589E-13,0.));
#12570=DIRECTION('',(0.,0.,1.));
#12571=DIRECTION('center_axis',(0.,0.,1.));
#12572=DIRECTION('ref_axis',(1.,1.10671505702589E-13,0.));
#12573=DIRECTION('',(0.,0.,1.));
#12574=DIRECTION('center_axis',(0.,0.,1.));
#12575=DIRECTION('ref_axis',(1.,1.10671505702589E-13,0.));
#12576=DIRECTION('',(0.,0.,1.));
#12577=DIRECTION('center_axis',(0.,0.,1.));
#12578=DIRECTION('ref_axis',(1.,1.10671505702589E-13,0.));
#12579=DIRECTION('',(0.,0.,1.));
#12580=DIRECTION('center_axis',(0.,0.,-1.));
#12581=DIRECTION('ref_axis',(1.,0.,0.));
#12582=DIRECTION('center_axis',(0.,0.,-1.));
#12583=DIRECTION('ref_axis',(1.,0.,0.));
#12584=DIRECTION('',(0.707106781186548,8.65956056235493E-17,0.707106781186547));
#12585=DIRECTION('center_axis',(0.,0.,1.));
#12586=DIRECTION('ref_axis',(1.,0.,0.));
#12587=DIRECTION('center_axis',(0.,0.,1.));
#12588=DIRECTION('ref_axis',(1.,1.10671505702589E-13,0.));
#12589=DIRECTION('center_axis',(0.,0.,-1.));
#12590=DIRECTION('ref_axis',(1.,1.10671505702589E-13,0.));
#12591=DIRECTION('center_axis',(0.,0.,1.));
#12592=DIRECTION('ref_axis',(1.,0.,0.));
#12593=DIRECTION('center_axis',(-2.40370335797945E-16,-1.,0.));
#12594=DIRECTION('ref_axis',(1.,-2.40370335797945E-16,0.));
#12595=DIRECTION('',(1.,-2.40370335797945E-16,0.));
#12596=DIRECTION('',(0.,0.,1.));
#12597=DIRECTION('',(1.,-2.40370335797945E-16,0.));
#12598=DIRECTION('',(0.,0.,1.));
#12599=DIRECTION('center_axis',(-0.866025403784439,-0.5,0.));
#12600=DIRECTION('ref_axis',(0.5,-0.866025403784439,0.));
#12601=DIRECTION('',(0.5,-0.866025403784439,0.));
#12602=DIRECTION('',(0.,0.,1.));
#12603=DIRECTION('',(0.5,-0.866025403784439,0.));
#12604=DIRECTION('center_axis',(-0.866025403784439,0.5,0.));
#12605=DIRECTION('ref_axis',(-0.5,-0.866025403784439,0.));
#12606=DIRECTION('',(-0.5,-0.866025403784439,0.));
#12607=DIRECTION('',(0.,0.,1.));
#12608=DIRECTION('',(-0.5,-0.866025403784439,0.));
#12609=DIRECTION('center_axis',(1.20185167898973E-16,1.,0.));
#12610=DIRECTION('ref_axis',(-1.,1.20185167898973E-16,0.));
#12611=DIRECTION('',(-1.,1.20185167898973E-16,0.));
#12612=DIRECTION('',(0.,0.,1.));
#12613=DIRECTION('',(-1.,1.20185167898973E-16,0.));
#12614=DIRECTION('center_axis',(0.866025403784439,0.5,0.));
#12615=DIRECTION('ref_axis',(-0.5,0.866025403784439,0.));
#12616=DIRECTION('',(-0.5,0.866025403784439,0.));
#12617=DIRECTION('',(0.,0.,1.));
#12618=DIRECTION('',(-0.5,0.866025403784439,0.));
#12619=DIRECTION('center_axis',(0.866025403784439,-0.5,0.));
#12620=DIRECTION('ref_axis',(0.5,0.866025403784439,0.));
#12621=DIRECTION('',(0.5,0.866025403784439,0.));
#12622=DIRECTION('',(0.5,0.866025403784439,0.));
#12623=DIRECTION('center_axis',(0.,0.,1.));
#12624=DIRECTION('ref_axis',(1.,0.,0.));
#12625=DIRECTION('center_axis',(0.,0.,1.));
#12626=DIRECTION('ref_axis',(1.,0.,0.));
#12627=DIRECTION('center_axis',(0.,0.,1.));
#12628=DIRECTION('ref_axis',(1.,0.,0.));
#12629=DIRECTION('center_axis',(0.,0.,1.));
#12630=DIRECTION('ref_axis',(1.,0.,0.));
#12631=DIRECTION('',(0.,0.,-1.));
#12632=DIRECTION('center_axis',(0.,0.,1.));
#12633=DIRECTION('ref_axis',(1.,0.,0.));
#12634=DIRECTION('center_axis',(0.,0.,1.));
#12635=DIRECTION('ref_axis',(1.,0.,0.));
#12636=DIRECTION('center_axis',(0.,0.,1.));
#12637=DIRECTION('ref_axis',(1.,0.,0.));
#12638=DIRECTION('',(0.,0.,1.));
#12639=DIRECTION('',(1.,0.,0.));
#12640=DIRECTION('',(0.,0.,1.));
#12641=DIRECTION('',(1.,0.,0.));
#12642=DIRECTION('',(0.,1.,0.));
#12643=DIRECTION('',(1.,0.,0.));
#12644=DIRECTION('',(0.,0.,1.));
#12645=DIRECTION('',(1.,0.,0.));
#12646=DIRECTION('',(0.,0.,1.));
#12647=DIRECTION('',(1.,0.,0.));
#12648=DIRECTION('',(0.,0.,1.));
#12649=DIRECTION('',(1.,0.,0.));
#12650=DIRECTION('',(0.,0.,1.));
#12651=DIRECTION('',(1.,0.,0.));
#12652=DIRECTION('',(0.,0.,1.));
#12653=DIRECTION('',(1.,0.,0.));
#12654=DIRECTION('',(1.,0.,0.));
#12655=DIRECTION('',(0.,1.,0.));
#12656=DIRECTION('',(0.,0.,1.));
#12657=DIRECTION('',(1.,0.,0.));
#12658=DIRECTION('',(0.,0.,1.));
#12659=DIRECTION('',(-1.,1.22464679914735E-16,0.));
#12660=DIRECTION('',(0.,0.,1.));
#12661=DIRECTION('',(1.,0.,0.));
#12662=DIRECTION('',(1.,0.,0.));
#12663=DIRECTION('',(0.,1.,0.));
#12664=DIRECTION('',(1.,0.,0.));
#12665=DIRECTION('',(0.,1.,0.));
#12666=DIRECTION('',(1.,0.,0.));
#12667=DIRECTION('',(0.,1.,0.));
#12668=DIRECTION('',(1.,0.,0.));
#12669=DIRECTION('',(0.,1.,0.));
#12670=DIRECTION('',(0.,-1.,0.));
#12671=DIRECTION('',(1.,0.,0.));
#12672=DIRECTION('',(1.,0.,0.));
#12673=DIRECTION('',(0.,1.,0.));
#12674=DIRECTION('',(1.,0.,0.));
#12675=DIRECTION('',(0.,1.,0.));
#12676=DIRECTION('',(0.,-1.22464679914735E-16,-1.));
#12677=DIRECTION('',(-0.766044443118978,-0.64278760968654,7.87187788734199E-17));
#12678=DIRECTION('',(0.,-1.22464679914735E-16,-1.));
#12679=DIRECTION('',(1.,0.,0.));
#12680=DIRECTION('',(0.,-1.22464679914735E-16,-1.));
#12681=DIRECTION('',(1.,0.,0.));
#12682=DIRECTION('',(0.,-1.22464679914735E-16,-1.));
#12683=DIRECTION('',(-0.766044443118978,-0.64278760968654,7.87187788734199E-17));
#12684=DIRECTION('',(0.,-1.22464679914735E-16,-1.));
#12685=DIRECTION('',(-0.766044443118978,-0.64278760968654,7.87187788734199E-17));
#12686=DIRECTION('',(0.,-1.22464679914735E-16,-1.));
#12687=DIRECTION('',(-0.766044443118978,-0.64278760968654,7.87187788734199E-17));
#12688=DIRECTION('',(0.,-2.46519032881566E-32,1.));
#12689=DIRECTION('',(-2.77555756156289E-16,-1.,0.));
#12690=DIRECTION('',(0.,-2.46519032881566E-32,1.));
#12691=DIRECTION('',(-2.77555756156289E-16,-1.,0.));
#12692=DIRECTION('',(0.,-1.22464679914735E-16,-1.));
#12693=DIRECTION('',(1.,0.,0.));
#12694=DIRECTION('',(1.49975978266186E-32,1.22464679914735E-16,-1.));
#12695=DIRECTION('',(-1.,1.22464679914735E-16,0.));
#12696=DIRECTION('',(0.,-1.22464679914735E-16,-1.));
#12697=DIRECTION('',(1.,0.,0.));
#12698=DIRECTION('',(0.,-1.22464679914735E-16,-1.));
#12699=DIRECTION('',(1.,0.,0.));
#12700=CARTESIAN_POINT('',(0.,0.,0.));
#12701=CARTESIAN_POINT('',(0.,0.,0.));
#12702=CARTESIAN_POINT('Origin',(3.6,2.4,4.7));
#12703=CARTESIAN_POINT('',(3.43324411482341,2.39987855685961,4.38714803633902));
#12704=CARTESIAN_POINT('',(3.43319917606922,2.4000969362753,4.36785196366098));
#12705=CARTESIAN_POINT('',(3.4334,2.4,4.7));
#12706=CARTESIAN_POINT('',(3.43648706727485,2.36807695453719,4.3));
#12707=CARTESIAN_POINT('Ctrl Pts',(3.43319917606922,2.4000969362753,4.36785196366098));
#12708=CARTESIAN_POINT('Ctrl Pts',(3.43315841823699,2.40590556741068,4.36746222055426));
#12709=CARTESIAN_POINT('Ctrl Pts',(3.43343543893775,2.41171030674387,4.36707247744754));
#12710=CARTESIAN_POINT('Ctrl Pts',(3.43404307301465,2.41748025740019,4.36668273434083));
#12711=CARTESIAN_POINT('Ctrl Pts',(3.43981877230484,2.47232494300381,4.36297813798856));
#12712=CARTESIAN_POINT('Ctrl Pts',(3.475465166407,2.52402649519299,4.35927354163629));
#12713=CARTESIAN_POINT('Ctrl Pts',(3.52467802575654,2.54891438715568,4.35556894528402));
#12714=CARTESIAN_POINT('Ctrl Pts',(3.57389088510608,2.57380227911837,4.35186434893175));
#12715=CARTESIAN_POINT('Ctrl Pts',(3.636670209703,2.57187651085455,4.34815975257948));
#12716=CARTESIAN_POINT('Ctrl Pts',(3.68426556342447,2.54403648109996,4.34445515622722));
#12717=CARTESIAN_POINT('Ctrl Pts',(3.73186091714595,2.51619645134536,4.34075055987495));
#12718=CARTESIAN_POINT('Ctrl Pts',(3.76427229999197,2.46244216009999,4.33704596352268));
#12719=CARTESIAN_POINT('Ctrl Pts',(3.76670490932883,2.40733835348838,4.33334136717041));
#12720=CARTESIAN_POINT('Ctrl Pts',(3.76913751866569,2.35223454687676,4.32963677081814));
#12721=CARTESIAN_POINT('Ctrl Pts',(3.74159135449339,2.29578122489891,4.32593217446588));
#12722=CARTESIAN_POINT('Ctrl Pts',(3.69659413605431,2.26388777656513,4.32222757811361));
#12723=CARTESIAN_POINT('Ctrl Pts',(3.65159691761524,2.23199432823136,4.31852298176134));
#12724=CARTESIAN_POINT('Ctrl Pts',(3.5891486449094,2.22466075354166,4.31481838540907));
#12725=CARTESIAN_POINT('Ctrl Pts',(3.53802497534865,2.24508842505152,4.3111137890568));
#12726=CARTESIAN_POINT('Ctrl Pts',(3.4869013057879,2.26551609656139,4.30740919270454));
#12727=CARTESIAN_POINT('Ctrl Pts',(3.44710223937223,2.31370501427082,4.30370459635227));
#12728=CARTESIAN_POINT('Ctrl Pts',(3.43648706727485,2.36807695453719,4.3));
#12729=CARTESIAN_POINT('',(3.5947433343941,2.5668198697629,4.3));
#12730=CARTESIAN_POINT('Origin',(3.6,2.4,4.3));
#12731=CARTESIAN_POINT('',(3.43365448824955,2.39993503013922,4.31714803633902));
#12732=CARTESIAN_POINT('Ctrl Pts',(3.59474333802771,2.56682006235004,4.3));
#12733=CARTESIAN_POINT('Ctrl Pts',(3.54069368762274,2.56504680898901,4.30363229181856));
#12734=CARTESIAN_POINT('Ctrl Pts',(3.48748281235487,2.53457817870515,4.30726458363711));
#12735=CARTESIAN_POINT('Ctrl Pts',(3.45871386452964,2.48878411340601,4.31089687545566));
#12736=CARTESIAN_POINT('Ctrl Pts',(3.44221011333674,2.46251364065879,4.31298059575012));
#12737=CARTESIAN_POINT('Ctrl Pts',(3.43375000591375,2.43119968923457,4.31506431604457));
#12738=CARTESIAN_POINT('Ctrl Pts',(3.43365448824955,2.39993503013922,4.31714803633902));
#12739=CARTESIAN_POINT('',(3.4334,2.4,4.2));
#12740=CARTESIAN_POINT('',(3.4334,2.4,4.7));
#12741=CARTESIAN_POINT('Origin',(3.6,2.4,4.2));
#12742=CARTESIAN_POINT('Ctrl Pts',(3.43365448824955,2.39993503013922,4.31714803633902));
#12743=CARTESIAN_POINT('Ctrl Pts',(3.4335801873487,2.37561500142982,4.31876891239684));
#12744=CARTESIAN_POINT('Ctrl Pts',(3.43856722533918,2.35132479907035,4.32038978845465));
#12745=CARTESIAN_POINT('Ctrl Pts',(3.44876666696164,2.32946151839122,4.32201066451247));
#12746=CARTESIAN_POINT('Ctrl Pts',(3.47207802013238,2.27949185571287,4.32571526086474));
#12747=CARTESIAN_POINT('Ctrl Pts',(3.52261765366037,2.24219981905568,4.32941985721701));
#12748=CARTESIAN_POINT('Ctrl Pts',(3.57725038766107,2.23467802743392,4.33312445356927));
#12749=CARTESIAN_POINT('Ctrl Pts',(3.63188312166177,2.22715623581217,4.33682904992154));
#12750=CARTESIAN_POINT('Ctrl Pts',(3.69060895613519,2.24940468922586,4.34053364627381));
#12751=CARTESIAN_POINT('Ctrl Pts',(3.72655438764877,2.29122842499976,4.34423824262608));
#12752=CARTESIAN_POINT('Ctrl Pts',(3.76249981916235,2.33305216077365,4.34794283897835));
#12753=CARTESIAN_POINT('Ctrl Pts',(3.77566484771609,2.39445117890775,4.35164743533062));
#12754=CARTESIAN_POINT('Ctrl Pts',(3.76002307153489,2.44733227776831,4.35535203168288));
#12755=CARTESIAN_POINT('Ctrl Pts',(3.7443812953537,2.50021337662887,4.35905662803515));
#12756=CARTESIAN_POINT('Ctrl Pts',(3.69993271443756,2.5445765562159,4.36276122438742));
#12757=CARTESIAN_POINT('Ctrl Pts',(3.64702014888419,2.56011555645441,4.36646582073968));
#12758=CARTESIAN_POINT('Ctrl Pts',(3.59410758333083,2.57565455669293,4.37017041709195));
#12759=CARTESIAN_POINT('Ctrl Pts',(3.53273103314024,2.56236937758293,4.37387501344422));
#12760=CARTESIAN_POINT('Ctrl Pts',(3.49097948747713,2.52634165427837,4.37757960979649));
#12761=CARTESIAN_POINT('Ctrl Pts',(3.45503345721934,2.49532355395523,4.38076908531067));
#12762=CARTESIAN_POINT('Ctrl Pts',(3.43363419524109,2.44744785138174,4.38395856082484));
#12763=CARTESIAN_POINT('Ctrl Pts',(3.43324411482341,2.39987855685961,4.38714803633902));
#12764=CARTESIAN_POINT('Origin',(3.6,2.4,4.7));
#12765=CARTESIAN_POINT('',(3.43327529856389,2.40013247750357,4.45714803633902));
#12766=CARTESIAN_POINT('',(3.43362892985438,2.40008323250784,4.43785196366098));
#12767=CARTESIAN_POINT('',(3.4334,2.4,4.7));
#12768=CARTESIAN_POINT('Ctrl Pts',(3.43362892985438,2.40008323250784,4.43785196366098));
#12769=CARTESIAN_POINT('Ctrl Pts',(3.43352744619908,2.42251958229607,4.43635646533454));
#12770=CARTESIAN_POINT('Ctrl Pts',(3.43774838281902,2.44491933756368,4.43486096700809));
#12771=CARTESIAN_POINT('Ctrl Pts',(3.44647310901037,2.4654005396039,4.43336546868165));
#12772=CARTESIAN_POINT('Ctrl Pts',(3.46808569676891,2.5161358597488,4.42966087232938));
#12773=CARTESIAN_POINT('Ctrl Pts',(3.51733510120548,2.55509827110394,4.42595627597712));
#12774=CARTESIAN_POINT('Ctrl Pts',(3.57168220127168,2.56445626518835,4.42225167962485));
#12775=CARTESIAN_POINT('Ctrl Pts',(3.62602930133789,2.57381425927275,4.41854708327258));
#12776=CARTESIAN_POINT('Ctrl Pts',(3.68547409703373,2.55356783608644,4.41484248692031));
#12777=CARTESIAN_POINT('Ctrl Pts',(3.7228110439026,2.51298316629394,4.41113789056804));
#12778=CARTESIAN_POINT('Ctrl Pts',(3.76014799077148,2.47239849650144,4.40743329421577));
#12779=CARTESIAN_POINT('Ctrl Pts',(3.77537708881339,2.41147558010275,4.4037286978635));
#12780=CARTESIAN_POINT('Ctrl Pts',(3.76152924886074,2.35809557405986,4.40002410151124));
#12781=CARTESIAN_POINT('Ctrl Pts',(3.74768140890809,2.30471556801697,4.39631950515897));
#12782=CARTESIAN_POINT('Ctrl Pts',(3.70475663096088,2.25887847232986,4.3926149088067));
#12783=CARTESIAN_POINT('Ctrl Pts',(3.65239849394634,2.24156301733926,4.38891031245443));
#12784=CARTESIAN_POINT('Ctrl Pts',(3.6000403569318,2.22424756234866,4.38520571610217));
#12785=CARTESIAN_POINT('Ctrl Pts',(3.53824886084993,2.23545374805455,4.3815011197499));
#12786=CARTESIAN_POINT('Ctrl Pts',(3.49530561504809,2.27005075041653,4.37779652339763));
#12787=CARTESIAN_POINT('Ctrl Pts',(3.45688022556308,2.30100796536268,4.37448167015208));
#12788=CARTESIAN_POINT('Ctrl Pts',(3.43354583064794,2.35069321510765,4.37116681690653));
#12789=CARTESIAN_POINT('Ctrl Pts',(3.43319917606922,2.4000969362753,4.36785196366098));
#12790=CARTESIAN_POINT('Ctrl Pts',(3.43324411482341,2.39987855685961,4.38714803633902));
#12791=CARTESIAN_POINT('Ctrl Pts',(3.43318111432356,2.39219580941329,4.38766315717711));
#12792=CARTESIAN_POINT('Ctrl Pts',(3.4336661242569,2.38452105441581,4.3881782780152));
#12793=CARTESIAN_POINT('Ctrl Pts',(3.43472636939645,2.37692660019285,4.38869339885329));
#12794=CARTESIAN_POINT('Ctrl Pts',(3.44235133811452,2.32230953691099,4.39239799520556));
#12795=CARTESIAN_POINT('Ctrl Pts',(3.47972781668628,2.27184567784637,4.39610259155783));
#12796=CARTESIAN_POINT('Ctrl Pts',(3.52975016370933,2.24863049260891,4.3998071879101));
#12797=CARTESIAN_POINT('Ctrl Pts',(3.57977251073239,2.22541530737146,4.40351178426237));
#12798=CARTESIAN_POINT('Ctrl Pts',(3.64244072620675,2.22944879596115,4.40721638061463));
#12799=CARTESIAN_POINT('Ctrl Pts',(3.6890743879353,2.25888481053352,4.4109209769669));
#12800=CARTESIAN_POINT('Ctrl Pts',(3.73570804966386,2.28832082510588,4.41462557331917));
#12801=CARTESIAN_POINT('Ctrl Pts',(3.76630715764661,2.34315936566092,4.41833016967144));
#12802=CARTESIAN_POINT('Ctrl Pts',(3.76686783565003,2.39830336248822,4.4220347660237));
#12803=CARTESIAN_POINT('Ctrl Pts',(3.76742851365345,2.45344735931552,4.42573936237597));
#12804=CARTESIAN_POINT('Ctrl Pts',(3.73795076167754,2.5088968124151,4.42944395872824));
#12805=CARTESIAN_POINT('Ctrl Pts',(3.69192525052887,2.53927491555576,4.43314855508051));
#12806=CARTESIAN_POINT('Ctrl Pts',(3.6458997393802,2.56965301869642,4.43685315143278));
#12807=CARTESIAN_POINT('Ctrl Pts',(3.58332646905877,2.57495977187817,4.44055774778505));
#12808=CARTESIAN_POINT('Ctrl Pts',(3.5328424463163,2.55276653418389,4.44426234413732));
#12809=CARTESIAN_POINT('Ctrl Pts',(3.48235842357382,2.53057329648961,4.44796694048958));
#12810=CARTESIAN_POINT('Ctrl Pts',(3.4439636484103,2.4808800679193,4.45167153684185));
#12811=CARTESIAN_POINT('Ctrl Pts',(3.43522971000183,2.42642922394017,4.45537613319412));
#12812=CARTESIAN_POINT('Ctrl Pts',(3.43383723324577,2.41774797030146,4.45596676757575));
#12813=CARTESIAN_POINT('Ctrl Pts',(3.43319870043454,2.40894578361697,4.45655740195739));
#12814=CARTESIAN_POINT('Ctrl Pts',(3.43327529856389,2.40013247750357,4.45714803633902));
#12815=CARTESIAN_POINT('Origin',(3.6,2.4,4.7));
#12816=CARTESIAN_POINT('',(3.43366207255012,2.4000380247868,4.52714803633902));
#12817=CARTESIAN_POINT('',(3.43350143198867,2.39985687063426,4.50785196366098));
#12818=CARTESIAN_POINT('',(3.4334,2.4,4.7));
#12819=CARTESIAN_POINT('Ctrl Pts',(3.43350143198867,2.39985687063426,4.50785196366098));
#12820=CARTESIAN_POINT('Ctrl Pts',(3.43382054827219,2.43880728393095,4.50525071011481));
#12821=CARTESIAN_POINT('Ctrl Pts',(3.44745633991989,2.47795898515992,4.50264945656865));
#12822=CARTESIAN_POINT('Ctrl Pts',(3.47241574712106,2.50756395301054,4.50004820302248));
#12823=CARTESIAN_POINT('Ctrl Pts',(3.50796188948324,2.54972610827987,4.49634360667021));
#12824=CARTESIAN_POINT('Ctrl Pts',(3.56647488720154,2.57252532742787,4.49263901031794));
#12825=CARTESIAN_POINT('Ctrl Pts',(3.62117593737884,2.56552741635789,4.48893441396567));
#12826=CARTESIAN_POINT('Ctrl Pts',(3.67587698755613,2.55852950528791,4.4852298176134));
#12827=CARTESIAN_POINT('Ctrl Pts',(3.72676609019243,2.52173446399995,4.48152522126113));
#12828=CARTESIAN_POINT('Ctrl Pts',(3.75055355430056,2.47198175613265,4.47782062490887));
#12829=CARTESIAN_POINT('Ctrl Pts',(3.77434101840868,2.42222904826535,4.4741160285566));
#12830=CARTESIAN_POINT('Ctrl Pts',(3.77102684398863,2.3595186738187,4.47041143220433));
#12831=CARTESIAN_POINT('Ctrl Pts',(3.74212779097605,2.31255038253853,4.46670683585206));
#12832=CARTESIAN_POINT('Ctrl Pts',(3.71322873796346,2.26558209125837,4.4630022394998));
#12833=CARTESIAN_POINT('Ctrl Pts',(3.65874480635833,2.23435588314469,4.45929764314753));
#12834=CARTESIAN_POINT('Ctrl Pts',(3.60361085794536,2.23316262684763,4.45559304679526));
#12835=CARTESIAN_POINT('Ctrl Pts',(3.54847690953239,2.23196937055057,4.45188845044299));
#12836=CARTESIAN_POINT('Ctrl Pts',(3.49269294431159,2.26080906607012,4.44818385409072));
#12837=CARTESIAN_POINT('Ctrl Pts',(3.46178884724144,2.30648302829723,4.44447925773845));
#12838=CARTESIAN_POINT('Ctrl Pts',(3.44336034023669,2.33371899416048,4.44227015971263));
#12839=CARTESIAN_POINT('Ctrl Pts',(3.43377883797438,2.36694103826561,4.44006106168681));
#12840=CARTESIAN_POINT('Ctrl Pts',(3.43362892985438,2.40008323250784,4.43785196366098));
#12841=CARTESIAN_POINT('Ctrl Pts',(3.43327529856389,2.40013247750357,4.45714803633902));
#12842=CARTESIAN_POINT('Ctrl Pts',(3.43367914173529,2.35366667577227,4.46026199830965));
#12843=CARTESIAN_POINT('Ctrl Pts',(3.45396107839716,2.3068917935147,4.46337596028029));
#12844=CARTESIAN_POINT('Ctrl Pts',(3.48843309004669,2.27590093912579,4.46648992225093));
#12845=CARTESIAN_POINT('Ctrl Pts',(3.52944351015346,2.23903195767851,4.47019451860319));
#12846=CARTESIAN_POINT('Ctrl Pts',(3.59053745202041,2.22450245417194,4.47389911495546));
#12847=CARTESIAN_POINT('Ctrl Pts',(3.64375492737657,2.23896193518984,4.47760371130773));
#12848=CARTESIAN_POINT('Ctrl Pts',(3.69697240273272,2.25342141620775,4.48130830765999));
#12849=CARTESIAN_POINT('Ctrl Pts',(3.74231341157808,2.29686988175014,4.48501290401227));
#12850=CARTESIAN_POINT('Ctrl Pts',(3.75902738378866,2.34942289673192,4.48871750036453));
#12851=CARTESIAN_POINT('Ctrl Pts',(3.77574135599923,2.40197591171369,4.4924220967168));
#12852=CARTESIAN_POINT('Ctrl Pts',(3.76382829157503,2.46363347613485,4.49612669306907));
#12853=CARTESIAN_POINT('Ctrl Pts',(3.7287402721637,2.50617765524692,4.49983128942134));
#12854=CARTESIAN_POINT('Ctrl Pts',(3.69365225275236,2.54872183435899,4.5035358857736));
#12855=CARTESIAN_POINT('Ctrl Pts',(3.63538927835389,2.57215262816197,4.50724048212587));
#12856=CARTESIAN_POINT('Ctrl Pts',(3.58061572949426,2.56574680139426,4.51094507847814));
#12857=CARTESIAN_POINT('Ctrl Pts',(3.52584218063463,2.55934097462656,4.51464967483041));
#12858=CARTESIAN_POINT('Ctrl Pts',(3.47455805731385,2.52309852728818,4.51835427118268));
#12859=CARTESIAN_POINT('Ctrl Pts',(3.45023382941089,2.47360602072044,4.52205886753494));
#12860=CARTESIAN_POINT('Ctrl Pts',(3.43909540477512,2.45094266808951,4.5237552571363));
#12861=CARTESIAN_POINT('Ctrl Pts',(3.43361009249165,2.42550096367579,4.52545164673766));
#12862=CARTESIAN_POINT('Ctrl Pts',(3.43366207255012,2.4000380247868,4.52714803633902));
#12863=CARTESIAN_POINT('Origin',(3.6,2.4,4.7));
#12864=CARTESIAN_POINT('',(3.43341474631901,2.39984765669014,4.59714803633902));
#12865=CARTESIAN_POINT('',(3.43312356359968,2.40000067112034,4.57785196366098));
#12866=CARTESIAN_POINT('',(3.4334,2.4,4.7));
#12867=CARTESIAN_POINT('Ctrl Pts',(3.43312356496403,2.40000067111703,4.57785196366098));
#12868=CARTESIAN_POINT('Ctrl Pts',(3.43312026903532,2.45518344011976,4.57414495489509));
#12869=CARTESIAN_POINT('Ctrl Pts',(3.46320502523792,2.51036311996034,4.5704379461292));
#12870=CARTESIAN_POINT('Ctrl Pts',(3.50958660620738,2.54026105638185,4.5667309373633));
#12871=CARTESIAN_POINT('Ctrl Pts',(3.55593800339121,2.57013953609479,4.56302634101103));
#12872=CARTESIAN_POINT('Ctrl Pts',(3.6185650095987,2.57476916693782,4.55932174465876));
#12873=CARTESIAN_POINT('Ctrl Pts',(3.66880602035543,2.55203117207009,4.55561714830649));
#12874=CARTESIAN_POINT('Ctrl Pts',(3.71904703111215,2.52929317720236,4.55191255195423));
#12875=CARTESIAN_POINT('Ctrl Pts',(3.7569020464181,2.47918755662387,4.54820795560196));
#12876=CARTESIAN_POINT('Ctrl Pts',(3.76504650379449,2.42464543177811,4.54450335924969));
#12877=CARTESIAN_POINT('Ctrl Pts',(3.77319096117088,2.37010330693235,4.54079876289743));
#12878=CARTESIAN_POINT('Ctrl Pts',(3.75162486061771,2.31112467781931,4.53709416654516));
#12879=CARTESIAN_POINT('Ctrl Pts',(3.71021805048437,2.27470144834891,4.53338957019289));
#12880=CARTESIAN_POINT('Ctrl Pts',(3.66881124035102,2.23827821887852,4.52968497384062));
#12881=CARTESIAN_POINT('Ctrl Pts',(3.60756372063751,2.22441038905077,4.52598037748835));
#12882=CARTESIAN_POINT('Ctrl Pts',(3.55450576575121,2.23944465009304,4.52227578113609));
#12883=CARTESIAN_POINT('Ctrl Pts',(3.50144781086492,2.25447891113532,4.51857118478382));
#12884=CARTESIAN_POINT('Ctrl Pts',(3.45657942080584,2.29841526304761,4.51486658843155));
#12885=CARTESIAN_POINT('Ctrl Pts',(3.44043486927933,2.35114598469909,4.51116199207928));
#12886=CARTESIAN_POINT('Ctrl Pts',(3.43562652497117,2.36685081644385,4.51005864927318));
#12887=CARTESIAN_POINT('Ctrl Pts',(3.43336607622673,2.38333573667221,4.50895530646708));
#12888=CARTESIAN_POINT('Ctrl Pts',(3.43350143198867,2.39985687063426,4.50785196366098));
#12889=CARTESIAN_POINT('Ctrl Pts',(3.43366207255012,2.4000380247868,4.52714803633902));
#12890=CARTESIAN_POINT('Ctrl Pts',(3.43372360717887,2.36989468640869,4.52915624308993));
#12891=CARTESIAN_POINT('Ctrl Pts',(3.44154516635149,2.33972158979514,4.53116444984084));
#12892=CARTESIAN_POINT('Ctrl Pts',(3.45693460375181,2.31409281443648,4.53317265659175));
#12893=CARTESIAN_POINT('Ctrl Pts',(3.48532393848085,2.26681468051736,4.53687725294402));
#12894=CARTESIAN_POINT('Ctrl Pts',(3.53946694042407,2.23500097847622,4.54058184929629));
#12895=CARTESIAN_POINT('Ctrl Pts',(3.59458475774056,2.23321142940033,4.54428644564855));
#12896=CARTESIAN_POINT('Ctrl Pts',(3.64970257505705,2.23142188032444,4.54799104200082));
#12897=CARTESIAN_POINT('Ctrl Pts',(3.7057952077468,2.25965648421381,4.55169563835309));
#12898=CARTESIAN_POINT('Ctrl Pts',(3.73719154438744,2.30499351452124,4.55540023470536));
#12899=CARTESIAN_POINT('Ctrl Pts',(3.76858788102808,2.35033054482868,4.55910483105763));
#12900=CARTESIAN_POINT('Ctrl Pts',(3.77528792161962,2.41277000155418,4.56280942740989));
#12901=CARTESIAN_POINT('Ctrl Pts',(3.75422535459604,2.4637361132596,4.56651402376216));
#12902=CARTESIAN_POINT('Ctrl Pts',(3.73316278757246,2.51470222496502,4.57021862011443));
#12903=CARTESIAN_POINT('Ctrl Pts',(3.68433761293377,2.55419499165036,4.5739232164667));
#12904=CARTESIAN_POINT('Ctrl Pts',(3.63009494870967,2.56414032470881,4.57762781281897));
#12905=CARTESIAN_POINT('Ctrl Pts',(3.57585228448556,2.57408565776726,4.58133240917124));
#12906=CARTESIAN_POINT('Ctrl Pts',(3.51619213067606,2.55448355719882,4.5850370055235));
#12907=CARTESIAN_POINT('Ctrl Pts',(3.47841829496877,2.51430503547713,4.58874160187577));
#12908=CARTESIAN_POINT('Ctrl Pts',(3.44984628656769,2.48391413027303,4.59154374669685));
#12909=CARTESIAN_POINT('Ctrl Pts',(3.43379623122065,2.44175071136891,4.59434589151794));
#12910=CARTESIAN_POINT('Ctrl Pts',(3.43341474631901,2.39984765669014,4.59714803633902));
#12911=CARTESIAN_POINT('Origin',(3.6,2.4,4.7));
#12912=CARTESIAN_POINT('',(3.43314571939013,2.4000550352968,4.66714803633902));
#12913=CARTESIAN_POINT('',(3.43350338992805,2.40014270746267,4.64785196366098));
#12914=CARTESIAN_POINT('',(3.4334,2.4,4.7));
#12915=CARTESIAN_POINT('Ctrl Pts',(3.43350338992805,2.40014270746267,4.64785196366098));
#12916=CARTESIAN_POINT('Ctrl Pts',(3.43336795942281,2.41673658085083,4.64674379602763));
#12917=CARTESIAN_POINT('Ctrl Pts',(3.43564861639563,2.43329406542932,4.64563562839428));
#12918=CARTESIAN_POINT('Ctrl Pts',(3.44049847652216,2.44906128539828,4.64452746076093));
#12919=CARTESIAN_POINT('Ctrl Pts',(3.45671152371201,2.5017709872742,4.64082286440866));
#12920=CARTESIAN_POINT('Ctrl Pts',(3.5016369588364,2.54564900761994,4.63711826805639));
#12921=CARTESIAN_POINT('Ctrl Pts',(3.55471440176584,2.56061432161925,4.63341367170412));
#12922=CARTESIAN_POINT('Ctrl Pts',(3.60779184469527,2.57557963561855,4.62970907535186));
#12923=CARTESIAN_POINT('Ctrl Pts',(3.66902129542974,2.56163224327142,4.62600447899959));
#12924=CARTESIAN_POINT('Ctrl Pts',(3.71038074864658,2.52515524777208,4.62229988264732));
#12925=CARTESIAN_POINT('Ctrl Pts',(3.75174020186341,2.48867825227274,4.61859528629505));
#12926=CARTESIAN_POINT('Ctrl Pts',(3.77322965756262,2.42967165362121,4.61489068994278));
#12927=CARTESIAN_POINT('Ctrl Pts',(3.76501434448883,2.37514015628156,4.61118609359052));
#12928=CARTESIAN_POINT('Ctrl Pts',(3.75679903141505,2.32060865894192,4.60748149723825));
#12929=CARTESIAN_POINT('Ctrl Pts',(3.71887894956827,2.27055226291416,4.60377690088598));
#12930=CARTESIAN_POINT('Ctrl Pts',(3.6686084394294,2.24787956167738,4.60007230453371));
#12931=CARTESIAN_POINT('Ctrl Pts',(3.61833792929053,2.22520686044059,4.59636770818145));
#12932=CARTESIAN_POINT('Ctrl Pts',(3.55571699085956,2.22991785399477,4.59266311182918));
#12933=CARTESIAN_POINT('Ctrl Pts',(3.50940445168984,2.2598565294309,4.58895851547691));
#12934=CARTESIAN_POINT('Ctrl Pts',(3.46312207100161,2.28977570895933,4.58525633153827));
#12935=CARTESIAN_POINT('Ctrl Pts',(3.43312685660295,2.34488972480058,4.58155414759962));
#12936=CARTESIAN_POINT('Ctrl Pts',(3.43312356496403,2.40000067111703,4.57785196366098));
#12937=CARTESIAN_POINT('Ctrl Pts',(3.43341474631901,2.39984765669014,4.59714803633902));
#12938=CARTESIAN_POINT('Ctrl Pts',(3.43329188627587,2.38635246701557,4.59805048787021));
#12939=CARTESIAN_POINT('Ctrl Pts',(3.43479418574107,2.37288428257405,4.59895293940139));
#12940=CARTESIAN_POINT('Ctrl Pts',(3.43802675467359,2.35984505096448,4.59985539093258));
#12941=CARTESIAN_POINT('Ctrl Pts',(3.45129656769075,2.30631853104845,4.60355998728484));
#12942=CARTESIAN_POINT('Ctrl Pts',(3.49372371133013,2.26002043409134,4.60726458363711));
#12943=CARTESIAN_POINT('Ctrl Pts',(3.54589116272705,2.24213934669288,4.61096917998938));
#12944=CARTESIAN_POINT('Ctrl Pts',(3.59805861412397,2.22425825929442,4.61467377634164));
#12945=CARTESIAN_POINT('Ctrl Pts',(3.65996637327845,2.23479418145462,4.61837837269391));
#12946=CARTESIAN_POINT('Ctrl Pts',(3.70328200317247,2.26892528865449,4.62208296904618));
#12947=CARTESIAN_POINT('Ctrl Pts',(3.7465976330665,2.30305639585435,4.62578756539845));
#12948=CARTESIAN_POINT('Ctrl Pts',(3.77132113370008,2.3607826880939,4.62949216175072));
#12949=CARTESIAN_POINT('Ctrl Pts',(3.76613765481651,2.41568540039916,4.63319675810299));
#12950=CARTESIAN_POINT('Ctrl Pts',(3.76095417593294,2.47058811270442,4.63690135445526));
#12951=CARTESIAN_POINT('Ctrl Pts',(3.72586371753223,2.5226672450754,4.64060595080753));
#12952=CARTESIAN_POINT('Ctrl Pts',(3.67692562687786,2.54808848727385,4.64431054715979));
#12953=CARTESIAN_POINT('Ctrl Pts',(3.6279875362235,2.5735097294723,4.64801514351206));
#12954=CARTESIAN_POINT('Ctrl Pts',(3.56520181331549,2.57227308149821,4.65171973986433));
#12955=CARTESIAN_POINT('Ctrl Pts',(3.51730270026196,2.54494450230916,4.65542433621659));
#12956=CARTESIAN_POINT('Ctrl Pts',(3.46940358720842,2.51761592312011,4.65912893256886));
#12957=CARTESIAN_POINT('Ctrl Pts',(3.43639108400936,2.46419541271609,4.66283352892113));
#12958=CARTESIAN_POINT('Ctrl Pts',(3.43337354994745,2.40913117059842,4.6665381252734));
#12959=CARTESIAN_POINT('Ctrl Pts',(3.43320795139183,2.40610931275893,4.66674142896194));
#12960=CARTESIAN_POINT('Ctrl Pts',(3.43313268806444,2.40308250452664,4.66694473265048));
#12961=CARTESIAN_POINT('Ctrl Pts',(3.43314571939013,2.4000550352968,4.66714803633902));
#12962=CARTESIAN_POINT('Origin',(3.6,2.4,4.7));
#12963=CARTESIAN_POINT('',(3.43357722762007,2.40011764662452,4.73714803633902));
#12964=CARTESIAN_POINT('',(3.43362781118013,2.39991574862771,4.71785196366098));
#12965=CARTESIAN_POINT('',(3.4334,2.4,4.7));
#12966=CARTESIAN_POINT('Ctrl Pts',(3.43362781118013,2.39991574862771,4.71785196366098));
#12967=CARTESIAN_POINT('Ctrl Pts',(3.4337799165104,2.43312978761853,4.71563804080791));
#12968=CARTESIAN_POINT('Ctrl Pts',(3.44340626416077,2.46642503117871,4.71342411795483));
#12969=CARTESIAN_POINT('Ctrl Pts',(3.46191047388993,2.49369647002616,4.71121019510175));
#12970=CARTESIAN_POINT('Ctrl Pts',(3.49287389602047,2.5393302520412,4.70750559874949));
#12971=CARTESIAN_POINT('Ctrl Pts',(3.54869526280824,2.56809742778931,4.70380100239722));
#12972=CARTESIAN_POINT('Ctrl Pts',(3.60382760921412,2.56683253616837,4.70009640604495));
#12973=CARTESIAN_POINT('Ctrl Pts',(3.65895995562,2.56556764454744,4.69639180969268));
#12974=CARTESIAN_POINT('Ctrl Pts',(3.71340328164399,2.53427068555747,4.69268721334041));
#12975=CARTESIAN_POINT('Ctrl Pts',(3.74224129041658,2.48726488994604,4.68898261698815));
#12976=CARTESIAN_POINT('Ctrl Pts',(3.77107929918916,2.44025909433461,4.68527802063588));
#12977=CARTESIAN_POINT('Ctrl Pts',(3.77431199071034,2.37754446210172,4.68157342428361));
#12978=CARTESIAN_POINT('Ctrl Pts',(3.75045990537481,2.32782270030492,4.67786882793134));
#12979=CARTESIAN_POINT('Ctrl Pts',(3.72660782003928,2.27810093850813,4.67416423157907));
#12980=CARTESIAN_POINT('Ctrl Pts',(3.67567095784705,2.24137204714742,4.6704596352268));
#12981=CARTESIAN_POINT('Ctrl Pts',(3.62096086261208,2.23444521162098,4.66675503887454));
#12982=CARTESIAN_POINT('Ctrl Pts',(3.56625076737711,2.22751837609454,4.66305044252227));
#12983=CARTESIAN_POINT('Ctrl Pts',(3.5077674390994,2.25039359640236,4.65934584617));
#12984=CARTESIAN_POINT('Ctrl Pts',(3.4722761045882,2.29260189825932,4.65564124981774));
#12985=CARTESIAN_POINT('Ctrl Pts',(3.44740140531328,2.32218429717603,4.65304482109882));
#12986=CARTESIAN_POINT('Ctrl Pts',(3.43382070261849,2.36126338259659,4.6504483923799));
#12987=CARTESIAN_POINT('Ctrl Pts',(3.43350338992805,2.40014270746267,4.64785196366098));
#12988=CARTESIAN_POINT('Ctrl Pts',(3.43314571939013,2.4000550352968,4.66714803633902));
#12989=CARTESIAN_POINT('Ctrl Pts',(3.43337014465933,2.34791601174949,4.67064932900275));
#12990=CARTESIAN_POINT('Ctrl Pts',(3.45978247246013,2.29558093851357,4.67415062166648));
#12991=CARTESIAN_POINT('Ctrl Pts',(3.50195947903851,2.26495997488444,4.67765191433021));
#12992=CARTESIAN_POINT('Ctrl Pts',(3.54658550711625,2.23256099511944,4.68135651068247));
#12993=CARTESIAN_POINT('Ctrl Pts',(3.60886012819649,2.22447100942077,4.68506110703474));
#12994=CARTESIAN_POINT('Ctrl Pts',(3.66028300882075,2.24439244561677,4.68876570338701));
#12995=CARTESIAN_POINT('Ctrl Pts',(3.71170588944501,2.26431388181277,4.69247029973928));
#12996=CARTESIAN_POINT('Ctrl Pts',(3.75227702961328,2.31224673990343,4.69617489609154));
#12997=CARTESIAN_POINT('Ctrl Pts',(3.76342881697354,2.36625427558577,4.69987949244381));
#12998=CARTESIAN_POINT('Ctrl Pts',(3.7745806043338,2.42026181126811,4.70358408879608));
#12999=CARTESIAN_POINT('Ctrl Pts',(3.75631303888606,2.48034402454213,4.70728868514835));
#13000=CARTESIAN_POINT('Ctrl Pts',(3.71698637554161,2.51900394981365,4.71099328150062));
#13001=CARTESIAN_POINT('Ctrl Pts',(3.67765971219715,2.55766387508518,4.71469787785288));
#13002=CARTESIAN_POINT('Ctrl Pts',(3.617273950956,2.57490151235421,4.71840247420515));
#13003=CARTESIAN_POINT('Ctrl Pts',(3.5634649778607,2.56282795918052,4.72210707055742));
#13004=CARTESIAN_POINT('Ctrl Pts',(3.50965600476541,2.55075440600683,4.72581166690969));
#13005=CARTESIAN_POINT('Ctrl Pts',(3.46242381981598,2.50936966239043,4.72951626326196));
#13006=CARTESIAN_POINT('Ctrl Pts',(3.44338450027923,2.45761369091481,4.73322085961423));
#13007=CARTESIAN_POINT('Ctrl Pts',(3.43665675223952,2.43932516253718,4.73452991852249));
#13008=CARTESIAN_POINT('Ctrl Pts',(3.43344927286167,2.41974164310833,4.73583897743076));
#13009=CARTESIAN_POINT('Ctrl Pts',(3.43357722762007,2.40011764662452,4.73714803633902));
#13010=CARTESIAN_POINT('Origin',(3.6,2.4,4.7));
#13011=CARTESIAN_POINT('',(3.4335708769619,2.39987935507417,4.80714803633902));
#13012=CARTESIAN_POINT('',(3.43319592025803,2.39990252619761,4.78785196366098));
#13013=CARTESIAN_POINT('',(3.4334,2.4,4.7));
#13014=CARTESIAN_POINT('Ctrl Pts',(3.43319592025803,2.39990252619761,4.78785196366098));
#13015=CARTESIAN_POINT('Ctrl Pts',(3.43353981667182,2.44937640878962,4.78453228558818));
#13016=CARTESIAN_POINT('Ctrl Pts',(3.45695303934336,2.49913297337583,4.78121260751538));
#13017=CARTESIAN_POINT('Ctrl Pts',(3.495475201044,2.5300857875399,4.77789292944258));
#13018=CARTESIAN_POINT('Ctrl Pts',(3.5384640260409,2.56462759548935,4.77418833309031));
#13019=CARTESIAN_POINT('Ctrl Pts',(3.60026870000874,2.57575223778946,4.77048373673805));
#13020=CARTESIAN_POINT('Ctrl Pts',(3.6526039634498,2.55836845881058,4.76677914038578));
#13021=CARTESIAN_POINT('Ctrl Pts',(3.70493922689085,2.54098467983171,4.76307454403351));
#13022=CARTESIAN_POINT('Ctrl Pts',(3.74780507980512,2.49509247957384,4.75936994768124));
#13023=CARTESIAN_POINT('Ctrl Pts',(3.76158372154047,2.44169468371147,4.75566535132897));
#13024=CARTESIAN_POINT('Ctrl Pts',(3.77536236327582,2.38829688784909,4.7519607549767));
#13025=CARTESIAN_POINT('Ctrl Pts',(3.76005379383226,2.32739349638222,4.74825615862444));
#13026=CARTESIAN_POINT('Ctrl Pts',(3.72266406682112,2.28685729176137,4.74455156227217));
#13027=CARTESIAN_POINT('Ctrl Pts',(3.68527433980998,2.24632108714052,4.7408469659199));
#13028=CARTESIAN_POINT('Ctrl Pts',(3.62580345523126,2.22615206936571,4.73714236956763));
#13029=CARTESIAN_POINT('Ctrl Pts',(3.57146860063526,2.23558070378767,4.73343777321536));
#13030=CARTESIAN_POINT('Ctrl Pts',(3.51713374603927,2.24500933820964,4.72973317686309));
#13031=CARTESIAN_POINT('Ctrl Pts',(3.467934921426,2.28403562482839,4.72602858051083));
#13032=CARTESIAN_POINT('Ctrl Pts',(3.44638824785603,2.33479896227876,4.72232398415856));
#13033=CARTESIAN_POINT('Ctrl Pts',(3.43771819254303,2.35522536091232,4.72083331065937));
#13034=CARTESIAN_POINT('Ctrl Pts',(3.43352539596517,2.37755214744982,4.71934263716017));
#13035=CARTESIAN_POINT('Ctrl Pts',(3.43362781118013,2.39991574862771,4.71785196366098));
#13036=CARTESIAN_POINT('Ctrl Pts',(3.43357722762007,2.40011764662452,4.73714803633902));
#13037=CARTESIAN_POINT('Ctrl Pts',(3.4338113808831,2.36420633806453,4.73954357378302));
#13038=CARTESIAN_POINT('Ctrl Pts',(3.44521519316665,2.32815948046248,4.74193911122703));
#13039=CARTESIAN_POINT('Ctrl Pts',(3.46665596573275,2.29966495797107,4.74433464867103));
#13040=CARTESIAN_POINT('Ctrl Pts',(3.49981320484709,2.25559939583779,4.7480392450233));
#13041=CARTESIAN_POINT('Ctrl Pts',(3.55697413719987,2.22959547090607,4.75174384137556));
#13042=CARTESIAN_POINT('Ctrl Pts',(3.61197873797528,2.23355402687319,4.75544843772783));
#13043=CARTESIAN_POINT('Ctrl Pts',(3.6669833387507,2.2375125828403,4.7591530340801));
#13044=CARTESIAN_POINT('Ctrl Pts',(3.71983160794876,2.27143361970626,4.76285763043237));
#13045=CARTESIAN_POINT('Ctrl Pts',(3.74633723550091,2.31979298260399,4.76656222678464));
#13046=CARTESIAN_POINT('Ctrl Pts',(3.77284286305306,2.36815234550172,4.7702668231369));
#13047=CARTESIAN_POINT('Ctrl Pts',(3.77300584895929,2.43095003443123,4.77397141948917));
#13048=CARTESIAN_POINT('Ctrl Pts',(3.74675160179543,2.47944633096681,4.77767601584144));
#13049=CARTESIAN_POINT('Ctrl Pts',(3.72049735463157,2.52794262750239,4.78138061219371));
#13050=CARTESIAN_POINT('Ctrl Pts',(3.66782587439761,2.56213753164403,4.78508520854598));
#13051=CARTESIAN_POINT('Ctrl Pts',(3.61284256269023,2.56638155161303,4.78878980489825));
#13052=CARTESIAN_POINT('Ctrl Pts',(3.55785925098286,2.57062557158203,4.79249440125052));
#13053=CARTESIAN_POINT('Ctrl Pts',(3.50056410780207,2.54491870737838,4.79619899760278));
#13054=CARTESIAN_POINT('Ctrl Pts',(3.4671785803101,2.50102585117272,4.79990359395505));
#13055=CARTESIAN_POINT('Ctrl Pts',(3.44541646757448,2.47241461280706,4.80231840808304));
#13056=CARTESIAN_POINT('Ctrl Pts',(3.43381352470784,2.43607616609189,4.80473322221103));
#13057=CARTESIAN_POINT('Ctrl Pts',(3.4335708769619,2.39987935507417,4.80714803633902));
#13058=CARTESIAN_POINT('Origin',(3.6,2.4,4.7));
#13059=CARTESIAN_POINT('',(3.43314188794433,2.3999499425809,4.87714803633902));
#13060=CARTESIAN_POINT('',(3.43333250203974,2.40014587505553,4.85785196366098));
#13061=CARTESIAN_POINT('',(3.4334,2.4,4.7));
#13062=CARTESIAN_POINT('Ctrl Pts',(3.43333250203974,2.40014587505553,4.85785196366098));
#13063=CARTESIAN_POINT('Ctrl Pts',(3.43323383740233,2.41091157669441,4.85713112672073));
#13064=CARTESIAN_POINT('Ctrl Pts',(3.43418764294185,2.42165986991066,4.85641028978047));
#13065=CARTESIAN_POINT('Ctrl Pts',(3.43625743346387,2.43218878097762,4.85568945284021));
#13066=CARTESIAN_POINT('Ctrl Pts',(3.44689470520955,2.48629999996998,4.85198485648794));
#13067=CARTESIAN_POINT('Ctrl Pts',(3.48700780884227,2.53461681182183,4.84828026013567));
#13068=CARTESIAN_POINT('Ctrl Pts',(3.53823875502779,2.55502675361418,4.8445756637834));
#13069=CARTESIAN_POINT('Ctrl Pts',(3.58946970121331,2.57543669540653,4.84087106743113));
#13070=CARTESIAN_POINT('Ctrl Pts',(3.65181848995162,2.56793976713939,4.83716647107887));
#13071=CARTESIAN_POINT('Ctrl Pts',(3.69675084453495,2.5359669805447,4.8334618747266));
#13072=CARTESIAN_POINT('Ctrl Pts',(3.74168319911827,2.50399419395,4.82975727837433));
#13073=CARTESIAN_POINT('Ctrl Pts',(3.7691991195466,2.44754554902777,4.82605268202206));
#13074=CARTESIAN_POINT('Ctrl Pts',(3.76670578881005,2.39245508821223,4.8223480856698));
#13075=CARTESIAN_POINT('Ctrl Pts',(3.7642124580735,2.33736462739668,4.81864348931753));
#13076=CARTESIAN_POINT('Ctrl Pts',(3.73170987617206,2.28363235068783,4.81493889296526));
#13077=CARTESIAN_POINT('Ctrl Pts',(3.68407303401509,2.25584913920422,4.811234296613));
#13078=CARTESIAN_POINT('Ctrl Pts',(3.63643619185813,2.2280659277206,4.80752970026073));
#13079=CARTESIAN_POINT('Ctrl Pts',(3.57366508944564,2.22623178146222,4.80382510390846));
#13080=CARTESIAN_POINT('Ctrl Pts',(3.52448727773306,2.25118610786454,4.80012050755619));
#13081=CARTESIAN_POINT('Ctrl Pts',(3.47530946602049,2.27614043426686,4.79641591120392));
#13082=CARTESIAN_POINT('Ctrl Pts',(3.43972494500783,2.32788323332987,4.79271131485165));
#13083=CARTESIAN_POINT('Ctrl Pts',(3.43401917251448,2.38273411966077,4.78900671849938));
#13084=CARTESIAN_POINT('Ctrl Pts',(3.43342632624397,2.38843328545001,4.78862180021992));
#13085=CARTESIAN_POINT('Ctrl Pts',(3.43315604530238,2.39416600556269,4.78823688194045));
#13086=CARTESIAN_POINT('Ctrl Pts',(3.43319592025803,2.39990252619761,4.78785196366098));
#13087=CARTESIAN_POINT('Ctrl Pts',(3.4335708769619,2.39987935507417,4.80714803633902));
#13088=CARTESIAN_POINT('Ctrl Pts',(3.43344127578645,2.38054618864739,4.8084378185633));
#13089=CARTESIAN_POINT('Ctrl Pts',(3.43655249507166,2.36125342749717,4.80972760078758));
#13090=CARTESIAN_POINT('Ctrl Pts',(3.44308754966948,2.34320004344294,4.81101738301185));
#13091=CARTESIAN_POINT('Ctrl Pts',(3.46185795832395,2.2913459401265,4.81472197936412));
#13092=CARTESIAN_POINT('Ctrl Pts',(3.50887468743604,2.24971658170129,4.81842657571639));
#13093=CARTESIAN_POINT('Ctrl Pts',(3.5626202643246,2.23736388010515,4.82213117206866));
#13094=CARTESIAN_POINT('Ctrl Pts',(3.61636584121316,2.22501117850901,4.82583576842092));
#13095=CARTESIAN_POINT('Ctrl Pts',(3.6768402658782,2.24193513374194,4.82954036477319));
#13096=CARTESIAN_POINT('Ctrl Pts',(3.71636707495845,2.28039040172619,4.83324496112546));
#13097=CARTESIAN_POINT('Ctrl Pts',(3.7558938840387,2.31884566971043,4.83694955747773));
#13098=CARTESIAN_POINT('Ctrl Pts',(3.77447307753417,2.378832250446,4.84065415383));
#13099=CARTESIAN_POINT('Ctrl Pts',(3.76360178219044,2.4328969451123,4.84435875018227));
#13100=CARTESIAN_POINT('Ctrl Pts',(3.75273048684672,2.4869616397786,4.84806334653454));
#13101=CARTESIAN_POINT('Ctrl Pts',(3.71240870266382,2.53510444837563,4.8517679428868));
#13102=CARTESIAN_POINT('Ctrl Pts',(3.66108992281312,2.55529254156049,4.85547253923907));
#13103=CARTESIAN_POINT('Ctrl Pts',(3.60977114296242,2.57548063474534,4.85917713559134));
#13104=CARTESIAN_POINT('Ctrl Pts',(3.54745536744392,2.56771401251802,4.86288173194361));
#13105=CARTESIAN_POINT('Ctrl Pts',(3.50266176427811,2.53554711358097,4.86658632829587));
#13106=CARTESIAN_POINT('Ctrl Pts',(3.46009329762648,2.50497811560107,4.87010689764359));
#13107=CARTESIAN_POINT('Ctrl Pts',(3.43334940270065,2.45237281292388,4.87362746699131));
#13108=CARTESIAN_POINT('Ctrl Pts',(3.43314188794433,2.3999499425809,4.87714803633902));
#13109=CARTESIAN_POINT('Origin',(3.6,2.4,4.7));
#13110=CARTESIAN_POINT('',(3.43342338863395,2.40015219044389,4.94714803633902));
#13111=CARTESIAN_POINT('',(3.4336698690944,2.40000633253548,4.92785196366098));
#13112=CARTESIAN_POINT('',(3.4334,2.4,4.7));
#13113=CARTESIAN_POINT('Ctrl Pts',(3.4336698690944,2.40000633253548,4.92785196366098));
#13114=CARTESIAN_POINT('Ctrl Pts',(3.43366057242126,2.42742681740845,4.926025371501));
#13115=CARTESIAN_POINT('Ctrl Pts',(3.44006468394764,2.45484321422969,4.92419877934102));
#13116=CARTESIAN_POINT('Ctrl Pts',(3.4529060499396,2.47881063108511,4.92237218718104));
#13117=CARTESIAN_POINT('Ctrl Pts',(3.47895022041959,2.52742006180595,4.91866759082877));
#13118=CARTESIAN_POINT('Ctrl Pts',(3.53147325119262,2.5618425345377,4.9149629944765));
#13119=CARTESIAN_POINT('Ctrl Pts',(3.58643767940152,2.56632440944362,4.91125839812423));
#13120=CARTESIAN_POINT('Ctrl Pts',(3.64140210761043,2.57080628434953,4.90755380177196));
#13121=CARTESIAN_POINT('Ctrl Pts',(3.6988079332552,2.54534756142961,4.90384920541969));
#13122=CARTESIAN_POINT('Ctrl Pts',(3.73238305471537,2.50159956959011,4.90014460906743));
#13123=CARTESIAN_POINT('Ctrl Pts',(3.76595817617555,2.45785157775061,4.89644001271516));
#13124=CARTESIAN_POINT('Ctrl Pts',(3.77570259345112,2.39581431699153,4.89273541636289));
#13125=CARTESIAN_POINT('Ctrl Pts',(3.75715671872181,2.34387949147388,4.88903082001062));
#13126=CARTESIAN_POINT('Ctrl Pts',(3.7386108439925,2.29194466595622,4.88532622365836));
#13127=CARTESIAN_POINT('Ctrl Pts',(3.6917746772583,2.25011227567998,4.88162162730609));
#13128=CARTESIAN_POINT('Ctrl Pts',(3.638083055804,2.23752715126117,4.87791703095382));
#13129=CARTESIAN_POINT('Ctrl Pts',(3.58439143434971,2.22494202684235,4.87421243460155));
#13130=CARTESIAN_POINT('Ctrl Pts',(3.52384435817533,2.24160416828095,4.87050783824928));
#13131=CARTESIAN_POINT('Ctrl Pts',(3.48415154001745,2.27988805206668,4.86680324189701));
#13132=CARTESIAN_POINT('Ctrl Pts',(3.45218211379499,2.3107226930672,4.863819482485));
#13133=CARTESIAN_POINT('Ctrl Pts',(3.43374090444541,2.35558342022287,4.86083572307299));
#13134=CARTESIAN_POINT('Ctrl Pts',(3.43333250203974,2.40014587505553,4.85785196366098));
#13135=CARTESIAN_POINT('Ctrl Pts',(3.43314188794433,2.3999499425809,4.87714803633902));
#13136=CARTESIAN_POINT('Ctrl Pts',(3.43313104074456,2.39720969722669,4.87733206334358));
#13137=CARTESIAN_POINT('Ctrl Pts',(3.43319270038641,2.39446995034259,4.87751609034813));
#13138=CARTESIAN_POINT('Ctrl Pts',(3.43332839678999,2.39173387533235,4.87770011735268));
#13139=CARTESIAN_POINT('Ctrl Pts',(3.43606006328079,2.33665471166754,4.88140471370495));
#13140=CARTESIAN_POINT('Ctrl Pts',(3.4687948270755,2.28306355998471,4.88510931005722));
#13141=CARTESIAN_POINT('Ctrl Pts',(3.5165514379046,2.2554867147355,4.88881390640948));
#13142=CARTESIAN_POINT('Ctrl Pts',(3.5643080487337,2.2279098694863,4.89251850276175));
#13143=CARTESIAN_POINT('Ctrl Pts',(3.6270865065972,2.22634733067072,4.89622309911402));
#13144=CARTESIAN_POINT('Ctrl Pts',(3.67615589427605,2.25151420303488,4.89992769546629));
#13145=CARTESIAN_POINT('Ctrl Pts',(3.72522528195491,2.27668107539905,4.90363229181856));
#13146=CARTESIAN_POINT('Ctrl Pts',(3.76058559944912,2.32857735894297,4.90733688817082));
#13147=CARTESIAN_POINT('Ctrl Pts',(3.76605399695032,2.38345242523688,4.91104148452309));
#13148=CARTESIAN_POINT('Ctrl Pts',(3.77152239445151,2.43832749153079,4.91474608087536));
#13149=CARTESIAN_POINT('Ctrl Pts',(3.74709887195967,2.4961813405747,4.91845067722763));
#13150=CARTESIAN_POINT('Ctrl Pts',(3.70396099303503,2.53053683028788,4.9221552735799));
#13151=CARTESIAN_POINT('Ctrl Pts',(3.66082311411038,2.56489232000106,4.92585986993216));
#13152=CARTESIAN_POINT('Ctrl Pts',(3.59897087875293,2.57574945038351,4.92956446628443));
#13153=CARTESIAN_POINT('Ctrl Pts',(3.54671131319796,2.55813939417591,4.9332690626367));
#13154=CARTESIAN_POINT('Ctrl Pts',(3.494451747643,2.5405293379683,4.93697365898897));
#13155=CARTESIAN_POINT('Ctrl Pts',(3.45178485189053,2.49445209517064,4.94067825534124));
#13156=CARTESIAN_POINT('Ctrl Pts',(3.43823737272355,2.44099517717631,4.94438285169351));
#13157=CARTESIAN_POINT('Ctrl Pts',(3.43486666978988,2.42769474038747,4.94530457990868));
#13158=CARTESIAN_POINT('Ctrl Pts',(3.43329859706143,2.41393746665015,4.94622630812385));
#13159=CARTESIAN_POINT('Ctrl Pts',(3.43342338863395,2.40015219044389,4.94714803633902));
#13160=CARTESIAN_POINT('Origin',(3.6,2.4,4.7));
#13161=CARTESIAN_POINT('',(3.43365998372879,2.39995738785189,5.01714803633902));
#13162=CARTESIAN_POINT('',(3.43335574706359,2.39985083704977,4.99785196366098));
#13163=CARTESIAN_POINT('',(3.4334,2.4,4.7));
#13164=CARTESIAN_POINT('Ctrl Pts',(3.43335574706359,2.39985083704977,4.99785196366098));
#13165=CARTESIAN_POINT('Ctrl Pts',(3.43376006251615,2.44366117078388,4.99491961628127));
#13166=CARTESIAN_POINT('Ctrl Pts',(3.45150379085869,2.48776127159334,4.99198726890157));
#13167=CARTESIAN_POINT('Ctrl Pts',(3.48249984106631,2.5184966596533,4.98905492152186));
#13168=CARTESIAN_POINT('Ctrl Pts',(3.52165886271855,2.55732637242214,4.98535032516959));
#13169=CARTESIAN_POINT('Ctrl Pts',(3.58196946998821,2.57482511625956,4.98164572881732));
#13170=CARTESIAN_POINT('Ctrl Pts',(3.63583017159909,2.56298449167174,4.97794113246505));
#13171=CARTESIAN_POINT('Ctrl Pts',(3.68969087320997,2.55114386708391,4.97423653611278));
#13172=CARTESIAN_POINT('Ctrl Pts',(3.73710166916209,2.50996387407084,4.97053193976052));
#13173=CARTESIAN_POINT('Ctrl Pts',(3.75636473978792,2.45829077001732,4.96682734340825));
#13174=CARTESIAN_POINT('Ctrl Pts',(3.77562781041376,2.4066176659638,4.96312274705598));
#13175=CARTESIAN_POINT('Ctrl Pts',(3.76674315571332,2.34445145086982,4.95941815070371));
#13176=CARTESIAN_POINT('Ctrl Pts',(3.73377688832091,2.30024284554165,4.95571355435145));
#13177=CARTESIAN_POINT('Ctrl Pts',(3.70081062092849,2.25603424021347,4.95200895799918));
#13178=CARTESIAN_POINT('Ctrl Pts',(3.64376274084411,2.2297832446511,4.94830436164691));
#13179=CARTESIAN_POINT('Ctrl Pts',(3.58874153385625,2.23350377584586,4.94459976529464));
#13180=CARTESIAN_POINT('Ctrl Pts',(3.5337203268684,2.23722430704061,4.94089516894238));
#13181=CARTESIAN_POINT('Ctrl Pts',(3.48072579297707,2.2709163649925,4.93719057259011));
#13182=CARTESIAN_POINT('Ctrl Pts',(3.45401118112487,2.31916058832341,4.93348597623784));
#13183=CARTESIAN_POINT('Ctrl Pts',(3.44046850379027,2.34361746433734,4.93160797204555));
#13184=CARTESIAN_POINT('Ctrl Pts',(3.43367942743562,2.37181405914562,4.92972996785326));
#13185=CARTESIAN_POINT('Ctrl Pts',(3.4336698690944,2.40000633253548,4.92785196366098));
#13186=CARTESIAN_POINT('Ctrl Pts',(3.43342338863395,2.40015219044389,4.94714803633902));
#13187=CARTESIAN_POINT('Ctrl Pts',(3.43380015749623,2.35853188927053,4.94993090447612));
#13188=CARTESIAN_POINT('Ctrl Pts',(3.44960819526551,2.31665633218087,4.95271377261321));
#13189=CARTESIAN_POINT('Ctrl Pts',(3.47782659951237,2.28632760954166,4.95549664075031));
#13190=CARTESIAN_POINT('Ctrl Pts',(3.51539136804964,2.24595355309232,4.95920123710258));
#13191=CARTESIAN_POINT('Ctrl Pts',(3.57494896770565,2.22604203338462,4.96290583345485));
#13192=CARTESIAN_POINT('Ctrl Pts',(3.62924252529985,2.23570567012353,4.96661042980711));
#13193=CARTESIAN_POINT('Ctrl Pts',(3.68353608289404,2.24536930686244,4.97031502615938));
#13194=CARTESIAN_POINT('Ctrl Pts',(3.73256559842641,2.28460810004796,4.97401962251165));
#13195=CARTESIAN_POINT('Ctrl Pts',(3.75389243606413,2.33546419387067,4.97772421886392));
#13196=CARTESIAN_POINT('Ctrl Pts',(3.77521927370186,2.38632028769338,4.98142881521618));
#13197=CARTESIAN_POINT('Ctrl Pts',(3.76884343344493,2.44879368215328,4.98513341156845));
#13198=CARTESIAN_POINT('Ctrl Pts',(3.73768285480685,2.49429307324449,4.98883800792072));
#13199=CARTESIAN_POINT('Ctrl Pts',(3.70652227616876,2.5397924643357,4.99254260427299));
#13200=CARTESIAN_POINT('Ctrl Pts',(3.65057695914952,2.5683178520582,4.99624720062526));
#13201=CARTESIAN_POINT('Ctrl Pts',(3.59545059518146,2.56681443253905,4.99995179697753));
#13202=CARTESIAN_POINT('Ctrl Pts',(3.54032423121339,2.5653110130199,5.00365639332979));
#13203=CARTESIAN_POINT('Ctrl Pts',(3.4860168202965,2.5337787862591,5.00736098968206));
#13204=CARTESIAN_POINT('Ctrl Pts',(3.45738245724731,2.48664865149311,5.01106558603433));
#13205=CARTESIAN_POINT('Ctrl Pts',(3.44171119613527,2.4608548649544,5.01309306946923));
#13206=CARTESIAN_POINT('Ctrl Pts',(3.43372965048622,2.43038911757193,5.01512055290412));
#13207=CARTESIAN_POINT('Ctrl Pts',(3.43365998372879,2.39995738785189,5.01714803633902));
#13208=CARTESIAN_POINT('Origin',(3.6,2.4,4.7));
#13209=CARTESIAN_POINT('',(3.43326717741735,2.39986996798437,5.08714803633902));
#13210=CARTESIAN_POINT('',(3.43317938608394,2.40008640134203,5.06785196366098));
#13211=CARTESIAN_POINT('',(3.4334,2.4,4.7));
#13212=CARTESIAN_POINT('Ctrl Pts',(3.43317938608394,2.40008640134203,5.06785196366098));
#13213=CARTESIAN_POINT('Ctrl Pts',(3.43314802172115,2.40505542046622,5.06751845741382));
#13214=CARTESIAN_POINT('Ctrl Pts',(3.4333507965104,2.41002184414099,5.06718495116665));
#13215=CARTESIAN_POINT('Ctrl Pts',(3.43379604919982,2.41496643290483,5.06685144491949));
#13216=CARTESIAN_POINT('Ctrl Pts',(3.4387419280344,2.46989105771691,5.06314684856722));
#13217=CARTESIAN_POINT('Ctrl Pts',(3.47360673324676,2.52212151084356,5.05944225221496));
#13218=CARTESIAN_POINT('Ctrl Pts',(3.52243437289015,2.54775424884904,5.05573765586269));
#13219=CARTESIAN_POINT('Ctrl Pts',(3.57126201253354,2.57338698685451,5.05203305951042));
#13220=CARTESIAN_POINT('Ctrl Pts',(3.63405248660798,2.57242200973882,5.04832846315815));
#13221=CARTESIAN_POINT('Ctrl Pts',(3.68206938667054,2.54530093495911,5.04462386680588));
#13222=CARTESIAN_POINT('Ctrl Pts',(3.7300862867331,2.51817986017941,5.04091927045361));
#13223=CARTESIAN_POINT('Ctrl Pts',(3.7633296127838,2.4649026877357,5.03721467410135));
#13224=CARTESIAN_POINT('Ctrl Pts',(3.76658536412569,2.40985202258946,5.03351007774908));
#13225=CARTESIAN_POINT('Ctrl Pts',(3.76984111546757,2.35480135744323,5.02980548139681));
#13226=CARTESIAN_POINT('Ctrl Pts',(3.74310929210064,2.29797719959448,5.02610088504454));
#13227=CARTESIAN_POINT('Ctrl Pts',(3.69862386658003,2.26538544465498,5.02239628869227));
#13228=CARTESIAN_POINT('Ctrl Pts',(3.65413844105941,2.23279368971548,5.01869169234));
#13229=CARTESIAN_POINT('Ctrl Pts',(3.59189941338511,2.22443433768522,5.01498709598774));
#13230=CARTESIAN_POINT('Ctrl Pts',(3.54039082648689,2.24413309464159,5.01128249963547));
#13231=CARTESIAN_POINT('Ctrl Pts',(3.48888223958867,2.26383185159795,5.0075779032832));
#13232=CARTESIAN_POINT('Ctrl Pts',(3.44810409346653,2.31158871754094,5.00387330693093));
#13233=CARTESIAN_POINT('Ctrl Pts',(3.43671873842288,2.36554749136257,5.00016871057866));
#13234=CARTESIAN_POINT('Ctrl Pts',(3.43434538167935,2.37679557446855,4.9993964616061));
#13235=CARTESIAN_POINT('Ctrl Pts',(3.43324926848095,2.38831315722103,4.99862421263354));
#13236=CARTESIAN_POINT('Ctrl Pts',(3.43335574706359,2.39985083704977,4.99785196366098));
#13237=CARTESIAN_POINT('Ctrl Pts',(3.43365998372879,2.39995738785189,5.01714803633902));
#13238=CARTESIAN_POINT('Ctrl Pts',(3.43360235612169,2.37478458193251,5.01882514925639));
#13239=CARTESIAN_POINT('Ctrl Pts',(3.43895837147105,2.34963505233992,5.02050226217376));
#13240=CARTESIAN_POINT('Ctrl Pts',(3.44985377385385,2.32717237393524,5.02217937509113));
#13241=CARTESIAN_POINT('Ctrl Pts',(3.47392076869108,2.2775542739145,5.0258839714434));
#13242=CARTESIAN_POINT('Ctrl Pts',(3.52501607354704,2.24104611664418,5.02958856779567));
#13243=CARTESIAN_POINT('Ctrl Pts',(3.57975563349286,2.23435605471958,5.03329316414794));
#13244=CARTESIAN_POINT('Ctrl Pts',(3.63449519343869,2.22766599279499,5.03699776050021));
#13245=CARTESIAN_POINT('Ctrl Pts',(3.69287900847437,2.25079402621613,5.04070235685247));
#13246=CARTESIAN_POINT('Ctrl Pts',(3.72818739245021,2.2931555045654,5.04440695320474));
#13247=CARTESIAN_POINT('Ctrl Pts',(3.76349577642604,2.33551698291468,5.04811154955701));
#13248=CARTESIAN_POINT('Ctrl Pts',(3.77572872934203,2.39711190619209,5.05181614590928));
#13249=CARTESIAN_POINT('Ctrl Pts',(3.75928777521595,2.44975095798197,5.05552074226155));
#13250=CARTESIAN_POINT('Ctrl Pts',(3.74284682108988,2.50239000977184,5.05922533861381));
#13251=CARTESIAN_POINT('Ctrl Pts',(3.69773195992176,2.54607319007419,5.06292993496608));
#13252=CARTESIAN_POINT('Ctrl Pts',(3.64459025516192,2.56080874487665,5.06663453131835));
#13253=CARTESIAN_POINT('Ctrl Pts',(3.59144855040209,2.57554429967911,5.07033912767062));
#13254=CARTESIAN_POINT('Ctrl Pts',(3.53028000205055,2.5613322289817,5.07404372402289));
#13255=CARTESIAN_POINT('Ctrl Pts',(3.48907876029587,2.52467656495583,5.07774832037516));
#13256=CARTESIAN_POINT('Ctrl Pts',(3.45423196161424,2.49367428224656,5.08088155902978));
#13257=CARTESIAN_POINT('Ctrl Pts',(3.43366833435756,2.44661747113372,5.0840147976844));
#13258=CARTESIAN_POINT('Ctrl Pts',(3.43326717741735,2.39986996798437,5.08714803633902));
#13259=CARTESIAN_POINT('Origin',(3.6,2.4,4.7));
#13260=CARTESIAN_POINT('',(3.43325215340634,2.40012157034435,5.15714803633902));
#13261=CARTESIAN_POINT('',(3.43361558566414,2.40009421455432,5.13785196366098));
#13262=CARTESIAN_POINT('',(3.4334,2.4,4.7));
#13263=CARTESIAN_POINT('',(3.72690708798524,2.50793586530485,5.2));
#13264=CARTESIAN_POINT('Ctrl Pts',(3.43325215340634,2.40012157034435,5.15714803633902));
#13265=CARTESIAN_POINT('Ctrl Pts',(3.43364568326786,2.35284438105766,5.16031823516921));
#13266=CARTESIAN_POINT('Ctrl Pts',(3.45475449837728,2.3052683699281,5.1634884339994));
#13267=CARTESIAN_POINT('Ctrl Pts',(3.49032381108024,2.27424021130156,5.16665863282959));
#13268=CARTESIAN_POINT('Ctrl Pts',(3.53188901034701,2.23798166430732,5.17036322918186));
#13269=CARTESIAN_POINT('Ctrl Pts',(3.59320079576331,2.22432009870508,5.17406782553412));
#13270=CARTESIAN_POINT('Ctrl Pts',(3.64619138280368,2.2396150803554,5.17777242188639));
#13271=CARTESIAN_POINT('Ctrl Pts',(3.69918196984405,2.25491006200572,5.18147701823866));
#13272=CARTESIAN_POINT('Ctrl Pts',(3.74385135850849,2.2991615909086,5.18518161459093));
#13273=CARTESIAN_POINT('Ctrl Pts',(3.75975544882264,2.35186813523316,5.1888862109432));
#13274=CARTESIAN_POINT('Ctrl Pts',(3.7756595391368,2.40457467955771,5.19259080729547));
#13275=CARTESIAN_POINT('Ctrl Pts',(3.76279833110066,2.46573623930395,5.19629540364773));
#13276=CARTESIAN_POINT('Ctrl Pts',(3.72690708798524,2.50793586530485,5.2));
#13277=CARTESIAN_POINT('',(3.47285246768952,2.50812032770478,5.2));
#13278=CARTESIAN_POINT('Origin',(3.6,2.4,5.2));
#13279=CARTESIAN_POINT('Ctrl Pts',(3.47285231527688,2.50812044463164,5.2));
#13280=CARTESIAN_POINT('Ctrl Pts',(3.50793811173714,2.54927258268021,5.19636770818145));
#13281=CARTESIAN_POINT('Ctrl Pts',(3.56493587106976,2.57187757629771,5.19273541636289));
#13282=CARTESIAN_POINT('Ctrl Pts',(3.6186762488644,2.56581789998251,5.18910312454433));
#13283=CARTESIAN_POINT('Ctrl Pts',(3.67348638458382,2.55963759952907,5.18539852819207));
#13284=CARTESIAN_POINT('Ctrl Pts',(3.72490816491496,2.52364007082416,5.1816939318398));
#13285=CARTESIAN_POINT('Ctrl Pts',(3.74944162746499,2.4742589593754,5.17798933548753));
#13286=CARTESIAN_POINT('Ctrl Pts',(3.77397509001502,2.42487784792664,5.17428473913527));
#13287=CARTESIAN_POINT('Ctrl Pts',(3.77162023478396,2.36211315373403,5.17058014278299));
#13288=CARTESIAN_POINT('Ctrl Pts',(3.74343805908691,2.31470980295916,5.16687554643072));
#13289=CARTESIAN_POINT('Ctrl Pts',(3.71525588338986,2.2673064521843,5.16317095007846));
#13290=CARTESIAN_POINT('Ctrl Pts',(3.66124638722683,2.23526444482719,5.15946635372619));
#13291=CARTESIAN_POINT('Ctrl Pts',(3.60613566997566,2.23323785031625,5.15576175737392));
#13292=CARTESIAN_POINT('Ctrl Pts',(3.55102495272448,2.23121125580531,5.15205716102166));
#13293=CARTESIAN_POINT('Ctrl Pts',(3.49481301438516,2.25920007414054,5.14835256466939));
#13294=CARTESIAN_POINT('Ctrl Pts',(3.46322139831185,2.30440012642267,5.14464796831712));
#13295=CARTESIAN_POINT('Ctrl Pts',(3.44390334496103,2.33203964380033,5.14238263343174));
#13296=CARTESIAN_POINT('Ctrl Pts',(3.43379141454156,2.36611485011022,5.14011729854636));
#13297=CARTESIAN_POINT('Ctrl Pts',(3.43361558566414,2.40009421455432,5.13785196366098));
#13298=CARTESIAN_POINT('Origin',(3.6,2.4,5.35459252805377));
#13299=CARTESIAN_POINT('',(3.39427731514299,2.4001195557093,4.34540747194623));
#13300=CARTESIAN_POINT('',(3.39483887138702,2.39991986985508,4.33959252805377));
#13301=CARTESIAN_POINT('',(3.394525,2.40000000000001,5.35459252805377));
#13302=CARTESIAN_POINT('',(3.78826275096636,2.31767678198967,4.3));
#13303=CARTESIAN_POINT('Ctrl Pts',(3.39483887138702,2.39991986985508,4.33959252805377));
#13304=CARTESIAN_POINT('Ctrl Pts',(3.39495667746176,2.43847992884438,4.33750880775932));
#13305=CARTESIAN_POINT('Ctrl Pts',(3.42394163903792,2.54576387140554,4.3317204911126));
#13306=CARTESIAN_POINT('Ctrl Pts',(3.59702533363695,2.64299053446886,4.32222757811361));
#13307=CARTESIAN_POINT('Ctrl Pts',(3.80250223745458,2.5338839434383,4.3111137890568));
#13308=CARTESIAN_POINT('Ctrl Pts',(3.81563717950601,2.38027862564402,4.30370459635227));
#13309=CARTESIAN_POINT('Ctrl Pts',(3.78826275096636,2.31767678198967,4.3));
#13310=CARTESIAN_POINT('',(3.72235838409899,2.2344646706273,4.3));
#13311=CARTESIAN_POINT('Origin',(3.6,2.4,4.3));
#13312=CARTESIAN_POINT('Ctrl Pts',(3.394277315143,2.4001195557093,4.34540747194623));
#13313=CARTESIAN_POINT('Ctrl Pts',(3.39422704674216,2.40728359221916,4.34501772883951));
#13314=CARTESIAN_POINT('Ctrl Pts',(3.39781627947545,2.48249299124839,4.34092338938053));
#13315=CARTESIAN_POINT('Ctrl Pts',(3.49037003538787,2.61673301642169,4.33312445356927));
#13316=CARTESIAN_POINT('Ctrl Pts',(3.72265542052987,2.60960761604941,4.32201066451248));
#13317=CARTESIAN_POINT('Ctrl Pts',(3.84179830935629,2.41200908789601,4.31096917998937));
#13318=CARTESIAN_POINT('Ctrl Pts',(3.77594284069862,2.27417970060314,4.30363229181856));
#13319=CARTESIAN_POINT('Ctrl Pts',(3.72235851517117,2.23446447326397,4.3));
#13320=CARTESIAN_POINT('Origin',(3.6,2.4,5.35459252805377));
#13321=CARTESIAN_POINT('',(3.39480734911062,2.40010265425899,4.41540747194623));
#13322=CARTESIAN_POINT('',(3.39433274005607,2.39985021891194,4.40959252805377));
#13323=CARTESIAN_POINT('',(3.394525,2.40000000000001,5.35459252805377));
#13324=CARTESIAN_POINT('Ctrl Pts',(3.39433274005607,2.39985021891194,4.40959252805377));
#13325=CARTESIAN_POINT('Ctrl Pts',(3.39481384314024,2.45851949137253,4.40640305253959));
#13326=CARTESIAN_POINT('Ctrl Pts',(3.45186169840294,2.58615034863243,4.39950898067315));
#13327=CARTESIAN_POINT('Ctrl Pts',(3.66843098640644,2.63302756431036,4.38891031245443));
#13328=CARTESIAN_POINT('Ctrl Pts',(3.83289206978718,2.4688824684104,4.37779652339763));
#13329=CARTESIAN_POINT('Ctrl Pts',(3.78418106902943,2.24170425860662,4.36668273434082));
#13330=CARTESIAN_POINT('Ctrl Pts',(3.56689371899776,2.15938431325527,4.35556894528402));
#13331=CARTESIAN_POINT('Ctrl Pts',(3.41495577575702,2.27149583748734,4.34653887652167));
#13332=CARTESIAN_POINT('Ctrl Pts',(3.39474723286599,2.36992492448255,4.34121340411158));
#13333=CARTESIAN_POINT('Ctrl Pts',(3.39483887138702,2.39991986985508,4.33959252805377));
#13334=CARTESIAN_POINT('Ctrl Pts',(3.39480734911062,2.40010265425899,4.41540747194623));
#13335=CARTESIAN_POINT('Ctrl Pts',(3.3946821849205,2.42777437678442,4.41391197361979));
#13336=CARTESIAN_POINT('Ctrl Pts',(3.41278383405305,2.52383658927861,4.40871187894108));
#13337=CARTESIAN_POINT('Ctrl Pts',(3.55878722266986,2.63934344974957,4.3998071879101));
#13338=CARTESIAN_POINT('Ctrl Pts',(3.77873475080197,2.56443107632444,4.38869339885329));
#13339=CARTESIAN_POINT('Ctrl Pts',(3.8350828706128,2.33901445723046,4.37757960979649));
#13340=CARTESIAN_POINT('Ctrl Pts',(3.67625990394949,2.16941582752504,4.36646582073968));
#13341=CARTESIAN_POINT('Ctrl Pts',(3.45564722223464,2.20942500090864,4.3557417747896));
#13342=CARTESIAN_POINT('Ctrl Pts',(3.394704859258,2.33918780536763,4.34872232519178));
#13343=CARTESIAN_POINT('Ctrl Pts',(3.394277315143,2.4001195557093,4.34540747194623));
#13344=CARTESIAN_POINT('Origin',(3.6,2.4,5.35459252805377));
#13345=CARTESIAN_POINT('',(3.39465010046741,2.39982347235041,4.48540747194623));
#13346=CARTESIAN_POINT('',(3.39437120031462,2.40016339024638,4.47959252805377));
#13347=CARTESIAN_POINT('',(3.394525,2.40000000000001,5.35459252805377));
#13348=CARTESIAN_POINT('Ctrl Pts',(3.39437120031462,2.40016339024638,4.47959252805377));
#13349=CARTESIAN_POINT('Ctrl Pts',(3.39427672852213,2.41103322262123,4.47900189367213));
#13350=CARTESIAN_POINT('Ctrl Pts',(3.40000383140382,2.48998144241434,4.47470666293823));
#13351=CARTESIAN_POINT('Ctrl Pts',(3.5022614856576,2.62233051762717,4.46670683585207));
#13352=CARTESIAN_POINT('Ctrl Pts',(3.73378446379617,2.60269537158839,4.45559304679526));
#13353=CARTESIAN_POINT('Ctrl Pts',(3.84285303079348,2.39753073097072,4.44447925773845));
#13354=CARTESIAN_POINT('Ctrl Pts',(3.72963541291671,2.19462648510256,4.43336546868165));
#13355=CARTESIAN_POINT('Ctrl Pts',(3.49776113486282,2.17970245626759,4.42225167962485));
#13356=CARTESIAN_POINT('Ctrl Pts',(3.39915518291127,2.31283529949844,4.41432736608222));
#13357=CARTESIAN_POINT('Ctrl Pts',(3.39425503880932,2.39037475353659,4.41010764889186));
#13358=CARTESIAN_POINT('Ctrl Pts',(3.39433274005607,2.39985021891194,4.40959252805377));
#13359=CARTESIAN_POINT('Ctrl Pts',(3.39465010046741,2.39982347235041,4.48540747194623));
#13360=CARTESIAN_POINT('Ctrl Pts',(3.39504368040953,2.44786270507631,4.48280621840007));
#13361=CARTESIAN_POINT('Ctrl Pts',(3.43581223293462,2.56491921556266,4.47650036850162));
#13362=CARTESIAN_POINT('Ctrl Pts',(3.63081864137997,2.64090222813732,4.46648992225093));
#13363=CARTESIAN_POINT('Ctrl Pts',(3.81910984841827,2.50475947107891,4.45537613319412));
#13364=CARTESIAN_POINT('Ctrl Pts',(3.80684730359907,2.27272920356226,4.44426234413732));
#13365=CARTESIAN_POINT('Ctrl Pts',(3.60525512148808,2.15719129638054,4.43314855508051));
#13366=CARTESIAN_POINT('Ctrl Pts',(3.42662677463403,2.24954018398722,4.42353026435015));
#13367=CARTESIAN_POINT('Ctrl Pts',(3.39499223729164,2.35922694980568,4.41761656997206));
#13368=CARTESIAN_POINT('Ctrl Pts',(3.39480734911062,2.40010265425899,4.41540747194623));
#13369=CARTESIAN_POINT('Origin',(3.6,2.4,5.35459252805377));
#13370=CARTESIAN_POINT('',(3.39418405900746,2.40000082772182,4.55540747194623));
#13371=CARTESIAN_POINT('',(3.39484822543359,2.40004689761745,4.54959252805377));
#13372=CARTESIAN_POINT('',(3.394525,2.40000000000001,5.35459252805377));
#13373=CARTESIAN_POINT('Ctrl Pts',(3.39484822543359,2.40004689761745,4.54959252805377));
#13374=CARTESIAN_POINT('Ctrl Pts',(3.3947841161748,2.43145144364515,4.54789613845241));
#13375=CARTESIAN_POINT('Ctrl Pts',(3.41632347620735,2.53135423912678,4.54249515249878));
#13376=CARTESIAN_POINT('Ctrl Pts',(3.57178887938318,2.64122151037363,4.5333895701929));
#13377=CARTESIAN_POINT('Ctrl Pts',(3.78736363324621,2.55452687009752,4.52227578113608));
#13378=CARTESIAN_POINT('Ctrl Pts',(3.83144232915068,2.3263920312721,4.51116199207928));
#13379=CARTESIAN_POINT('Ctrl Pts',(3.66367923564831,2.1656314047897,4.50004820302247));
#13380=CARTESIAN_POINT('Ctrl Pts',(3.44964305208187,2.21653398832958,4.48952504834731));
#13381=CARTESIAN_POINT('Ctrl Pts',(3.39486927759939,2.34285510326715,4.4827064900244));
#13382=CARTESIAN_POINT('Ctrl Pts',(3.39437120031462,2.40016339024638,4.47959252805377));
#13383=CARTESIAN_POINT('Ctrl Pts',(3.39418406069018,2.40000082771773,4.55540747194623));
#13384=CARTESIAN_POINT('Ctrl Pts',(3.39418405804479,2.40004511873352,4.55540505953261));
#13385=CARTESIAN_POINT('Ctrl Pts',(3.39420412805525,2.46810441674863,4.55169805076671));
#13386=CARTESIAN_POINT('Ctrl Pts',(3.46841582920963,2.6041305389052,4.54428644564855));
#13387=CARTESIAN_POINT('Ctrl Pts',(3.70013763173937,2.6212603119689,4.53317265659175));
#13388=CARTESIAN_POINT('Ctrl Pts',(3.84020232447629,2.43586801205837,4.52205886753494));
#13389=CARTESIAN_POINT('Ctrl Pts',(3.76040710518764,2.21764531427324,4.51094507847815));
#13390=CARTESIAN_POINT('Ctrl Pts',(3.53378944408678,2.16633392770918,4.49983128942133));
#13391=CARTESIAN_POINT('Ctrl Pts',(3.40663178603677,2.29085017634376,4.4913187539107));
#13392=CARTESIAN_POINT('Ctrl Pts',(3.39448316034026,2.37944724185309,4.48651081475233));
#13393=CARTESIAN_POINT('Ctrl Pts',(3.39465010046741,2.39982347235041,4.48540747194623));
#13394=CARTESIAN_POINT('Origin',(3.6,2.4,5.35459252805377));
#13395=CARTESIAN_POINT('',(3.3946525152789,2.40017600729827,4.62540747194623));
#13396=CARTESIAN_POINT('',(3.39454318727431,2.3998121083938,4.61959252805377));
#13397=CARTESIAN_POINT('',(3.394525,2.40000000000001,5.35459252805377));
#13398=CARTESIAN_POINT('Ctrl Pts',(3.39454318727431,2.3998121083938,4.61959252805377));
#13399=CARTESIAN_POINT('Ctrl Pts',(3.39501368913604,2.45149296169584,4.61679038323269));
#13400=CARTESIAN_POINT('Ctrl Pts',(3.44097934710978,2.57224452612634,4.61028364205933));
#13401=CARTESIAN_POINT('Ctrl Pts',(3.64379902916374,2.63888350626668,4.60007230453372));
#13402=CARTESIAN_POINT('Ctrl Pts',(3.8244536406683,2.49275908427381,4.5889585154769));
#13403=CARTESIAN_POINT('Ctrl Pts',(3.79966328939795,2.26173122045618,4.57784472642011));
#13404=CARTESIAN_POINT('Ctrl Pts',(3.59211886499353,2.15726233868846,4.56673093736329));
#13405=CARTESIAN_POINT('Ctrl Pts',(3.42236627044389,2.25700668735564,4.55731353790786));
#13406=CARTESIAN_POINT('Ctrl Pts',(3.39492411875798,2.36286981206378,4.55160073480468));
#13407=CARTESIAN_POINT('Ctrl Pts',(3.39484822543359,2.40004689761745,4.54959252805377));
#13408=CARTESIAN_POINT('Ctrl Pts',(3.3946525152789,2.40017600729827,4.62540747194623));
#13409=CARTESIAN_POINT('Ctrl Pts',(3.3944854829676,2.42064195048213,4.62429930431288));
#13410=CARTESIAN_POINT('Ctrl Pts',(3.40670159662045,2.50933048007129,4.61948654032727));
#13411=CARTESIAN_POINT('Ctrl Pts',(3.53409308462842,2.63375189718637,4.61096917998938));
#13412=CARTESIAN_POINT('Ctrl Pts',(3.76064388996454,2.58214612691277,4.59985539093257));
#13413=CARTESIAN_POINT('Ctrl Pts',(3.84015552099323,2.36381994099575,4.58874160187577));
#13414=CARTESIAN_POINT('Ctrl Pts',(3.6998500801025,2.17860977340027,4.57762781281896));
#13415=CARTESIAN_POINT('Ctrl Pts',(3.46820102232696,2.19603680731826,4.56651643617579));
#13416=CARTESIAN_POINT('Ctrl Pts',(3.3941881204111,2.33203010926412,4.55910965588488));
#13417=CARTESIAN_POINT('Ctrl Pts',(3.39418406069018,2.40000082771773,4.55540747194623));
#13418=CARTESIAN_POINT('Origin',(3.6,2.4,5.35459252805377));
#13419=CARTESIAN_POINT('',(3.39480596940119,2.39989608913133,4.69540747194623));
#13420=CARTESIAN_POINT('',(3.394211384704,2.40006787741663,4.68959252805377));
#13421=CARTESIAN_POINT('',(3.394525,2.40000000000001,5.35459252805377));
#13422=CARTESIAN_POINT('Ctrl Pts',(3.394211384704,2.40006787741663,4.68959252805377));
#13423=CARTESIAN_POINT('Ctrl Pts',(3.39419531260529,2.40380178642024,4.68938922436523));
#13424=CARTESIAN_POINT('Ctrl Pts',(3.3959796032358,2.47555925126455,4.68548132432442));
#13425=CARTESIAN_POINT('Ctrl Pts',(3.47964553527297,2.61094664572852,4.67786882793135));
#13426=CARTESIAN_POINT('Ctrl Pts',(3.71195459435803,2.61552228034691,4.66675503887453));
#13427=CARTESIAN_POINT('Ctrl Pts',(3.84179034357568,2.42282792757511,4.65564124981774));
#13428=CARTESIAN_POINT('Ctrl Pts',(3.75031264922961,2.20923891380705,4.64452746076093));
#13429=CARTESIAN_POINT('Ctrl Pts',(3.5212520823821,2.17025568561017,4.63341367170412));
#13430=CARTESIAN_POINT('Ctrl Pts',(3.40385053057498,2.29836868031663,4.62510202746841));
#13431=CARTESIAN_POINT('Ctrl Pts',(3.39439165865867,2.38316790612259,4.62049497958496));
#13432=CARTESIAN_POINT('Ctrl Pts',(3.39454318727431,2.3998121083938,4.61959252805377));
#13433=CARTESIAN_POINT('Ctrl Pts',(3.39480596940119,2.39989608913133,4.69540747194623));
#13434=CARTESIAN_POINT('Ctrl Pts',(3.39499356749685,2.44086040282664,4.69319354909316));
#13435=CARTESIAN_POINT('Ctrl Pts',(3.42673277743261,2.55063876982526,4.68727502988781));
#13436=CARTESIAN_POINT('Ctrl Pts',(3.60557055501943,2.64280164712995,4.67765191433021));
#13437=CARTESIAN_POINT('Ctrl Pts',(3.80701249526159,2.52700195958257,4.6665381252734));
#13438=CARTESIAN_POINT('Ctrl Pts',(3.81897355090948,2.29495593812904,4.65542433621659));
#13439=CARTESIAN_POINT('Ctrl Pts',(3.63050563208088,2.15905793778677,4.6443105471598));
#13440=CARTESIAN_POINT('Ctrl Pts',(3.43569204443384,2.23525749529523,4.63430492573634));
#13441=CARTESIAN_POINT('Ctrl Pts',(3.39504387077152,2.35222445101461,4.62800390066515));
#13442=CARTESIAN_POINT('Ctrl Pts',(3.3946525152789,2.40017600729827,4.62540747194623));
#13443=CARTESIAN_POINT('Origin',(3.6,2.4,5.35459252805377));
#13444=CARTESIAN_POINT('',(3.39427329960995,2.39987978133526,4.76540747194623));
#13445=CARTESIAN_POINT('',(3.3947435825044,2.40014509868052,4.75959252805377));
#13446=CARTESIAN_POINT('',(3.394525,2.40000000000001,5.35459252805377));
#13447=CARTESIAN_POINT('Ctrl Pts',(3.3947435825044,2.40014509868052,4.75959252805377));
#13448=CARTESIAN_POINT('Ctrl Pts',(3.39458577035565,2.4243482239957,4.7582834691455));
#13449=CARTESIAN_POINT('Ctrl Pts',(3.40973683471182,2.51685424764646,4.75326981388497));
#13450=CARTESIAN_POINT('Ctrl Pts',(3.54682833602434,2.63697354002902,4.74455156227216));
#13451=CARTESIAN_POINT('Ctrl Pts',(3.77025746491439,2.57319376479756,4.73343777321537));
#13452=CARTESIAN_POINT('Ctrl Pts',(3.83784800531731,2.35088777249601,4.72232398415856));
#13453=CARTESIAN_POINT('Ctrl Pts',(3.68773356907346,2.1735347589994,4.71121019510175));
#13454=CARTESIAN_POINT('Ctrl Pts',(3.46153062024069,2.20292038334059,4.70029970973349));
#13455=CARTESIAN_POINT('Ctrl Pts',(3.3944881781145,2.3357625601094,4.6930938207175));
#13456=CARTESIAN_POINT('Ctrl Pts',(3.394211384704,2.40006787741663,4.68959252805377));
#13457=CARTESIAN_POINT('Ctrl Pts',(3.39427329960995,2.39987978133526,4.76540747194623));
#13458=CARTESIAN_POINT('Ctrl Pts',(3.39469744196064,2.4608980648022,4.76208779387343));
#13459=CARTESIAN_POINT('Ctrl Pts',(3.45579877538026,2.59074744458416,4.75506351944837));
#13460=CARTESIAN_POINT('Ctrl Pts',(3.67655778221991,2.63048335496042,4.74433464867103));
#13461=CARTESIAN_POINT('Ctrl Pts',(3.8351627244929,2.46068083668937,4.73322085961423));
#13462=CARTESIAN_POINT('Ctrl Pts',(3.77852055811084,2.23533646042905,4.72210707055742));
#13463=CARTESIAN_POINT('Ctrl Pts',(3.55847650032912,2.16071048934957,4.71099328150062));
#13464=CARTESIAN_POINT('Ctrl Pts',(3.41270208696854,2.27634402495147,4.70209341529689));
#13465=CARTESIAN_POINT('Ctrl Pts',(3.39467965627817,2.37231409061976,4.69689814544543));
#13466=CARTESIAN_POINT('Ctrl Pts',(3.39480596940119,2.39989608913133,4.69540747194623));
#13467=CARTESIAN_POINT('Origin',(3.6,2.4,5.35459252805377));
#13468=CARTESIAN_POINT('',(3.39444175184043,2.40017991402784,4.83540747194624));
#13469=CARTESIAN_POINT('',(3.39473574996246,2.39985120338455,4.82959252805377));
#13470=CARTESIAN_POINT('',(3.394525,2.40000000000001,5.35459252805377));
#13471=CARTESIAN_POINT('Ctrl Pts',(3.39473574996246,2.39985120338455,4.82959252805377));
#13472=CARTESIAN_POINT('Ctrl Pts',(3.39503501794323,2.44449429908603,4.82717771392578));
#13473=CARTESIAN_POINT('Ctrl Pts',(3.43129921147106,2.55806759504416,4.82105830344552));
#13474=CARTESIAN_POINT('Ctrl Pts',(3.61869057107309,2.64214530157901,4.811234296613));
#13475=CARTESIAN_POINT('Ctrl Pts',(3.81357662871545,2.51562312999728,4.80012050755618));
#13476=CARTESIAN_POINT('Ctrl Pts',(3.81297357597085,2.28326979627357,4.78900671849939));
#13477=CARTESIAN_POINT('Ctrl Pts',(3.61743339385551,2.1577609418312,4.77789292944258));
#13478=CARTESIAN_POINT('Ctrl Pts',(3.43084782690273,2.24264334099221,4.76808819929404));
#13479=CARTESIAN_POINT('Ctrl Pts',(3.39503237387128,2.35585412553307,4.76198806549777));
#13480=CARTESIAN_POINT('Ctrl Pts',(3.3947435825044,2.40014509868052,4.75959252805377));
#13481=CARTESIAN_POINT('Ctrl Pts',(3.39444175184043,2.40017991402784,4.83540747194624));
#13482=CARTESIAN_POINT('Ctrl Pts',(3.39432006446725,2.41345772041588,4.83468663500598));
#13483=CARTESIAN_POINT('Ctrl Pts',(3.40154214948563,2.49484232576125,4.83026120171345));
#13484=CARTESIAN_POINT('Ctrl Pts',(3.51011506296999,2.62561996593247,4.82213117206865));
#13485=CARTESIAN_POINT('Ctrl Pts',(3.74080745251389,2.59788110634618,4.81101738301186));
#13486=CARTESIAN_POINT('Ctrl Pts',(3.84261718390667,2.38901942599691,4.79990359395504));
#13487=CARTESIAN_POINT('Ctrl Pts',(3.72235665540369,2.19020838956081,4.78878980489825));
#13488=CARTESIAN_POINT('Ctrl Pts',(3.49010169259086,2.18342199335841,4.77767601584144));
#13489=CARTESIAN_POINT('Ctrl Pts',(3.3977657456792,2.31768599948744,4.76988190485744));
#13490=CARTESIAN_POINT('Ctrl Pts',(3.39422412009908,2.39280468183069,4.7657923902257));
#13491=CARTESIAN_POINT('Ctrl Pts',(3.39427329960995,2.39987978133526,4.76540747194623));
#13492=CARTESIAN_POINT('Origin',(3.6,2.4,5.35459252805377));
#13493=CARTESIAN_POINT('',(3.39485784124953,2.40000781019044,4.90540747194623));
#13494=CARTESIAN_POINT('',(3.39420665921585,2.39993826201568,4.89959252805377));
#13495=CARTESIAN_POINT('',(3.394525,2.40000000000001,5.35459252805377));
#13496=CARTESIAN_POINT('Ctrl Pts',(3.39420665921585,2.39993826201568,4.89959252805377));
#13497=CARTESIAN_POINT('Ctrl Pts',(3.39446259615796,2.46459365987715,4.89607195870605));
#13498=CARTESIAN_POINT('Ctrl Pts',(3.46215556435864,2.59774588363475,4.88884679300606));
#13499=CARTESIAN_POINT('Ctrl Pts',(3.68890792061744,2.62600678347214,4.87791703095382));
#13500=CARTESIAN_POINT('Ctrl Pts',(3.83809973223177,2.44787694680091,4.86680324189701));
#13501=CARTESIAN_POINT('Ctrl Pts',(3.76935615869971,2.22592479776177,4.85568945284022));
#13502=CARTESIAN_POINT('Ctrl Pts',(3.54559897248035,2.16330565547811,4.8445756637834));
#13503=CARTESIAN_POINT('Ctrl Pts',(3.40943456861369,2.28386778049975,4.83587668885459));
#13504=CARTESIAN_POINT('Ctrl Pts',(3.39457590721621,2.37600677138249,4.83088231027805));
#13505=CARTESIAN_POINT('Ctrl Pts',(3.39473574996246,2.39985120338455,4.82959252805377));
#13506=CARTESIAN_POINT('Ctrl Pts',(3.39485784124953,2.40000781019044,4.90540747194623));
#13507=CARTESIAN_POINT('Ctrl Pts',(3.39484637525965,2.43382668251502,4.90358087978625));
#13508=CARTESIAN_POINT('Ctrl Pts',(3.41876409372263,2.5362199118863,4.898049691274));
#13509=CARTESIAN_POINT('Ctrl Pts',(3.58026192098975,2.64206213906777,4.88881390640948));
#13510=CARTESIAN_POINT('Ctrl Pts',(3.79266519873933,2.54786410019675,4.87770011735268));
#13511=CARTESIAN_POINT('Ctrl Pts',(3.82871983510845,2.3183243735256,4.86658632829587));
#13512=CARTESIAN_POINT('Ctrl Pts',(3.65542461254465,2.16354327402962,4.85547253923907));
#13513=CARTESIAN_POINT('Ctrl Pts',(3.44592887095679,2.22119506991598,4.84507958712252));
#13514=CARTESIAN_POINT('Ctrl Pts',(3.39494545222641,2.34521910726469,4.83839123135825));
#13515=CARTESIAN_POINT('Ctrl Pts',(3.39444175184043,2.40017991402784,4.83540747194624));
#13516=CARTESIAN_POINT('Origin',(3.6,2.4,5.35459252805377));
#13517=CARTESIAN_POINT('',(3.39447042093573,2.39981603086916,4.97540747194623));
#13518=CARTESIAN_POINT('',(3.39455384621585,2.40018770306997,4.96959252805377));
#13519=CARTESIAN_POINT('',(3.394525,2.40000000000001,5.35459252805377));
#13520=CARTESIAN_POINT('Ctrl Pts',(3.39455384621585,2.40018770306997,4.96959252805377));
#13521=CARTESIAN_POINT('Ctrl Pts',(3.39439993536132,2.41718968163228,4.9686707998386));
#13522=CARTESIAN_POINT('Ctrl Pts',(3.40410689916048,2.50235241402357,4.96404447527116));
#13523=CARTESIAN_POINT('Ctrl Pts',(3.52244569778922,2.63014998309056,4.95571355435144));
#13524=CARTESIAN_POINT('Ctrl Pts',(3.7513008249214,2.58997827483123,4.94459976529465));
#13525=CARTESIAN_POINT('Ctrl Pts',(3.84166859114005,2.37591729705878,4.93348597623783));
#13526=CARTESIAN_POINT('Ctrl Pts',(3.71083435517744,2.18389949043478,4.92237218718104));
#13527=CARTESIAN_POINT('Ctrl Pts',(3.47855217697512,2.18968093094735,4.91125839812423));
#13528=CARTESIAN_POINT('Ctrl Pts',(3.39580021960588,2.32515686494945,4.90366517841514));
#13529=CARTESIAN_POINT('Ctrl Pts',(3.39419328089429,2.3965585986654,4.89977655505832));
#13530=CARTESIAN_POINT('Ctrl Pts',(3.39420665921585,2.39993826201568,4.89959252805377));
#13531=CARTESIAN_POINT('Ctrl Pts',(3.39447042093573,2.39981603086916,4.97540747194623));
#13532=CARTESIAN_POINT('Ctrl Pts',(3.39496908070531,2.45384921408654,4.97247512456653));
#13533=CARTESIAN_POINT('Ctrl Pts',(3.44450059321654,2.57695438413994,4.96583818083455));
#13534=CARTESIAN_POINT('Ctrl Pts',(3.652145851588,2.63720135146115,4.95549664075031));
#13535=CARTESIAN_POINT('Ctrl Pts',(3.82756721950384,2.48483414141864,4.9443828516935));
#13536=CARTESIAN_POINT('Ctrl Pts',(3.79469373046592,2.25481727983819,4.9332690626367));
#13537=CARTESIAN_POINT('Ctrl Pts',(3.58361486203243,2.15768780841241,4.9221552735799));
#13538=CARTESIAN_POINT('Ctrl Pts',(3.41976019074743,2.26186083674666,4.91286807668307));
#13539=CARTESIAN_POINT('Ctrl Pts',(3.39486962996599,2.36523705764074,4.90728547613852));
#13540=CARTESIAN_POINT('Ctrl Pts',(3.39485784124953,2.40000781019044,4.90540747194623));
#13541=CARTESIAN_POINT('Origin',(3.6,2.4,5.35459252805377));
#13542=CARTESIAN_POINT('',(3.3942529072965,2.40010656251954,5.04540747194623));
#13543=CARTESIAN_POINT('',(3.39484564919972,2.39994744459104,5.03959252805377));
#13544=CARTESIAN_POINT('',(3.394525,2.40000000000001,5.35459252805377));
#13545=CARTESIAN_POINT('Ctrl Pts',(3.39484564919972,2.39994744459104,5.03959252805377));
#13546=CARTESIAN_POINT('Ctrl Pts',(3.39493157223083,2.43748021568483,5.03756504461887));
#13547=CARTESIAN_POINT('Ctrl Pts',(3.42276238606253,2.54371108636155,5.03183296483171));
#13548=CARTESIAN_POINT('Ctrl Pts',(3.59337897158896,2.64277529828296,5.02239628869227));
#13549=CARTESIAN_POINT('Ctrl Pts',(3.80037832359127,2.53723050760561,5.01128249963547));
#13550=CARTESIAN_POINT('Ctrl Pts',(3.82396912389365,2.30607707315216,5.00016871057866));
#13551=CARTESIAN_POINT('Ctrl Pts',(3.64255844494981,2.16089236073089,4.98905492152186));
#13552=CARTESIAN_POINT('Ctrl Pts',(3.44046962361553,2.22845545212382,4.97886286068023));
#13553=CARTESIAN_POINT('Ctrl Pts',(3.39501853158186,2.34885558191993,4.97237539619086));
#13554=CARTESIAN_POINT('Ctrl Pts',(3.39455384621585,2.40018770306997,4.96959252805377));
#13555=CARTESIAN_POINT('Ctrl Pts',(3.3942529072965,2.40010656251954,5.04540747194623));
#13556=CARTESIAN_POINT('Ctrl Pts',(3.39421422426863,2.40623506914945,5.04507396569907));
#13557=CARTESIAN_POINT('Ctrl Pts',(3.39724233203131,2.4804004332851,5.04103586309963));
#13558=CARTESIAN_POINT('Ctrl Pts',(3.48711398178203,2.61503583311392,5.03329316414794));
#13559=CARTESIAN_POINT('Ctrl Pts',(3.71944062032543,2.61146538882495,5.02217937509113));
#13560=CARTESIAN_POINT('Ctrl Pts',(3.84244192441188,2.41433825182845,5.01106558603433));
#13561=CARTESIAN_POINT('Ctrl Pts',(3.74353337567863,2.20408716238119,4.99995179697753));
#13562=CARTESIAN_POINT('Ctrl Pts',(3.51324710536571,2.17315730898832,4.98883800792072));
#13563=CARTESIAN_POINT('Ctrl Pts',(3.40217617393534,2.30323677769677,4.98065656624362));
#13564=CARTESIAN_POINT('Ctrl Pts',(3.39433909628525,2.38558611032407,4.97617972091879));
#13565=CARTESIAN_POINT('Ctrl Pts',(3.39447042093573,2.39981603086916,4.97540747194623));
#13566=CARTESIAN_POINT('Origin',(3.6,2.4,5.35459252805377));
#13567=CARTESIAN_POINT('',(3.39479089114249,2.40011619889285,5.11540747194623));
#13568=CARTESIAN_POINT('',(3.39436118415265,2.39983962587988,5.10959252805377));
#13569=CARTESIAN_POINT('',(3.394525,2.40000000000001,5.35459252805377));
#13570=CARTESIAN_POINT('Ctrl Pts',(3.39436118415265,2.39983962587988,5.10959252805377));
#13571=CARTESIAN_POINT('Ctrl Pts',(3.39485594839208,2.45749534742618,5.10645928939915));
#13572=CARTESIAN_POINT('Ctrl Pts',(3.45020483086988,2.58415305598872,5.09962145439226));
#13573=CARTESIAN_POINT('Ctrl Pts',(3.66489494817768,2.63403475512075,5.08907902303309));
#13574=CARTESIAN_POINT('Ctrl Pts',(3.83182128848718,2.47240567698227,5.0779652339763));
#13575=CARTESIAN_POINT('Ctrl Pts',(3.78655899556261,2.24450261226871,5.06685144491949));
#13576=CARTESIAN_POINT('Ctrl Pts',(3.57053712771522,2.15892819449186,5.05573765586269));
#13577=CARTESIAN_POINT('Ctrl Pts',(3.41597203014558,2.26936665662614,5.04665135024078));
#13578=CARTESIAN_POINT('Ctrl Pts',(3.39477457457446,2.36890073212835,5.04126964097114));
#13579=CARTESIAN_POINT('Ctrl Pts',(3.39484564919972,2.39994744459104,5.03959252805377));
#13580=CARTESIAN_POINT('Ctrl Pts',(3.39479089114249,2.40011619889285,5.11540747194623));
#13581=CARTESIAN_POINT('Ctrl Pts',(3.39465311263348,2.42674223574529,5.11396821047934));
#13582=CARTESIAN_POINT('Ctrl Pts',(3.4118399484044,2.5217320012959,5.10882435266019));
#13583=CARTESIAN_POINT('Ctrl Pts',(3.55516852834243,2.63869087044012,5.09997589848876));
#13584=CARTESIAN_POINT('Ctrl Pts',(3.77622353148193,2.56711958879047,5.08886210943196));
#13585=CARTESIAN_POINT('Ctrl Pts',(3.8359804180852,2.34258029751366,5.07774832037515));
#13586=CARTESIAN_POINT('Ctrl Pts',(3.6797411123384,2.17059868763558,5.06663453131835));
#13587=CARTESIAN_POINT('Ctrl Pts',(3.45739289886954,2.2074502474941,5.05585424850871));
#13588=CARTESIAN_POINT('Ctrl Pts',(3.39464391638139,2.33815945287815,5.04877856205133));
#13589=CARTESIAN_POINT('Ctrl Pts',(3.3942529072965,2.40010656251954,5.04540747194623));
#13590=CARTESIAN_POINT('Origin',(3.6,2.4,5.35459252805377));
#13591=CARTESIAN_POINT('',(3.39473291096846,2.39977036782444,5.18540747194623));
#13592=CARTESIAN_POINT('',(3.39434265438876,2.4001499379742,5.17959252805377));
#13593=CARTESIAN_POINT('',(3.394525,2.40000000000001,5.35459252805377));
#13594=CARTESIAN_POINT('',(3.54698297828114,2.20148256743283,5.2));
#13595=CARTESIAN_POINT('Ctrl Pts',(3.54698297828114,2.20148256743283,5.2));
#13596=CARTESIAN_POINT('Ctrl Pts',(3.48097120902544,2.21911198848201,5.19629540364773));
#13597=CARTESIAN_POINT('Ctrl Pts',(3.40750559920538,2.28872805295596,5.19143122762981));
#13598=CARTESIAN_POINT('Ctrl Pts',(3.39457126112442,2.3783468402669,5.18656705161189));
#13599=CARTESIAN_POINT('Ctrl Pts',(3.39473291096846,2.39977036782444,5.18540747194623));
#13600=CARTESIAN_POINT('',(3.6531315533849,2.20112677566065,5.2));
#13601=CARTESIAN_POINT('Origin',(3.6,2.4,5.2));
#13602=CARTESIAN_POINT('Ctrl Pts',(3.65313162618093,2.20112654952031,5.2));
#13603=CARTESIAN_POINT('Ctrl Pts',(3.58867175365004,2.1839946978326,5.19636770818145));
#13604=CARTESIAN_POINT('Ctrl Pts',(3.45069166079049,2.21593288928867,5.1895652175327));
#13605=CARTESIAN_POINT('Ctrl Pts',(3.39482801182151,2.34184093155955,5.18276272688396));
#13606=CARTESIAN_POINT('Ctrl Pts',(3.39434265438876,2.4001499379742,5.17959252805377));
#13607=CARTESIAN_POINT('Origin',(3.6,-2.4,4.7));
#13608=CARTESIAN_POINT('',(3.4332441194689,-2.40012144310043,4.38714803633902));
#13609=CARTESIAN_POINT('',(3.43319918361158,-2.39990306414324,4.36785196366098));
#13610=CARTESIAN_POINT('',(3.4334,-2.4,4.7));
#13611=CARTESIAN_POINT('',(3.43648706727485,-2.43192304546281,4.3));
#13612=CARTESIAN_POINT('Ctrl Pts',(3.43319918361158,-2.39990306414324,4.36785196366098));
#13613=CARTESIAN_POINT('Ctrl Pts',(3.43315842575224,-2.39409443322767,4.36746222055426));
#13614=CARTESIAN_POINT('Ctrl Pts',(3.43343544638748,-2.38828969410672,4.36707247744754));
#13615=CARTESIAN_POINT('Ctrl Pts',(3.43404308035483,-2.38251974365232,4.36668273434082));
#13616=CARTESIAN_POINT('Ctrl Pts',(3.43981877860357,-2.32767505996788,4.36297813798856));
#13617=CARTESIAN_POINT('Ctrl Pts',(3.47546516768456,-2.27597350876472,4.35927354163629));
#13618=CARTESIAN_POINT('Ctrl Pts',(3.52467802663468,-2.2510856178596,4.35556894528402));
#13619=CARTESIAN_POINT('Ctrl Pts',(3.57389088558479,-2.22619772695447,4.35186434893175));
#13620=CARTESIAN_POINT('Ctrl Pts',(3.63667021440403,-2.22812349634739,4.34815975257949));
#13621=CARTESIAN_POINT('Ctrl Pts',(3.68426556377096,-2.25596352517201,4.34445515622722));
#13622=CARTESIAN_POINT('Ctrl Pts',(3.73186091313788,-2.28380355399663,4.34075055987495));
#13623=CARTESIAN_POINT('Ctrl Pts',(3.7642722830525,-2.33755784225296,4.33704596352268));
#13624=CARTESIAN_POINT('Ctrl Pts',(3.76670489686818,-2.39266164590465,4.33334136717041));
#13625=CARTESIAN_POINT('Ctrl Pts',(3.76913751068386,-2.44776544955635,4.32963677081814));
#13626=CARTESIAN_POINT('Ctrl Pts',(3.74159136840061,-2.50421876860342,4.32593217446587));
#13627=CARTESIAN_POINT('Ctrl Pts',(3.69659414024548,-2.53611221831126,4.32222757811361));
#13628=CARTESIAN_POINT('Ctrl Pts',(3.65159691209034,-2.56800566801911,4.31852298176134));
#13629=CARTESIAN_POINT('Ctrl Pts',(3.58914859806332,-2.57533924838774,4.31481838540907));
#13630=CARTESIAN_POINT('Ctrl Pts',(3.53802492988379,-2.55491157781525,4.3111137890568));
#13631=CARTESIAN_POINT('Ctrl Pts',(3.48690126170426,-2.53448390724277,4.30740919270454));
#13632=CARTESIAN_POINT('Ctrl Pts',(3.44710223937223,-2.48629498572918,4.30370459635227));
#13633=CARTESIAN_POINT('Ctrl Pts',(3.43648706727485,-2.43192304546281,4.3));
#13634=CARTESIAN_POINT('',(3.59474332937116,-2.23318013131002,4.3));
#13635=CARTESIAN_POINT('Origin',(3.6,-2.4,4.3));
#13636=CARTESIAN_POINT('',(3.43365449489478,-2.40006497081539,4.31714803633902));
#13637=CARTESIAN_POINT('Ctrl Pts',(3.5947433329992,-2.23317993884958,4.3));
#13638=CARTESIAN_POINT('Ctrl Pts',(3.54069367702075,-2.23495318942066,4.30363229181855));
#13639=CARTESIAN_POINT('Ctrl Pts',(3.48748281579126,-2.26542182682866,4.30726458363711));
#13640=CARTESIAN_POINT('Ctrl Pts',(3.45871387185408,-2.31121589220503,4.31089687545567));
#13641=CARTESIAN_POINT('Ctrl Pts',(3.44221012289161,-2.33748636499654,4.31298059575012));
#13642=CARTESIAN_POINT('Ctrl Pts',(3.43375001435867,-2.36880031414598,4.31506431604457));
#13643=CARTESIAN_POINT('Ctrl Pts',(3.43365449489478,-2.40006497081539,4.31714803633902));
#13644=CARTESIAN_POINT('',(3.4334,-2.4,4.2));
#13645=CARTESIAN_POINT('',(3.4334,-2.4,4.7));
#13646=CARTESIAN_POINT('Origin',(3.6,-2.4,4.2));
#13647=CARTESIAN_POINT('Ctrl Pts',(3.43365449489478,-2.40006497081539,4.31714803633902));
#13648=CARTESIAN_POINT('Ctrl Pts',(3.43358019259399,-2.42438499763772,4.31876891239684));
#13649=CARTESIAN_POINT('Ctrl Pts',(3.43856722876717,-2.44867519801865,4.32038978845465));
#13650=CARTESIAN_POINT('Ctrl Pts',(3.44876666940262,-2.4705384776482,4.32201066451247));
#13651=CARTESIAN_POINT('Ctrl Pts',(3.47207802031749,-2.52050813792769,4.32571526086474));
#13652=CARTESIAN_POINT('Ctrl Pts',(3.52261765592676,-2.55780017703868,4.329419857217));
#13653=CARTESIAN_POINT('Ctrl Pts',(3.57725038923478,-2.56532196913419,4.33312445356927));
#13654=CARTESIAN_POINT('Ctrl Pts',(3.6318831225428,-2.57284376122971,4.33682904992154));
#13655=CARTESIAN_POINT('Ctrl Pts',(3.69060895354956,-2.55059530630975,4.34053364627381));
#13656=CARTESIAN_POINT('Ctrl Pts',(3.72655438362155,-2.50877157126828,4.34423824262608));
#13657=CARTESIAN_POINT('Ctrl Pts',(3.76249981369354,-2.4669478362268,4.34794283897835));
#13658=CARTESIAN_POINT('Ctrl Pts',(3.77566484283074,-2.40554882106382,4.35164743533061));
#13659=CARTESIAN_POINT('Ctrl Pts',(3.76002306731497,-2.35266772394791,4.35535203168288));
#13660=CARTESIAN_POINT('Ctrl Pts',(3.74438129179919,-2.29978662683201,4.35905662803515));
#13661=CARTESIAN_POINT('Ctrl Pts',(3.69993271163044,-2.25542344776319,4.36276122438742));
#13662=CARTESIAN_POINT('Ctrl Pts',(3.64702014743753,-2.23988444780227,4.36646582073969));
#13663=CARTESIAN_POINT('Ctrl Pts',(3.59410758324462,-2.22434544784136,4.37017041709196));
#13664=CARTESIAN_POINT('Ctrl Pts',(3.53273103502755,-2.23763062698835,4.37387501344422));
#13665=CARTESIAN_POINT('Ctrl Pts',(3.49097949059372,-2.27365834937589,4.37757960979649));
#13666=CARTESIAN_POINT('Ctrl Pts',(3.45503346139427,-2.30467644890953,4.38076908531067));
#13667=CARTESIAN_POINT('Ctrl Pts',(3.43363419992272,-2.35255214998637,4.38395856082484));
#13668=CARTESIAN_POINT('Ctrl Pts',(3.4332441194689,-2.40012144310043,4.38714803633902));
#13669=CARTESIAN_POINT('Origin',(3.6,-2.4,4.7));
#13670=CARTESIAN_POINT('',(3.4332753032246,-2.39986752249821,4.45714803633902));
#13671=CARTESIAN_POINT('',(3.43362893615635,-2.39991676750829,4.43785196366098));
#13672=CARTESIAN_POINT('',(3.4334,-2.4,4.7));
#13673=CARTESIAN_POINT('Ctrl Pts',(3.43362893615635,-2.39991676750829,4.43785196366098));
#13674=CARTESIAN_POINT('Ctrl Pts',(3.43352745251214,-2.37748041857078,4.43635646533454));
#13675=CARTESIAN_POINT('Ctrl Pts',(3.43774838897563,-2.35508066415019,4.43486096700809));
#13676=CARTESIAN_POINT('Ctrl Pts',(3.44647311482898,-2.33459946287839,4.43336546868165));
#13677=CARTESIAN_POINT('Ctrl Pts',(3.46808570175023,-2.28386414463698,4.42966087232938));
#13678=CARTESIAN_POINT('Ctrl Pts',(3.51733510423541,-2.24490173470295,4.42595627597711));
#13679=CARTESIAN_POINT('Ctrl Pts',(3.57168220229163,-2.23554374099052,4.42225167962485));
#13680=CARTESIAN_POINT('Ctrl Pts',(3.62602930034785,-2.22618574727809,4.41854708327258));
#13681=CARTESIAN_POINT('Ctrl Pts',(3.68547409397512,-2.24643216978725,4.41484248692031));
#13682=CARTESIAN_POINT('Ctrl Pts',(3.72281103935986,-2.2870168380163,4.41113789056804));
#13683=CARTESIAN_POINT('Ctrl Pts',(3.7601479847446,-2.32760150624535,4.40743329421577));
#13684=CARTESIAN_POINT('Ctrl Pts',(3.77537708188681,-2.38852442019428,4.4037286978635));
#13685=CARTESIAN_POINT('Ctrl Pts',(3.76152924259544,-2.44190442427593,4.40002410151124));
#13686=CARTESIAN_POINT('Ctrl Pts',(3.74768140330407,-2.49528442835759,4.39631950515897));
#13687=CARTESIAN_POINT('Ctrl Pts',(3.70475662757912,-2.54112152257198,4.3926149088067));
#13688=CARTESIAN_POINT('Ctrl Pts',(3.65239849228647,-2.55843697682615,4.38891031245443));
#13689=CARTESIAN_POINT('Ctrl Pts',(3.60004035699382,-2.57575243108032,4.38520571610217));
#13690=CARTESIAN_POINT('Ctrl Pts',(3.53824886213347,-2.56454624537428,4.3815011197499));
#13691=CARTESIAN_POINT('Ctrl Pts',(3.49530561841154,-2.52994924443839,4.37779652339763));
#13692=CARTESIAN_POINT('Ctrl Pts',(3.45688023078761,-2.49899203076829,4.37448167015208));
#13693=CARTESIAN_POINT('Ctrl Pts',(3.43354583842081,-2.4493067834413,4.37116681690653));
#13694=CARTESIAN_POINT('Ctrl Pts',(3.43319918361158,-2.39990306414324,4.36785196366098));
#13695=CARTESIAN_POINT('Ctrl Pts',(3.4332441194689,-2.40012144310043,4.38714803633902));
#13696=CARTESIAN_POINT('Ctrl Pts',(3.4331811189632,-2.40780419031934,4.38766315717711));
#13697=CARTESIAN_POINT('Ctrl Pts',(3.43366612887655,-2.41547894509172,4.3881782780152));
#13698=CARTESIAN_POINT('Ctrl Pts',(3.43472637398198,-2.42307339909524,4.3886933988533));
#13699=CARTESIAN_POINT('Ctrl Pts',(3.44235134245467,-2.47769046079897,4.39239799520556));
#13700=CARTESIAN_POINT('Ctrl Pts',(3.47972782005064,-2.52815431857834,4.39610259155783));
#13701=CARTESIAN_POINT('Ctrl Pts',(3.5297501656918,-2.5513695031952,4.3998071879101));
#13702=CARTESIAN_POINT('Ctrl Pts',(3.57977251133296,-2.57458468781207,4.40351178426237));
#13703=CARTESIAN_POINT('Ctrl Pts',(3.64244072501932,-2.57055119926642,4.40721638061463));
#13704=CARTESIAN_POINT('Ctrl Pts',(3.68907438543537,-2.54111518550135,4.4109209769669));
#13705=CARTESIAN_POINT('Ctrl Pts',(3.73570804585142,-2.51167917173628,4.41462557331917));
#13706=CARTESIAN_POINT('Ctrl Pts',(3.76630715299715,-2.4568406327518,4.41833016967144));
#13707=CARTESIAN_POINT('Ctrl Pts',(3.76686783098938,-2.40169663747488,4.42203476602371));
#13708=CARTESIAN_POINT('Ctrl Pts',(3.7674285089816,-2.34655264219797,4.42573936237597));
#13709=CARTESIAN_POINT('Ctrl Pts',(3.73795075782031,-2.29110319062863,4.42944395872824));
#13710=CARTESIAN_POINT('Ctrl Pts',(3.69192524795617,-2.26072508833266,4.43314855508051));
#13711=CARTESIAN_POINT('Ctrl Pts',(3.64589973809204,-2.23034698603669,4.43685315143278));
#13712=CARTESIAN_POINT('Ctrl Pts',(3.58332646952505,-2.2250402330141,4.44055774778505));
#13713=CARTESIAN_POINT('Ctrl Pts',(3.53284244819528,-2.24723347009038,4.44426234413732));
#13714=CARTESIAN_POINT('Ctrl Pts',(3.48235842686551,-2.26942670716666,4.44796694048958));
#13715=CARTESIAN_POINT('Ctrl Pts',(3.44396365277294,-2.31911993434182,4.45167153684185));
#13716=CARTESIAN_POINT('Ctrl Pts',(3.43522971460805,-2.37357077679719,4.45537613319412));
#13717=CARTESIAN_POINT('Ctrl Pts',(3.43383723789082,-2.38225203019296,4.45596676757575));
#13718=CARTESIAN_POINT('Ctrl Pts',(3.4331987050974,-2.39105421663124,4.45655740195739));
#13719=CARTESIAN_POINT('Ctrl Pts',(3.4332753032246,-2.39986752249821,4.45714803633902));
#13720=CARTESIAN_POINT('Origin',(3.6,-2.4,4.7));
#13721=CARTESIAN_POINT('',(3.43366207720083,-2.39996197521424,4.52714803633902));
#13722=CARTESIAN_POINT('',(3.43350143827108,-2.40014312936039,4.50785196366098));
#13723=CARTESIAN_POINT('',(3.4334,-2.4,4.7));
#13724=CARTESIAN_POINT('Ctrl Pts',(3.43350143827108,-2.40014312936039,4.50785196366098));
#13725=CARTESIAN_POINT('Ctrl Pts',(3.43382055454292,-2.36119271753362,4.50525071011481));
#13726=CARTESIAN_POINT('Ctrl Pts',(3.44745634567654,-2.3220410177822,4.50264945656865));
#13727=CARTESIAN_POINT('Ctrl Pts',(3.4724157519356,-2.29243605104842,4.50004820302248));
#13728=CARTESIAN_POINT('Ctrl Pts',(3.50796189295608,-2.25027389736965,4.49634360667021));
#13729=CARTESIAN_POINT('Ctrl Pts',(3.56647488846456,-2.22747467908062,4.49263901031794));
#13730=CARTESIAN_POINT('Ctrl Pts',(3.62117593657879,-2.23447258988711,4.48893441396567));
#13731=CARTESIAN_POINT('Ctrl Pts',(3.67587698469302,-2.2414705006936,4.4852298176134));
#13732=CARTESIAN_POINT('Ctrl Pts',(3.726766085413,-2.27826554059562,4.48152522126114));
#13733=CARTESIAN_POINT('Ctrl Pts',(3.75055354862185,-2.32801824658462,4.47782062490887));
#13734=CARTESIAN_POINT('Ctrl Pts',(3.7743410118307,-2.37777095257363,4.4741160285566));
#13735=CARTESIAN_POINT('Ctrl Pts',(3.77102683752841,-2.44048132464963,4.47041143220433));
#13736=CARTESIAN_POINT('Ctrl Pts',(3.74212778560952,-2.48744961415947,4.46670683585206));
#13737=CARTESIAN_POINT('Ctrl Pts',(3.71322873369063,-2.53441790366931,4.4630022394998));
#13738=CARTESIAN_POINT('Ctrl Pts',(3.65874480415513,-2.56564411061299,4.45929764314753));
#13739=CARTESIAN_POINT('Ctrl Pts',(3.60361085781629,-2.56683736686161,4.45559304679526));
#13740=CARTESIAN_POINT('Ctrl Pts',(3.54847691147744,-2.56803062311024,4.45188845044299));
#13741=CARTESIAN_POINT('Ctrl Pts',(3.49269294833524,-2.5391909286638,4.44818385409072));
#13742=CARTESIAN_POINT('Ctrl Pts',(3.46178885244281,-2.49351696816619,4.44447925773846));
#13743=CARTESIAN_POINT('Ctrl Pts',(3.44336034614035,-2.46628100333426,4.44227015971263));
#13744=CARTESIAN_POINT('Ctrl Pts',(3.43377884425998,-2.43305896049386,4.4400610616868));
#13745=CARTESIAN_POINT('Ctrl Pts',(3.43362893615635,-2.39991676750829,4.43785196366098));
#13746=CARTESIAN_POINT('Ctrl Pts',(3.4332753032246,-2.39986752249821,4.45714803633902));
#13747=CARTESIAN_POINT('Ctrl Pts',(3.43367914638464,-2.44633332293026,4.46026199830965));
#13748=CARTESIAN_POINT('Ctrl Pts',(3.45396108248041,-2.49310820388228,4.46337596028029));
#13749=CARTESIAN_POINT('Ctrl Pts',(3.48843309316639,-2.52409905740531,4.46648992225092));
#13750=CARTESIAN_POINT('Ctrl Pts',(3.52944351212684,-2.56096803782247,4.47019451860319));
#13751=CARTESIAN_POINT('Ctrl Pts',(3.59053745228497,-2.57549754092119,4.47389911495546));
#13752=CARTESIAN_POINT('Ctrl Pts',(3.64375492615303,-2.56103806030718,4.47760371130773));
#13753=CARTESIAN_POINT('Ctrl Pts',(3.69697240002109,-2.54657857969317,4.48130830766));
#13754=CARTESIAN_POINT('Ctrl Pts',(3.74231340759908,-2.50313011536643,4.48501290401227));
#13755=CARTESIAN_POINT('Ctrl Pts',(3.75902737934242,-2.45057710185421,4.48871750036453));
#13756=CARTESIAN_POINT('Ctrl Pts',(3.77574135108577,-2.39802408834199,4.4924220967168));
#13757=CARTESIAN_POINT('Ctrl Pts',(3.76382828699448,-2.33636652564429,4.49612669306907));
#13758=CARTESIAN_POINT('Ctrl Pts',(3.72874026856414,-2.29382234772163,4.49983128942134));
#13759=CARTESIAN_POINT('Ctrl Pts',(3.6936522501338,-2.25127816979896,4.5035358857736));
#13760=CARTESIAN_POINT('Ctrl Pts',(3.63538927736442,-2.22784737665133,4.50724048212587));
#13761=CARTESIAN_POINT('Ctrl Pts',(3.58061573003626,-2.23425320323999,4.51094507847814));
#13762=CARTESIAN_POINT('Ctrl Pts',(3.52584218270809,-2.24065902982864,4.51464967483041));
#13763=CARTESIAN_POINT('Ctrl Pts',(3.47455806082114,-2.27690147615359,4.51835427118267));
#13764=CARTESIAN_POINT('Ctrl Pts',(3.45023383359826,-2.32639398133752,4.52205886753494));
#13765=CARTESIAN_POINT('Ctrl Pts',(3.43909540927391,-2.34905733333477,4.5237552571363));
#13766=CARTESIAN_POINT('Ctrl Pts',(3.4336100971438,-2.37449903703717,4.52545164673766));
#13767=CARTESIAN_POINT('Ctrl Pts',(3.43366207720083,-2.39996197521424,4.52714803633902));
#13768=CARTESIAN_POINT('Origin',(3.6,-2.4,4.7));
#13769=CARTESIAN_POINT('',(3.43341475097665,-2.4001523433056,4.59714803633902));
#13770=CARTESIAN_POINT('',(3.43312356989615,-2.39999932887968,4.57785196366098));
#13771=CARTESIAN_POINT('',(3.4334,-2.4,4.7));
#13772=CARTESIAN_POINT('Ctrl Pts',(3.4331235712606,-2.39999932888299,4.57785196366098));
#13773=CARTESIAN_POINT('Ctrl Pts',(3.43312027533203,-2.34481656196242,4.57414495489509));
#13774=CARTESIAN_POINT('Ctrl Pts',(3.46320503039949,-2.28963688420389,4.57043794612919));
#13775=CARTESIAN_POINT('Ctrl Pts',(3.50958660961886,-2.25973894891049,4.5667309373633));
#13776=CARTESIAN_POINT('Ctrl Pts',(3.55593800505376,-2.22986047032491,4.56302634101103));
#13777=CARTESIAN_POINT('Ctrl Pts',(3.61856500889817,-2.22523083965654,4.55932174465877));
#13778=CARTESIAN_POINT('Ctrl Pts',(3.66880601775922,-2.24796883366633,4.5556171483065));
#13779=CARTESIAN_POINT('Ctrl Pts',(3.71904702662027,-2.27070682767613,4.55191255195423));
#13780=CARTESIAN_POINT('Ctrl Pts',(3.75690204049796,-2.32081244636408,4.54820795560196));
#13781=CARTESIAN_POINT('Ctrl Pts',(3.765046497567,-2.37535456915184,4.54450335924969));
#13782=CARTESIAN_POINT('Ctrl Pts',(3.77319095463605,-2.4298966919396,4.54079876289742));
#13783=CARTESIAN_POINT('Ctrl Pts',(3.75162485489646,-2.48887531882715,4.53709416654515));
#13784=CARTESIAN_POINT('Ctrl Pts',(3.71021804632554,-2.52529854692327,4.53338957019289));
#13785=CARTESIAN_POINT('Ctrl Pts',(3.66881123775463,-2.56172177501939,4.52968497384062));
#13786=CARTESIAN_POINT('Ctrl Pts',(3.60756372035239,-2.57558960432407,4.52598037748835));
#13787=CARTESIAN_POINT('Ctrl Pts',(3.55450576746795,-2.56055534384899,4.52227578113609));
#13788=CARTESIAN_POINT('Ctrl Pts',(3.5014478145835,-2.5455210833739,4.51857118478382));
#13789=CARTESIAN_POINT('Ctrl Pts',(3.45657942621685,-2.50158473311904,4.51486658843155));
#13790=CARTESIAN_POINT('Ctrl Pts',(3.44043487529976,-2.44885401345736,4.51116199207928));
#13791=CARTESIAN_POINT('Ctrl Pts',(3.43562653117309,-2.43314918230523,4.51005864927318));
#13792=CARTESIAN_POINT('Ctrl Pts',(3.43336608251409,-2.41666426269897,4.50895530646708));
#13793=CARTESIAN_POINT('Ctrl Pts',(3.43350143827108,-2.40014312936039,4.50785196366098));
#13794=CARTESIAN_POINT('Ctrl Pts',(3.43366207720083,-2.39996197521424,4.52714803633902));
#13795=CARTESIAN_POINT('Ctrl Pts',(3.43372361182786,-2.43010531274957,4.52915624308993));
#13796=CARTESIAN_POINT('Ctrl Pts',(3.4415451707818,-2.46027840851952,4.53116444984084));
#13797=CARTESIAN_POINT('Ctrl Pts',(3.45693460775185,-2.48590718316162,4.53317265659175));
#13798=CARTESIAN_POINT('Ctrl Pts',(3.48532394168714,-2.53318531575888,4.53687725294402));
#13799=CARTESIAN_POINT('Ctrl Pts',(3.53946694211655,-2.5649990169105,4.54058184929628));
#13800=CARTESIAN_POINT('Ctrl Pts',(3.59458475789197,-2.56678856593634,4.54428644564855));
#13801=CARTESIAN_POINT('Ctrl Pts',(3.64970257366739,-2.56857811496219,4.54799104200082));
#13802=CARTESIAN_POINT('Ctrl Pts',(3.70579520478882,-2.54034351186226,4.55169563835309));
#13803=CARTESIAN_POINT('Ctrl Pts',(3.73719154055164,-2.49500648282243,4.55540023470536));
#13804=CARTESIAN_POINT('Ctrl Pts',(3.76858787631446,-2.4496694537826,4.55910483105763));
#13805=CARTESIAN_POINT('Ctrl Pts',(3.77528791671867,-2.38722999880286,4.56280942740989));
#13806=CARTESIAN_POINT('Ctrl Pts',(3.75422535028399,-2.33626388852243,4.56651402376216));
#13807=CARTESIAN_POINT('Ctrl Pts',(3.73316278384931,-2.28529777824199,4.57021862011443));
#13808=CARTESIAN_POINT('Ctrl Pts',(3.68433761057573,-2.24580501266085,4.5739232164667));
#13809=CARTESIAN_POINT('Ctrl Pts',(3.63009494786823,-2.23585967988047,4.57762781281896));
#13810=CARTESIAN_POINT('Ctrl Pts',(3.57585228516072,-2.22591434710008,4.58133240917123));
#13811=CARTESIAN_POINT('Ctrl Pts',(3.51619213301928,-2.24551644712046,4.5850370055235));
#13812=CARTESIAN_POINT('Ctrl Pts',(3.47841829836813,-2.28569496771878,4.58874160187577));
#13813=CARTESIAN_POINT('Ctrl Pts',(3.4498462907659,-2.31608587207317,4.59154374669685));
#13814=CARTESIAN_POINT('Ctrl Pts',(3.43379623586762,-2.35824928979842,4.59434589151794));
#13815=CARTESIAN_POINT('Ctrl Pts',(3.43341475097665,-2.4001523433056,4.59714803633902));
#13816=CARTESIAN_POINT('Origin',(3.6,-2.4,4.7));
#13817=CARTESIAN_POINT('',(3.43314572405529,-2.39994496470472,4.66714803633902));
#13818=CARTESIAN_POINT('',(3.43350339621029,-2.39985729254273,4.64785196366098));
#13819=CARTESIAN_POINT('',(3.4334,-2.4,4.7));
#13820=CARTESIAN_POINT('Ctrl Pts',(3.43350339621029,-2.39985729254273,4.64785196366098));
#13821=CARTESIAN_POINT('Ctrl Pts',(3.43336796571017,-2.38326341978069,4.64674379602763));
#13822=CARTESIAN_POINT('Ctrl Pts',(3.43564862259693,-2.36670593582693,4.64563562839428));
#13823=CARTESIAN_POINT('Ctrl Pts',(3.44049848254047,-2.3509387164529,4.64452746076093));
#13824=CARTESIAN_POINT('Ctrl Pts',(3.45671152911857,-2.29822901656582,4.64082286440866));
#13825=CARTESIAN_POINT('Ctrl Pts',(3.50163696254783,-2.25435099787568,4.6371182680564));
#13826=CARTESIAN_POINT('Ctrl Pts',(3.55471440347455,-2.23938568444105,4.63341367170413));
#13827=CARTESIAN_POINT('Ctrl Pts',(3.60779184440126,-2.22442037100641,4.62970907535186));
#13828=CARTESIAN_POINT('Ctrl Pts',(3.66902129282543,-2.23836776282728,4.62600447899959));
#13829=CARTESIAN_POINT('Ctrl Pts',(3.71038074448169,-2.27484475695027,4.62229988264732));
#13830=CARTESIAN_POINT('Ctrl Pts',(3.75174019613796,-2.31132175107326,4.61859528629505));
#13831=CARTESIAN_POINT('Ctrl Pts',(3.77322965102632,-2.37032834749837,4.61489068994278));
#13832=CARTESIAN_POINT('Ctrl Pts',(3.76501433826252,-2.42485984278043,4.61118609359052));
#13833=CARTESIAN_POINT('Ctrl Pts',(3.75679902549871,-2.47939133806249,4.60748149723825));
#13834=CARTESIAN_POINT('Ctrl Pts',(3.71887894508274,-2.52944773220152,4.60377690088598));
#13835=CARTESIAN_POINT('Ctrl Pts',(3.66860843684067,-2.55212043258282,4.60007230453372));
#13836=CARTESIAN_POINT('Ctrl Pts',(3.6183379285986,-2.57479313296412,4.59636770818145));
#13837=CARTESIAN_POINT('Ctrl Pts',(3.55571699253044,-2.5700821395877,4.59266311182918));
#13838=CARTESIAN_POINT('Ctrl Pts',(3.50940445510819,-2.54014346528121,4.58895851547691));
#13839=CARTESIAN_POINT('Ctrl Pts',(3.46312207616628,-2.51022428688169,4.58525633153827));
#13840=CARTESIAN_POINT('Ctrl Pts',(3.43312686289939,-2.45511027311999,4.58155414759963));
#13841=CARTESIAN_POINT('Ctrl Pts',(3.4331235712606,-2.39999932888299,4.57785196366098));
#13842=CARTESIAN_POINT('Ctrl Pts',(3.43341475097665,-2.4001523433056,4.59714803633902));
#13843=CARTESIAN_POINT('Ctrl Pts',(3.43329189093694,-2.41364753260286,4.5980504878702));
#13844=CARTESIAN_POINT('Ctrl Pts',(3.43479419036014,-2.42711571666781,4.59895293940139));
#13845=CARTESIAN_POINT('Ctrl Pts',(3.43802675920227,-2.44015494791281,4.59985539093257));
#13846=CARTESIAN_POINT('Ctrl Pts',(3.45129657184842,-2.49368146633226,4.60355998728484));
#13847=CARTESIAN_POINT('Ctrl Pts',(3.49372371430156,-2.53997956199491,4.60726458363711));
#13848=CARTESIAN_POINT('Ctrl Pts',(3.54589116423991,-2.55786064889342,4.61096917998938));
#13849=CARTESIAN_POINT('Ctrl Pts',(3.59805861417826,-2.57574173579194,4.61467377634165));
#13850=CARTESIAN_POINT('Ctrl Pts',(3.65996637160182,-2.56520581392632,4.61837837269391));
#13851=CARTESIAN_POINT('Ctrl Pts',(3.70328200028476,-2.53107470768073,4.62208296904618));
#13852=CARTESIAN_POINT('Ctrl Pts',(3.74659762896771,-2.49694360143515,4.62578756539845));
#13853=CARTESIAN_POINT('Ctrl Pts',(3.77132112891003,-2.43921731080961,4.62949216175072));
#13854=CARTESIAN_POINT('Ctrl Pts',(3.76613765017139,-2.3843146000394,4.63319675810299));
#13855=CARTESIAN_POINT('Ctrl Pts',(3.76095417143275,-2.32941188926919,4.63690135445526));
#13856=CARTESIAN_POINT('Ctrl Pts',(3.72586371401314,-2.27733275835431,4.64060595080752));
#13857=CARTESIAN_POINT('Ctrl Pts',(3.67692562472706,-2.25191151686662,4.64431054715979));
#13858=CARTESIAN_POINT('Ctrl Pts',(3.62798753544098,-2.22649027537894,4.64801514351206));
#13859=CARTESIAN_POINT('Ctrl Pts',(3.56520181428843,-2.22772692331845,4.65171973986433));
#13860=CARTESIAN_POINT('Ctrl Pts',(3.51730270257413,-2.25505550174341,4.6554243362166));
#13861=CARTESIAN_POINT('Ctrl Pts',(3.46940359085983,-2.28238408016837,4.65912893256887));
#13862=CARTESIAN_POINT('Ctrl Pts',(3.43639108858378,-2.33580458907878,4.66283352892113));
#13863=CARTESIAN_POINT('Ctrl Pts',(3.43337355460624,-2.39086882965689,4.6665381252734));
#13864=CARTESIAN_POINT('Ctrl Pts',(3.43320795605525,-2.39389068741188,4.66674142896194));
#13865=CARTESIAN_POINT('Ctrl Pts',(3.43313269272996,-2.39691749555954,4.66694473265048));
#13866=CARTESIAN_POINT('Ctrl Pts',(3.43314572405529,-2.39994496470472,4.66714803633902));
#13867=CARTESIAN_POINT('Origin',(3.6,-2.4,4.7));
#13868=CARTESIAN_POINT('',(3.43357723227316,-2.39988235337877,4.73714803633902));
#13869=CARTESIAN_POINT('',(3.43362781745768,-2.40008425136911,4.71785196366098));
#13870=CARTESIAN_POINT('',(3.4334,-2.4,4.7));
#13871=CARTESIAN_POINT('Ctrl Pts',(3.43362781745768,-2.40008425136911,4.71785196366098));
#13872=CARTESIAN_POINT('Ctrl Pts',(3.43377992278221,-2.36687021363152,4.7156380408079));
#13873=CARTESIAN_POINT('Ctrl Pts',(3.44340627006936,-2.33357497132763,4.71342411795483));
#13874=CARTESIAN_POINT('Ctrl Pts',(3.46191047910031,-2.30630353350919,4.71121019510175));
#13875=CARTESIAN_POINT('Ctrl Pts',(3.49287390006255,-2.260669753216,4.70750559874949));
#13876=CARTESIAN_POINT('Ctrl Pts',(3.54869526474406,-2.23190257855334,4.70380100239722));
#13877=CARTESIAN_POINT('Ctrl Pts',(3.60382760906969,-2.23316747012655,4.70009640604495));
#13878=CARTESIAN_POINT('Ctrl Pts',(3.65895995339532,-2.23443236169976,4.69639180969269));
#13879=CARTESIAN_POINT('Ctrl Pts',(3.71340327736507,-2.26572931950883,4.69268721334041));
#13880=CARTESIAN_POINT('Ctrl Pts',(3.74224128504954,-2.31273511334664,4.68898261698815));
#13881=CARTESIAN_POINT('Ctrl Pts',(3.77107929273401,-2.35974090718445,4.68527802063588));
#13882=CARTESIAN_POINT('Ctrl Pts',(3.7743119841332,-2.42245553705099,4.68157342428361));
#13883=CARTESIAN_POINT('Ctrl Pts',(3.75045989969766,-2.47217729697168,4.67786882793135));
#13884=CARTESIAN_POINT('Ctrl Pts',(3.72660781526212,-2.52189905689238,4.67416423157908));
#13885=CARTESIAN_POINT('Ctrl Pts',(3.67567095499184,-2.55862794686723,4.67045963522681));
#13886=CARTESIAN_POINT('Ctrl Pts',(3.62096086182118,-2.56555478213231,4.66675503887454));
#13887=CARTESIAN_POINT('Ctrl Pts',(3.56625076865053,-2.57248161739739,4.66305044252227));
#13888=CARTESIAN_POINT('Ctrl Pts',(3.50776744257951,-2.54960639795269,4.65934584617));
#13889=CARTESIAN_POINT('Ctrl Pts',(3.47227610940747,-2.50739809768834,4.65564124981773));
#13890=CARTESIAN_POINT('Ctrl Pts',(3.44740141107113,-2.47781569988784,4.65304482109882));
#13891=CARTESIAN_POINT('Ctrl Pts',(3.43382070888877,-2.43873661594181,4.6504483923799));
#13892=CARTESIAN_POINT('Ctrl Pts',(3.43350339621029,-2.39985729254273,4.64785196366098));
#13893=CARTESIAN_POINT('Ctrl Pts',(3.43314572405529,-2.39994496470472,4.66714803633902));
#13894=CARTESIAN_POINT('Ctrl Pts',(3.43337014931821,-2.45208398679426,4.67064932900275));
#13895=CARTESIAN_POINT('Ctrl Pts',(3.45978247638053,-2.50441905856693,4.67415062166648));
#13896=CARTESIAN_POINT('Ctrl Pts',(3.50195948177967,-2.53504002133992,4.67765191433021));
#13897=CARTESIAN_POINT('Ctrl Pts',(3.54658550860969,-2.56743900019905,4.68135651068247));
#13898=CARTESIAN_POINT('Ctrl Pts',(3.60886012794877,-2.57552898567153,4.68506110703474));
#13899=CARTESIAN_POINT('Ctrl Pts',(3.66028300713527,-2.55560755003253,4.68876570338701));
#13900=CARTESIAN_POINT('Ctrl Pts',(3.71170588632177,-2.53568611439352,4.69247029973927));
#13901=CARTESIAN_POINT('Ctrl Pts',(3.7522770253557,-2.48775325764304,4.69617489609154));
#13902=CARTESIAN_POINT('Ctrl Pts',(3.76342881240416,-2.43374572347072,4.69987949244381));
#13903=CARTESIAN_POINT('Ctrl Pts',(3.77458059945262,-2.3797381892984,4.70358408879608));
#13904=CARTESIAN_POINT('Ctrl Pts',(3.75631303451563,-2.31965597770425,4.70728868514835));
#13905=CARTESIAN_POINT('Ctrl Pts',(3.71698637227073,-2.28099605351363,4.71099328150061));
#13906=CARTESIAN_POINT('Ctrl Pts',(3.67765971002583,-2.24233612932302,4.71469787785288));
#13907=CARTESIAN_POINT('Ctrl Pts',(3.61727395047302,-2.22509849253594,4.71840247420515));
#13908=CARTESIAN_POINT('Ctrl Pts',(3.5634649788822,-2.23717204537206,4.72210707055742));
#13909=CARTESIAN_POINT('Ctrl Pts',(3.50965600729138,-2.24924559820818,4.72581166690969));
#13910=CARTESIAN_POINT('Ctrl Pts',(3.46242382366254,-2.29063034066749,4.72951626326196));
#13911=CARTESIAN_POINT('Ctrl Pts',(3.44338450465812,-2.34238631069604,4.73322085961423));
#13912=CARTESIAN_POINT('Ctrl Pts',(3.43665675680651,-2.36067483856233,4.73452991852249));
#13913=CARTESIAN_POINT('Ctrl Pts',(3.43344927751834,-2.38025835744364,4.73583897743076));
#13914=CARTESIAN_POINT('Ctrl Pts',(3.43357723227316,-2.39988235337877,4.73714803633902));
#13915=CARTESIAN_POINT('Origin',(3.6,-2.4,4.7));
#13916=CARTESIAN_POINT('',(3.43357088161517,-2.40012064492246,4.80714803633902));
#13917=CARTESIAN_POINT('',(3.43319592655187,-2.40009747379871,4.78785196366098));
#13918=CARTESIAN_POINT('',(3.4334,-2.4,4.7));
#13919=CARTESIAN_POINT('Ctrl Pts',(3.43319592655187,-2.40009747379871,4.78785196366098));
#13920=CARTESIAN_POINT('Ctrl Pts',(3.43353982295269,-2.35062359307345,4.78453228558818));
#13921=CARTESIAN_POINT('Ctrl Pts',(3.45695304474081,-2.30086703036466,4.78121260751538));
#13922=CARTESIAN_POINT('Ctrl Pts',(3.49547520498793,-2.2699142173685,4.77789292944258));
#13923=CARTESIAN_POINT('Ctrl Pts',(3.53846402836278,-2.23537241072238,4.77418833309031));
#13924=CARTESIAN_POINT('Ctrl Pts',(3.6002686999986,-2.22424776884202,4.77048373673804));
#13925=CARTESIAN_POINT('Ctrl Pts',(3.65260396146494,-2.24163154716497,4.76677914038577));
#13926=CARTESIAN_POINT('Ctrl Pts',(3.70493922293128,-2.25901532548792,4.76307454403351));
#13927=CARTESIAN_POINT('Ctrl Pts',(3.74780507422814,-2.30490752401418,4.75936994768124));
#13928=CARTESIAN_POINT('Ctrl Pts',(3.7615837154436,-2.35830531786175,4.75566535132897));
#13929=CARTESIAN_POINT('Ctrl Pts',(3.77536235665906,-2.41170311170932,4.75196075497671));
#13930=CARTESIAN_POINT('Ctrl Pts',(3.76005378779311,-2.4726065008782,4.74825615862444));
#13931=CARTESIAN_POINT('Ctrl Pts',(3.72266406219276,-2.51314270396953,4.74455156227217));
#13932=CARTESIAN_POINT('Ctrl Pts',(3.68527433659241,-2.55367890706087,4.7408469659199));
#13933=CARTESIAN_POINT('Ctrl Pts',(3.62580345425764,-2.57384792407467,4.73714236956763));
#13934=CARTESIAN_POINT('Ctrl Pts',(3.57146860171181,-2.56441929000846,4.73343777321536));
#13935=CARTESIAN_POINT('Ctrl Pts',(3.51713374916598,-2.55499065594226,4.7297331768631));
#13936=CARTESIAN_POINT('Ctrl Pts',(3.46793492640908,-2.51596437079605,4.72602858051083));
#13937=CARTESIAN_POINT('Ctrl Pts',(3.4463882536521,-2.46520103526108,4.72232398415856));
#13938=CARTESIAN_POINT('Ctrl Pts',(3.43771819866623,-2.44477463739825,4.72083331065937));
#13939=CARTESIAN_POINT('Ctrl Pts',(3.43352540224658,-2.42244785170318,4.71934263716017));
#13940=CARTESIAN_POINT('Ctrl Pts',(3.43362781745768,-2.40008425136911,4.71785196366098));
#13941=CARTESIAN_POINT('Ctrl Pts',(3.43357723227316,-2.39988235337877,4.73714803633902));
#13942=CARTESIAN_POINT('Ctrl Pts',(3.43381138552965,-2.4357936609347,4.73954357378302));
#13943=CARTESIAN_POINT('Ctrl Pts',(3.44521519749436,-2.4718405175289,4.74193911122702));
#13944=CARTESIAN_POINT('Ctrl Pts',(3.46665596946098,-2.50033503922361,4.74433464867103));
#13945=CARTESIAN_POINT('Ctrl Pts',(3.49981320764826,-2.54440060012484,4.74803924502329));
#13946=CARTESIAN_POINT('Ctrl Pts',(3.55697413840284,-2.57040452432951,4.75174384137556));
#13947=CARTESIAN_POINT('Ctrl Pts',(3.61197873764036,-2.56644596847307,4.75544843772783));
#13948=CARTESIAN_POINT('Ctrl Pts',(3.66698333687788,-2.56248741261664,4.7591530340801));
#13949=CARTESIAN_POINT('Ctrl Pts',(3.71983160459833,-2.52856637669909,4.76285763043237));
#13950=CARTESIAN_POINT('Ctrl Pts',(3.7463372314094,-2.48020701515346,4.76656222678464));
#13951=CARTESIAN_POINT('Ctrl Pts',(3.77284285822047,-2.43184765360783,4.7702668231369));
#13952=CARTESIAN_POINT('Ctrl Pts',(3.77300584412214,-2.36904996643411,4.77397141948917));
#13953=CARTESIAN_POINT('Ctrl Pts',(3.74675159769234,-2.32055367125447,4.77767601584144));
#13954=CARTESIAN_POINT('Ctrl Pts',(3.72049735126253,-2.27205737607482,4.78138061219371));
#13955=CARTESIAN_POINT('Ctrl Pts',(3.66782587250124,-2.23786247288924,4.78508520854598));
#13956=CARTESIAN_POINT('Ctrl Pts',(3.61284256233116,-2.23361845303891,4.78878980489824));
#13957=CARTESIAN_POINT('Ctrl Pts',(3.55785925216109,-2.22937443318857,4.79249440125051));
#13958=CARTESIAN_POINT('Ctrl Pts',(3.50056411058224,-2.25508129667347,4.79619899760278));
#13959=CARTESIAN_POINT('Ctrl Pts',(3.46717858402372,-2.29897415165191,4.79990359395505));
#13960=CARTESIAN_POINT('Ctrl Pts',(3.44541647189655,-2.32758538921762,4.80231840808304));
#13961=CARTESIAN_POINT('Ctrl Pts',(3.43381352935432,-2.36392383491678,4.80473322221103));
#13962=CARTESIAN_POINT('Ctrl Pts',(3.43357088161517,-2.40012064492246,4.80714803633902));
#13963=CARTESIAN_POINT('Origin',(3.6,-2.4,4.7));
#13964=CARTESIAN_POINT('',(3.43314189260959,-2.4000500574177,4.87714803633902));
#13965=CARTESIAN_POINT('',(3.43333250832843,-2.39985412494998,4.85785196366098));
#13966=CARTESIAN_POINT('',(3.4334,-2.4,4.7));
#13967=CARTESIAN_POINT('Ctrl Pts',(3.43333250832843,-2.39985412494998,4.85785196366098));
#13968=CARTESIAN_POINT('Ctrl Pts',(3.43323384369475,-2.3890884237173,4.85713112672072));
#13969=CARTESIAN_POINT('Ctrl Pts',(3.43418764919828,-2.37834013090661,4.85641028978047));
#13970=CARTESIAN_POINT('Ctrl Pts',(3.4362574396422,-2.36781122023692,4.85568945284021));
#13971=CARTESIAN_POINT('Ctrl Pts',(3.44689471098651,-2.31370000328629,4.85198485648794));
#13972=CARTESIAN_POINT('Ctrl Pts',(3.48700781310569,-2.26538319325753,4.84828026013567));
#13973=CARTESIAN_POINT('Ctrl Pts',(3.53823875735816,-2.24497325223528,4.8445756637834));
#13974=CARTESIAN_POINT('Ctrl Pts',(3.58946970161063,-2.22456331121304,4.84087106743114));
#13975=CARTESIAN_POINT('Ctrl Pts',(3.65181848799641,-2.23206023919731,4.83716647107887));
#13976=CARTESIAN_POINT('Ctrl Pts',(3.69675084088435,-2.26403302458561,4.8334618747266));
#13977=CARTESIAN_POINT('Ctrl Pts',(3.74168319377229,-2.2960058099739,4.82975727837434));
#13978=CARTESIAN_POINT('Ctrl Pts',(3.76919911316239,-2.35245445276622,4.82605268202207));
#13979=CARTESIAN_POINT('Ctrl Pts',(3.76670578251992,-2.40754491150309,4.8223480856698));
#13980=CARTESIAN_POINT('Ctrl Pts',(3.76421245187744,-2.46263537023996,4.81864348931753));
#13981=CARTESIAN_POINT('Ctrl Pts',(3.73170987120238,-2.51636764492139,4.81493889296526));
#13982=CARTESIAN_POINT('Ctrl Pts',(3.68407303084285,-2.54415085535669,4.81123429661299));
#13983=CARTESIAN_POINT('Ctrl Pts',(3.63643619048332,-2.57193406579199,4.80752970026073));
#13984=CARTESIAN_POINT('Ctrl Pts',(3.57366509043931,-2.57376821198116,4.80382510390846));
#13985=CARTESIAN_POINT('Ctrl Pts',(3.52448728058231,-2.54881388652042,4.80012050755619));
#13986=CARTESIAN_POINT('Ctrl Pts',(3.47530947072531,-2.52385956105968,4.79641591120392));
#13987=CARTESIAN_POINT('Ctrl Pts',(3.43972495105532,-2.47211676394902,4.79271131485165));
#13988=CARTESIAN_POINT('Ctrl Pts',(3.43401917877726,-2.41726587968776,4.78900671849938));
#13989=CARTESIAN_POINT('Ctrl Pts',(3.43342633252912,-2.41156671411356,4.78862180021992));
#13990=CARTESIAN_POINT('Ctrl Pts',(3.43315605159773,-2.40583399421718,4.78823688194045));
#13991=CARTESIAN_POINT('Ctrl Pts',(3.43319592655187,-2.40009747379871,4.78785196366098));
#13992=CARTESIAN_POINT('Ctrl Pts',(3.43357088161517,-2.40012064492246,4.80714803633902));
#13993=CARTESIAN_POINT('Ctrl Pts',(3.43344128044335,-2.4194538108087,4.8084378185633));
#13994=CARTESIAN_POINT('Ctrl Pts',(3.43655249964156,-2.4387465714195,4.80972760078758));
#13995=CARTESIAN_POINT('Ctrl Pts',(3.44308755405667,-2.45679995496896,4.81101738301185));
#13996=CARTESIAN_POINT('Ctrl Pts',(3.46185796218633,-2.50865405683559,4.81472197936412));
#13997=CARTESIAN_POINT('Ctrl Pts',(3.50887468998386,-2.55028341409687,4.81842657571639));
#13998=CARTESIAN_POINT('Ctrl Pts',(3.56262026536972,-2.56263611534763,4.82213117206866));
#13999=CARTESIAN_POINT('Ctrl Pts',(3.61636584075558,-2.5749888165984,4.82583576842092));
#14000=CARTESIAN_POINT('Ctrl Pts',(3.67684026372979,-2.55806486183865,4.82954036477319));
#14001=CARTESIAN_POINT('Ctrl Pts',(3.71636707170489,-2.51960959492959,4.83324496112546));
#14002=CARTESIAN_POINT('Ctrl Pts',(3.75589387967999,-2.48115432802054,4.83694955747773));
#14003=CARTESIAN_POINT('Ctrl Pts',(3.77447307265599,-2.42116774896216,4.84065415383));
#14004=CARTESIAN_POINT('Ctrl Pts',(3.76360177761623,-2.36710305580748,4.84435875018227));
#14005=CARTESIAN_POINT('Ctrl Pts',(3.75273048257646,-2.3130383626528,4.84806334653453));
#14006=CARTESIAN_POINT('Ctrl Pts',(3.71240869952093,-2.26489555540181,4.8517679428868));
#14007=CARTESIAN_POINT('Ctrl Pts',(3.66108992110507,-2.24470746278141,4.85547253923907));
#14008=CARTESIAN_POINT('Ctrl Pts',(3.60977114268922,-2.224519370161,4.85917713559134));
#14009=CARTESIAN_POINT('Ctrl Pts',(3.54745536891304,-2.23228599217118,4.86288173194361));
#14010=CARTESIAN_POINT('Ctrl Pts',(3.50266176699964,-2.26445289020885,4.86658632829587));
#14011=CARTESIAN_POINT('Ctrl Pts',(3.4600933015382,-2.29502188733407,4.87010689764359));
#14012=CARTESIAN_POINT('Ctrl Pts',(3.43334940736011,-2.34762718854044,4.87362746699131));
#14013=CARTESIAN_POINT('Ctrl Pts',(3.43314189260959,-2.4000500574177,4.87714803633902));
#14014=CARTESIAN_POINT('Origin',(3.6,-2.4,4.7));
#14015=CARTESIAN_POINT('',(3.43342339329134,-2.39984780956037,4.94714803633902));
#14016=CARTESIAN_POINT('',(3.43366987537036,-2.39999366746476,4.92785196366098));
#14017=CARTESIAN_POINT('',(3.4334,-2.4,4.7));
#14018=CARTESIAN_POINT('Ctrl Pts',(3.43366987537036,-2.39999366746476,4.92785196366098));
#14019=CARTESIAN_POINT('Ctrl Pts',(3.43366057869757,-2.37257318362641,4.926025371501));
#14020=CARTESIAN_POINT('Ctrl Pts',(3.44006468998231,-2.34515678783965,4.92419877934102));
#14021=CARTESIAN_POINT('Ctrl Pts',(3.45290605548974,-2.32118937188857,4.92237218718104));
#14022=CARTESIAN_POINT('Ctrl Pts',(3.47895022498703,-2.27257994300186,4.91866759082877));
#14023=CARTESIAN_POINT('Ctrl Pts',(3.53147325377826,-2.23815747156893,4.9149629944765));
#14024=CARTESIAN_POINT('Ctrl Pts',(3.58643767991325,-2.23367559683213,4.91125839812423));
#14025=CARTESIAN_POINT('Ctrl Pts',(3.64140210604824,-2.22919372209532,4.90755380177196));
#14026=CARTESIAN_POINT('Ctrl Pts',(3.69880792952698,-2.25465244405464,4.9038492054197));
#14027=CARTESIAN_POINT('Ctrl Pts',(3.7323830497203,-2.29840043424344,4.90014460906743));
#14028=CARTESIAN_POINT('Ctrl Pts',(3.76595816991362,-2.34214842443224,4.89644001271516));
#14029=CARTESIAN_POINT('Ctrl Pts',(3.77570258682152,-2.40418568285053,4.89273541636289));
#14030=CARTESIAN_POINT('Ctrl Pts',(3.75715671279198,-2.45612050640859,4.88903082001062));
#14031=CARTESIAN_POINT('Ctrl Pts',(3.73861083876244,-2.50805532996664,4.88532622365835));
#14032=CARTESIAN_POINT('Ctrl Pts',(3.69177467379546,-2.54988771866446,4.88162162730609));
#14033=CARTESIAN_POINT('Ctrl Pts',(3.63808305436706,-2.56247284260842,4.87791703095382));
#14034=CARTESIAN_POINT('Ctrl Pts',(3.58439143493865,-2.57505796655237,4.87421243460155));
#14035=CARTESIAN_POINT('Ctrl Pts',(3.52384436104883,-2.55839582574246,4.87050783824928));
#14036=CARTESIAN_POINT('Ctrl Pts',(3.48415154438863,-2.52011194340126,4.86680324189701));
#14037=CARTESIAN_POINT('Ctrl Pts',(3.45218211937245,-2.4892773035642,4.863819482485));
#14038=CARTESIAN_POINT('Ctrl Pts',(3.4337409107187,-2.4444165781012,4.86083572307299));
#14039=CARTESIAN_POINT('Ctrl Pts',(3.43333250832843,-2.39985412494998,4.85785196366098));
#14040=CARTESIAN_POINT('Ctrl Pts',(3.43314189260959,-2.4000500574177,4.87714803633902));
#14041=CARTESIAN_POINT('Ctrl Pts',(3.43313104541013,-2.4027903026953,4.87733206334358));
#14042=CARTESIAN_POINT('Ctrl Pts',(3.43319270505025,-2.40553004950279,4.87751609034813));
#14043=CARTESIAN_POINT('Ctrl Pts',(3.43332840145004,-2.40826612443654,4.87770011735268));
#14044=CARTESIAN_POINT('Ctrl Pts',(3.43606006786446,-2.46334528656136,4.88140471370495));
#14045=CARTESIAN_POINT('Ctrl Pts',(3.46879483074392,-2.51693643674581,4.88510931005721));
#14046=CARTESIAN_POINT('Ctrl Pts',(3.51655144023777,-2.54451328122398,4.88881390640948));
#14047=CARTESIAN_POINT('Ctrl Pts',(3.56430804973163,-2.57209012570216,4.89251850276175));
#14048=CARTESIAN_POINT('Ctrl Pts',(3.62708650583988,-2.57365266447405,4.89622309911402));
#14049=CARTESIAN_POINT('Ctrl Pts',(3.67615589214678,-2.54848579281353,4.89992769546629));
#14050=CARTESIAN_POINT('Ctrl Pts',(3.72522527845368,-2.52331892115301,4.90363229181856));
#14051=CARTESIAN_POINT('Ctrl Pts',(3.76058559495924,-2.47142263906009,4.90733688817082));
#14052=CARTESIAN_POINT('Ctrl Pts',(3.76605399230753,-2.41654757430046,4.91104148452309));
#14053=CARTESIAN_POINT('Ctrl Pts',(3.77152238965583,-2.36167250954082,4.91474608087536));
#14054=CARTESIAN_POINT('Ctrl Pts',(3.74709886784687,-2.30381866211447,4.91845067722763));
#14055=CARTESIAN_POINT('Ctrl Pts',(3.70396099012833,-2.26946317336186,4.9221552735799));
#14056=CARTESIAN_POINT('Ctrl Pts',(3.6608231124098,-2.23510768460924,4.92585986993216));
#14057=CARTESIAN_POINT('Ctrl Pts',(3.5989708787817,-2.22425055453036,4.92956446628443));
#14058=CARTESIAN_POINT('Ctrl Pts',(3.54671131468788,-2.24186061024559,4.9332690626367));
#14059=CARTESIAN_POINT('Ctrl Pts',(3.49445175059407,-2.25947066596082,4.93697365898896));
#14060=CARTESIAN_POINT('Ctrl Pts',(3.45178485603454,-2.30554790747016,4.94067825534124));
#14061=CARTESIAN_POINT('Ctrl Pts',(3.43823737724635,-2.35900482396987,4.94438285169351));
#14062=CARTESIAN_POINT('Ctrl Pts',(3.43486667440692,-2.37230526038685,4.94530457990868));
#14063=CARTESIAN_POINT('Ctrl Pts',(3.43329860172231,-2.38606253373953,4.94622630812385));
#14064=CARTESIAN_POINT('Ctrl Pts',(3.43342339329134,-2.39984780956037,4.94714803633902));
#14065=CARTESIAN_POINT('Origin',(3.6,-2.4,4.7));
#14066=CARTESIAN_POINT('',(3.43365998837939,-2.40004261214837,5.01714803633902));
#14067=CARTESIAN_POINT('',(3.4333557533513,-2.40014916294441,4.99785196366098));
#14068=CARTESIAN_POINT('',(3.4334,-2.4,4.7));
#14069=CARTESIAN_POINT('Ctrl Pts',(3.4333557533513,-2.40014916294441,4.99785196366098));
#14070=CARTESIAN_POINT('Ctrl Pts',(3.43376006878861,-2.35633883086337,4.99491961628128));
#14071=CARTESIAN_POINT('Ctrl Pts',(3.45150379646176,-2.31223873171809,4.99198726890157));
#14072=CARTESIAN_POINT('Ctrl Pts',(3.48249984549986,-2.28150334481789,4.98905492152186));
#14073=CARTESIAN_POINT('Ctrl Pts',(3.5216588656746,-2.24267363351424,4.98535032516959));
#14074=CARTESIAN_POINT('Ctrl Pts',(3.58196947066853,-2.22517489033693,4.98164572881732));
#14075=CARTESIAN_POINT('Ctrl Pts',(3.63583017024712,-2.23701551447795,4.97794113246505));
#14076=CARTESIAN_POINT('Ctrl Pts',(3.68969086982571,-2.24885613861896,4.97423653611278));
#14077=CARTESIAN_POINT('Ctrl Pts',(3.73710166398897,-2.29003613007831,4.97053193976052));
#14078=CARTESIAN_POINT('Ctrl Pts',(3.75636473388799,-2.34170923218213,4.96682734340825));
#14079=CARTESIAN_POINT('Ctrl Pts',(3.775627803787,-2.39338233428594,4.96312274705599));
#14080=CARTESIAN_POINT('Ctrl Pts',(3.76674314942177,-2.45554854703422,4.95941815070372));
#14081=CARTESIAN_POINT('Ctrl Pts',(3.73377688327324,-2.49975715069431,4.95571355435145));
#14082=CARTESIAN_POINT('Ctrl Pts',(3.7008106171247,-2.54396575435439,4.95200895799918));
#14083=CARTESIAN_POINT('Ctrl Pts',(3.64376273919286,-2.57021674892629,4.94830436164691));
#14084=CARTESIAN_POINT('Ctrl Pts',(3.58874153428106,-2.56649621787192,4.94459976529464));
#14085=CARTESIAN_POINT('Ctrl Pts',(3.53372032936927,-2.56277568681755,4.94089516894238));
#14086=CARTESIAN_POINT('Ctrl Pts',(3.48072579747752,-2.52908363013692,4.93719057259011));
#14087=CARTESIAN_POINT('Ctrl Pts',(3.45401118663332,-2.48083940862635,4.93348597623784));
#14088=CARTESIAN_POINT('Ctrl Pts',(3.4404685098097,-2.45638253353524,4.93160797204555));
#14089=CARTESIAN_POINT('Ctrl Pts',(3.43367943371122,-2.42818593979086,4.92972996785327));
#14090=CARTESIAN_POINT('Ctrl Pts',(3.43366987537036,-2.39999366746476,4.92785196366098));
#14091=CARTESIAN_POINT('Ctrl Pts',(3.43342339329134,-2.39984780956037,4.94714803633902));
#14092=CARTESIAN_POINT('Ctrl Pts',(3.43380016214308,-2.44146810957007,4.94993090447612));
#14093=CARTESIAN_POINT('Ctrl Pts',(3.44960819947038,-2.48334366548894,4.95271377261321));
#14094=CARTESIAN_POINT('Ctrl Pts',(3.47782660292827,-2.51367238728015,4.95549664075031));
#14095=CARTESIAN_POINT('Ctrl Pts',(3.51539137041525,-2.55404644260063,4.95920123710258));
#14096=CARTESIAN_POINT('Ctrl Pts',(3.57494896840608,-2.57395796175148,4.96290583345484));
#14097=CARTESIAN_POINT('Ctrl Pts',(3.62924252448225,-2.56429432528282,4.96661042980711));
#14098=CARTESIAN_POINT('Ctrl Pts',(3.68353608055842,-2.55463068881416,4.97031502615938));
#14099=CARTESIAN_POINT('Ctrl Pts',(3.73256559471993,-2.51539189672599,4.97401962251165));
#14100=CARTESIAN_POINT('Ctrl Pts',(3.75389243176138,-2.46453580432507,4.97772421886392));
#14101=CARTESIAN_POINT('Ctrl Pts',(3.77521926880282,-2.41367971192415,4.98142881521619));
#14102=CARTESIAN_POINT('Ctrl Pts',(3.7688434287242,-2.35120631921049,4.98513341156845));
#14103=CARTESIAN_POINT('Ctrl Pts',(3.73768285095733,-2.30570692939164,4.98883800792072));
#14104=CARTESIAN_POINT('Ctrl Pts',(3.70652227319045,-2.26020753957279,4.99254260427299));
#14105=CARTESIAN_POINT('Ctrl Pts',(3.65057695773533,-2.23168215264876,4.99624720062526));
#14106=CARTESIAN_POINT('Ctrl Pts',(3.59545059530862,-2.23318557212546,4.99995179697752));
#14107=CARTESIAN_POINT('Ctrl Pts',(3.5403242328819,-2.23468899160217,5.00365639332979));
#14108=CARTESIAN_POINT('Ctrl Pts',(3.48601682348359,-2.2662212174796,5.00736098968206));
#14109=CARTESIAN_POINT('Ctrl Pts',(3.4573824612349,-2.31335135092863,5.01106558603433));
#14110=CARTESIAN_POINT('Ctrl Pts',(3.44171120056098,-2.3391451367466,5.01309306946923));
#14111=CARTESIAN_POINT('Ctrl Pts',(3.43372965513495,-2.36961088327844,5.01512055290413));
#14112=CARTESIAN_POINT('Ctrl Pts',(3.43365998837939,-2.40004261214837,5.01714803633902));
#14113=CARTESIAN_POINT('Origin',(3.6,-2.4,4.7));
#14114=CARTESIAN_POINT('',(3.43326718206005,-2.40013003210005,5.08714803633902));
#14115=CARTESIAN_POINT('',(3.43317939237559,-2.39991359865598,5.06785196366098));
#14116=CARTESIAN_POINT('',(3.4334,-2.4,4.7));
#14117=CARTESIAN_POINT('Ctrl Pts',(3.43317939237559,-2.39991359865598,5.06785196366098));
#14118=CARTESIAN_POINT('Ctrl Pts',(3.43314802801357,-2.39494457971841,5.06751845741381));
#14119=CARTESIAN_POINT('Ctrl Pts',(3.43335080279482,-2.38997815623028,5.06718495116665));
#14120=CARTESIAN_POINT('Ctrl Pts',(3.43379605546717,-2.38503356765244,5.06685144491949));
#14121=CARTESIAN_POINT('Ctrl Pts',(3.43874193411214,-2.33010894490636,5.06314684856722));
#14122=CARTESIAN_POINT('Ctrl Pts',(3.47360673801625,-2.27787849376484,5.05944225221495));
#14123=CARTESIAN_POINT('Ctrl Pts',(3.52243437581894,-2.25224575672994,5.05573765586269));
#14124=CARTESIAN_POINT('Ctrl Pts',(3.57126201362163,-2.22661301969504,5.05203305951042));
#14125=CARTESIAN_POINT('Ctrl Pts',(3.63405248532289,-2.22757799676674,5.04832846315815));
#14126=CARTESIAN_POINT('Ctrl Pts',(3.68206938357278,-2.25469907052132,5.04462386680588));
#14127=CARTESIAN_POINT('Ctrl Pts',(3.73008628182266,-2.28182014427589,5.04091927045361));
#14128=CARTESIAN_POINT('Ctrl Pts',(3.76332960662116,-2.33509731471334,5.03721467410135));
#14129=CARTESIAN_POINT('Ctrl Pts',(3.7665853578407,-2.39014797778335,5.03351007774908));
#14130=CARTESIAN_POINT('Ctrl Pts',(3.76984110906023,-2.44519864085336,5.02980548139681));
#14131=CARTESIAN_POINT('Ctrl Pts',(3.7431092867008,-2.50202279655593,5.02610088504454));
#14132=CARTESIAN_POINT('Ctrl Pts',(3.69862386285843,-2.53461455026518,5.02239628869228));
#14133=CARTESIAN_POINT('Ctrl Pts',(3.65413843901607,-2.56720630397444,5.01869169234001));
#14134=CARTESIAN_POINT('Ctrl Pts',(3.59189941369078,-2.57556565569037,5.01498709598774));
#14135=CARTESIAN_POINT('Ctrl Pts',(3.54039082873623,-2.55586689947754,5.01128249963547));
#14136=CARTESIAN_POINT('Ctrl Pts',(3.48888224378167,-2.53616814326471,5.0075779032832));
#14137=CARTESIAN_POINT('Ctrl Pts',(3.44810409919785,-2.48841127912311,5.00387330693093));
#14138=CARTESIAN_POINT('Ctrl Pts',(3.43671874458371,-2.43445250733732,5.00016871057866));
#14139=CARTESIAN_POINT('Ctrl Pts',(3.43434538792972,-2.42320442465572,4.9993964616061));
#14140=CARTESIAN_POINT('Ctrl Pts',(3.43324927477267,-2.41168684233781,4.99862421263354));
#14141=CARTESIAN_POINT('Ctrl Pts',(3.4333557533513,-2.40014916294441,4.99785196366098));
#14142=CARTESIAN_POINT('Ctrl Pts',(3.43365998837939,-2.40004261214837,5.01714803633902));
#14143=CARTESIAN_POINT('Ctrl Pts',(3.43360236077384,-2.42521541736454,5.01882514925639));
#14144=CARTESIAN_POINT('Ctrl Pts',(3.43895837597341,-2.45036494625428,5.02050226217376));
#14145=CARTESIAN_POINT('Ctrl Pts',(3.44985377805168,-2.47282762403026,5.02217937509113));
#14146=CARTESIAN_POINT('Ctrl Pts',(3.47392077221621,-2.52244572266223,5.0258839714434));
#14147=CARTESIAN_POINT('Ctrl Pts',(3.52501607564434,-2.55895387890556,5.02958856779567));
#14148=CARTESIAN_POINT('Ctrl Pts',(3.57975563405926,-2.56564394064586,5.03329316414793));
#14149=CARTESIAN_POINT('Ctrl Pts',(3.63449519247418,-2.57233400238615,5.0369977605002));
#14150=CARTESIAN_POINT('Ctrl Pts',(3.69287900587587,-2.54920596962341,5.04070235685248));
#14151=CARTESIAN_POINT('Ctrl Pts',(3.72818738886538,-2.5068444924534,5.04440695320474));
#14152=CARTESIAN_POINT('Ctrl Pts',(3.76349577185488,-2.4644830152834,5.04811154955701));
#14153=CARTESIAN_POINT('Ctrl Pts',(3.77572872443219,-2.40288809370614,5.05181614590928));
#14154=CARTESIAN_POINT('Ctrl Pts',(3.75928777076399,-2.35024904339754,5.05552074226154));
#14155=CARTESIAN_POINT('Ctrl Pts',(3.74284681709578,-2.29760999308894,5.05922533861381));
#14156=CARTESIAN_POINT('Ctrl Pts',(3.69773195718207,-2.25392681404901,5.06292993496608));
#14157=CARTESIAN_POINT('Ctrl Pts',(3.6445902539118,-2.239191259641,5.06663453131835));
#14158=CARTESIAN_POINT('Ctrl Pts',(3.59144855064154,-2.22445570523299,5.07033912767062));
#14159=CARTESIAN_POINT('Ctrl Pts',(3.53028000401472,-2.2386677754569,5.07404372402289));
#14160=CARTESIAN_POINT('Ctrl Pts',(3.48907876340423,-2.27532343849,5.07774832037515));
#14161=CARTESIAN_POINT('Ctrl Pts',(3.45423196569032,-2.3063257203596,5.08088155902977));
#14162=CARTESIAN_POINT('Ctrl Pts',(3.43366833898609,-2.35338253026132,5.0840147976844));
#14163=CARTESIAN_POINT('Ctrl Pts',(3.43326718206005,-2.40013003210005,5.08714803633902));
#14164=CARTESIAN_POINT('Origin',(3.6,-2.4,4.7));
#14165=CARTESIAN_POINT('',(3.43325215766083,-2.39987843114813,5.15714803633902));
#14166=CARTESIAN_POINT('',(3.43361559198215,-2.39990578567643,5.13785196366098));
#14167=CARTESIAN_POINT('',(3.4334,-2.4,4.7));
#14168=CARTESIAN_POINT('',(3.72690708798524,-2.29206413469515,5.2));
#14169=CARTESIAN_POINT('Ctrl Pts',(3.43325215766083,-2.39987843114813,5.15714803633902));
#14170=CARTESIAN_POINT('Ctrl Pts',(3.43364568926707,-2.44715561674071,5.16031823516921));
#14171=CARTESIAN_POINT('Ctrl Pts',(3.45475450700198,-2.49473162154361,5.1634884339994));
#14172=CARTESIAN_POINT('Ctrl Pts',(3.49032381647516,-2.52575978121339,5.16665863282959));
#14173=CARTESIAN_POINT('Ctrl Pts',(3.53188901196771,-2.56201832942672,5.17036322918186));
#14174=CARTESIAN_POINT('Ctrl Pts',(3.59320078561411,-2.575679906312,5.17406782553413));
#14175=CARTESIAN_POINT('Ctrl Pts',(3.64619137793262,-2.5603849196725,5.17777242188639));
#14176=CARTESIAN_POINT('Ctrl Pts',(3.69918197025112,-2.545089933033,5.18147701823866));
#14177=CARTESIAN_POINT('Ctrl Pts',(3.74385138124173,-2.50083838286872,5.18518161459093));
#14178=CARTESIAN_POINT('Ctrl Pts',(3.75975547145412,-2.44813183978448,5.1888862109432));
#14179=CARTESIAN_POINT('Ctrl Pts',(3.7756595616665,-2.39542529670025,5.19259080729546));
#14180=CARTESIAN_POINT('Ctrl Pts',(3.76279833110066,-2.33426376069605,5.19629540364773));
#14181=CARTESIAN_POINT('Ctrl Pts',(3.72690708798524,-2.29206413469515,5.2));
#14182=CARTESIAN_POINT('',(3.47285247305911,-2.29187966783456,5.2));
#14183=CARTESIAN_POINT('Origin',(3.6,-2.4,5.2));
#14184=CARTESIAN_POINT('Ctrl Pts',(3.47285232078578,-2.29187955100914,5.2));
#14185=CARTESIAN_POINT('Ctrl Pts',(3.50793811899511,-2.25072740472549,5.19636770818144));
#14186=CARTESIAN_POINT('Ctrl Pts',(3.5649358740211,-2.22812243199181,5.19273541636289));
#14187=CARTESIAN_POINT('Ctrl Pts',(3.61867624862122,-2.23418211249055,5.18910312454433));
#14188=CARTESIAN_POINT('Ctrl Pts',(3.67348638108252,-2.24036241721079,5.18539852819207));
#14189=CARTESIAN_POINT('Ctrl Pts',(3.72490815931237,-2.27635993281072,5.1816939318398));
#14190=CARTESIAN_POINT('Ctrl Pts',(3.74944162123119,-2.32574103985171,5.17798933548753));
#14191=CARTESIAN_POINT('Ctrl Pts',(3.77397508315002,-2.37512214689269,5.17428473913527));
#14192=CARTESIAN_POINT('Ctrl Pts',(3.77162022875783,-2.43788684537472,5.17058014278299));
#14193=CARTESIAN_POINT('Ctrl Pts',(3.74343805414309,-2.48529019582313,5.16687554643072));
#14194=CARTESIAN_POINT('Ctrl Pts',(3.71525587952836,-2.53269354627153,5.16317095007846));
#14195=CARTESIAN_POINT('Ctrl Pts',(3.66124638469108,-2.5647355486863,5.15946635372619));
#14196=CARTESIAN_POINT('Ctrl Pts',(3.60613566942556,-2.56676214228893,5.15576175737392));
#14197=CARTESIAN_POINT('Ctrl Pts',(3.55102495416005,-2.56878873589157,5.15205716102166));
#14198=CARTESIAN_POINT('Ctrl Pts',(3.49481301846629,-2.54079992068208,5.14835256466939));
#14199=CARTESIAN_POINT('Ctrl Pts',(3.46322140367409,-2.49559987057215,5.14464796831712));
#14200=CARTESIAN_POINT('Ctrl Pts',(3.44390335110665,-2.46796035452279,5.14238263343174));
#14201=CARTESIAN_POINT('Ctrl Pts',(3.43379142096037,-2.43388514918463,5.14011729854636));
#14202=CARTESIAN_POINT('Ctrl Pts',(3.43361559198215,-2.39990578567643,5.13785196366098));
#14203=CARTESIAN_POINT('Origin',(3.6,-2.4,5.35459252805377));
#14204=CARTESIAN_POINT('',(3.39427732444531,-2.39988044480691,4.34540747194623));
#14205=CARTESIAN_POINT('',(3.39483887958286,-2.40008013132228,4.33959252805377));
#14206=CARTESIAN_POINT('',(3.394525,-2.39999999999999,5.35459252805377));
#14207=CARTESIAN_POINT('',(3.78826275096636,-2.48232321801033,4.3));
#14208=CARTESIAN_POINT('Ctrl Pts',(3.39483887958286,-2.40008013132228,4.33959252805377));
#14209=CARTESIAN_POINT('Ctrl Pts',(3.39495668787724,-2.361520075325,4.33750880775932));
#14210=CARTESIAN_POINT('Ctrl Pts',(3.4239416532562,-2.25423614055743,4.3317204911126));
#14211=CARTESIAN_POINT('Ctrl Pts',(3.59702530195382,-2.15700945407857,4.32222757811361));
#14212=CARTESIAN_POINT('Ctrl Pts',(3.80250230755732,-2.26611609660926,4.31111378905681));
#14213=CARTESIAN_POINT('Ctrl Pts',(3.81563717950601,-2.41972137435598,4.30370459635227));
#14214=CARTESIAN_POINT('Ctrl Pts',(3.78826275096636,-2.48232321801033,4.3));
#14215=CARTESIAN_POINT('',(3.72235839003881,-2.56553532314028,4.3));
#14216=CARTESIAN_POINT('Origin',(3.6,-2.4,4.3));
#14217=CARTESIAN_POINT('Ctrl Pts',(3.39427732444531,-2.39988044480691,4.34540747194623));
#14218=CARTESIAN_POINT('Ctrl Pts',(3.39422705601106,-2.39271640856816,4.34501772883951));
#14219=CARTESIAN_POINT('Ctrl Pts',(3.39781628789546,-2.31750701228878,4.34092338938053));
#14220=CARTESIAN_POINT('Ctrl Pts',(3.49037003077072,-2.18326698967564,4.33312445356928));
#14221=CARTESIAN_POINT('Ctrl Pts',(3.72265543153543,-2.19039239422561,4.32201066451247));
#14222=CARTESIAN_POINT('Ctrl Pts',(3.84179827282652,-2.38799091139141,4.31096917998938));
#14223=CARTESIAN_POINT('Ctrl Pts',(3.77594285680537,-2.52582029152411,4.30363229181855));
#14224=CARTESIAN_POINT('Ctrl Pts',(3.72235852099786,-2.56553552032367,4.3));
#14225=CARTESIAN_POINT('Origin',(3.6,-2.4,5.35459252805377));
#14226=CARTESIAN_POINT('',(3.39480735688311,-2.3998973457609,4.41540747194623));
#14227=CARTESIAN_POINT('',(3.39433274578554,-2.4001497810388,4.40959252805377));
#14228=CARTESIAN_POINT('',(3.394525,-2.39999999999999,5.35459252805377));
#14229=CARTESIAN_POINT('Ctrl Pts',(3.39433274578554,-2.4001497810388,4.40959252805377));
#14230=CARTESIAN_POINT('Ctrl Pts',(3.39481384891428,-2.34148051031483,4.40640305253959));
#14231=CARTESIAN_POINT('Ctrl Pts',(3.45186170282621,-2.21384965704481,4.39950898067315));
#14232=CARTESIAN_POINT('Ctrl Pts',(3.66843098386609,-2.16697244123634,4.38891031245443));
#14233=CARTESIAN_POINT('Ctrl Pts',(3.83289206448147,-2.33111753521892,4.37779652339763));
#14234=CARTESIAN_POINT('Ctrl Pts',(3.7841810615649,-2.55829573402952,4.36668273434082));
#14235=CARTESIAN_POINT('Ctrl Pts',(3.56689372435994,-2.6406156849541,4.35556894528403));
#14236=CARTESIAN_POINT('Ctrl Pts',(3.4149557748622,-2.52850415334516,4.34653887652167));
#14237=CARTESIAN_POINT('Ctrl Pts',(3.39474723933523,-2.4300750743674,4.34121340411158));
#14238=CARTESIAN_POINT('Ctrl Pts',(3.39483887958286,-2.40008013132228,4.33959252805377));
#14239=CARTESIAN_POINT('Ctrl Pts',(3.39480735688311,-2.3998973457609,4.41540747194623));
#14240=CARTESIAN_POINT('Ctrl Pts',(3.39468219270667,-2.3722256242847,4.41391197361979));
#14241=CARTESIAN_POINT('Ctrl Pts',(3.4127838411683,-2.27616341542302,4.40871187894107));
#14242=CARTESIAN_POINT('Ctrl Pts',(3.55878722400007,-2.16065655916503,4.3998071879101));
#14243=CARTESIAN_POINT('Ctrl Pts',(3.77873474447839,-2.23556893008468,4.38869339885329));
#14244=CARTESIAN_POINT('Ctrl Pts',(3.83508286096032,-2.4609855401145,4.37757960979649));
#14245=CARTESIAN_POINT('Ctrl Pts',(3.67625990251943,-2.63058416437082,4.36646582073969));
#14246=CARTESIAN_POINT('Ctrl Pts',(3.45564722516575,-2.59057499098668,4.3557417747896));
#14247=CARTESIAN_POINT('Ctrl Pts',(3.39470486884463,-2.46081219284274,4.34872232519178));
#14248=CARTESIAN_POINT('Ctrl Pts',(3.39427732444531,-2.39988044480691,4.34540747194623));
#14249=CARTESIAN_POINT('Origin',(3.6,-2.4,5.35459252805377));
#14250=CARTESIAN_POINT('',(3.39465010821578,-2.400176527643,4.48540747194623));
#14251=CARTESIAN_POINT('',(3.39437120606287,-2.39983660975581,4.47959252805377));
#14252=CARTESIAN_POINT('',(3.394525,-2.39999999999999,5.35459252805377));
#14253=CARTESIAN_POINT('Ctrl Pts',(3.39437120606287,-2.39983660975581,4.47959252805376));
#14254=CARTESIAN_POINT('Ctrl Pts',(3.39427673427304,-2.3889667776849,4.47900189367213));
#14255=CARTESIAN_POINT('Ctrl Pts',(3.40000383699504,-2.31001856010007,4.47470666293823));
#14256=CARTESIAN_POINT('Ctrl Pts',(3.50226148839652,-2.17766948860297,4.46670683585206));
#14257=CARTESIAN_POINT('Ctrl Pts',(3.73378446004359,-2.19730463405286,4.45559304679526));
#14258=CARTESIAN_POINT('Ctrl Pts',(3.84285302402677,-2.40246926900864,4.44447925773845));
#14259=CARTESIAN_POINT('Ctrl Pts',(3.72963540924699,-2.60537350906572,4.43336546868165));
#14260=CARTESIAN_POINT('Ctrl Pts',(3.49776113780875,-2.62029753773771,4.42225167962485));
#14261=CARTESIAN_POINT('Ctrl Pts',(3.39915518843152,-2.48716469789757,4.41432736608222));
#14262=CARTESIAN_POINT('Ctrl Pts',(3.3942550445316,-2.40962524613366,4.41010764889186));
#14263=CARTESIAN_POINT('Ctrl Pts',(3.39433274578554,-2.4001497810388,4.40959252805377));
#14264=CARTESIAN_POINT('Ctrl Pts',(3.39465010821578,-2.400176527643,4.48540747194623));
#14265=CARTESIAN_POINT('Ctrl Pts',(3.3950436881435,-2.35213729673001,4.48280621840006));
#14266=CARTESIAN_POINT('Ctrl Pts',(3.43581223913156,-2.23508079066125,4.47650036850162));
#14267=CARTESIAN_POINT('Ctrl Pts',(3.63081864021225,-2.15909778094929,4.46648992225093));
#14268=CARTESIAN_POINT('Ctrl Pts',(3.81910984016012,-2.29524053287965,4.45537613319411));
#14269=CARTESIAN_POINT('Ctrl Pts',(3.80684729577664,-2.52727079162485,4.44426234413733));
#14270=CARTESIAN_POINT('Ctrl Pts',(3.60525512132335,-2.64280869447754,4.4331485550805));
#14271=CARTESIAN_POINT('Ctrl Pts',(3.42662678112532,-2.55045981030713,4.42353026435015));
#14272=CARTESIAN_POINT('Ctrl Pts',(3.39499224504393,-2.44077304866432,4.41761656997206));
#14273=CARTESIAN_POINT('Ctrl Pts',(3.39480735688311,-2.3998973457609,4.41540747194623));
#14274=CARTESIAN_POINT('Origin',(3.6,-2.4,5.35459252805377));
#14275=CARTESIAN_POINT('',(3.39418406677318,-2.39999917227821,4.55540747194623));
#14276=CARTESIAN_POINT('',(3.39484823116951,-2.39995310238382,4.54959252805377));
#14277=CARTESIAN_POINT('',(3.394525,-2.39999999999999,5.35459252805377));
#14278=CARTESIAN_POINT('Ctrl Pts',(3.39484823116951,-2.39995310238382,4.54959252805377));
#14279=CARTESIAN_POINT('Ctrl Pts',(3.3947841219125,-2.36854855723416,4.54789613845241));
#14280=CARTESIAN_POINT('Ctrl Pts',(3.41632348134282,-2.26864576454574,4.54249515249878));
#14281=CARTESIAN_POINT('Ctrl Pts',(3.57178888017207,-2.15877849637109,4.53338957019289));
#14282=CARTESIAN_POINT('Ctrl Pts',(3.78736362800739,-2.2454731342224,4.52227578113608));
#14283=CARTESIAN_POINT('Ctrl Pts',(3.83144232268012,-2.47360796667095,4.51116199207928));
#14284=CARTESIAN_POINT('Ctrl Pts',(3.66367923386702,-2.6343685886554,4.50004820302247));
#14285=CARTESIAN_POINT('Ctrl Pts',(3.44964305628728,-2.58346600654441,4.48952504834731));
#14286=CARTESIAN_POINT('Ctrl Pts',(3.39486928333363,-2.45714489513262,4.4827064900244));
#14287=CARTESIAN_POINT('Ctrl Pts',(3.39437120606287,-2.39983660975581,4.47959252805376));
#14288=CARTESIAN_POINT('Ctrl Pts',(3.39418406845602,-2.39999917228229,4.55540747194623));
#14289=CARTESIAN_POINT('Ctrl Pts',(3.39418406581063,-2.39995488126817,4.55540505953261));
#14290=CARTESIAN_POINT('Ctrl Pts',(3.39420413582033,-2.33189558582108,4.55169805076672));
#14291=CARTESIAN_POINT('Ctrl Pts',(3.46841583417461,-2.19586946879708,4.54428644564855));
#14292=CARTESIAN_POINT('Ctrl Pts',(3.70013762796088,-2.17873969637961,4.53317265659175));
#14293=CARTESIAN_POINT('Ctrl Pts',(3.84020231541317,-2.36413198929513,4.52205886753494));
#14294=CARTESIAN_POINT('Ctrl Pts',(3.7604070991348,-2.58235467884591,4.51094507847814));
#14295=CARTESIAN_POINT('Ctrl Pts',(3.53378944658573,-2.63366606347461,4.49983128942134));
#14296=CARTESIAN_POINT('Ctrl Pts',(3.40663179333208,-2.50914981953724,4.4913187539107));
#14297=CARTESIAN_POINT('Ctrl Pts',(3.39448316809474,-2.42055275737136,4.48651081475233));
#14298=CARTESIAN_POINT('Ctrl Pts',(3.39465010821578,-2.400176527643,4.48540747194623));
#14299=CARTESIAN_POINT('Origin',(3.6,-2.4,5.35459252805377));
#14300=CARTESIAN_POINT('',(3.39465252302706,-2.39982399270837,4.62540747194623));
#14301=CARTESIAN_POINT('',(3.39454319301877,-2.40018789160095,4.61959252805377));
#14302=CARTESIAN_POINT('',(3.394525,-2.39999999999999,5.35459252805377));
#14303=CARTESIAN_POINT('Ctrl Pts',(3.39454319301877,-2.40018789160095,4.61959252805377));
#14304=CARTESIAN_POINT('Ctrl Pts',(3.39501369486734,-2.34850703974388,4.61679038323268));
#14305=CARTESIAN_POINT('Ctrl Pts',(3.44097935155591,-2.22775547868952,4.61028364205933));
#14306=CARTESIAN_POINT('Ctrl Pts',(3.64379902793915,-2.16111650041238,4.60007230453371));
#14307=CARTESIAN_POINT('Ctrl Pts',(3.82445363439269,-2.30724091831967,4.58895851547691));
#14308=CARTESIAN_POINT('Ctrl Pts',(3.79966328381548,-2.53826877567792,4.57784472642011));
#14309=CARTESIAN_POINT('Ctrl Pts',(3.59211886521387,-2.64273765452468,4.5667309373633));
#14310=CARTESIAN_POINT('Ctrl Pts',(3.42236627541046,-2.54299330864641,4.55731353790785));
#14311=CARTESIAN_POINT('Ctrl Pts',(3.39492412449178,-2.43713018689806,4.55160073480468));
#14312=CARTESIAN_POINT('Ctrl Pts',(3.39484823116951,-2.39995310238382,4.54959252805377));
#14313=CARTESIAN_POINT('Ctrl Pts',(3.39465252302706,-2.39982399270837,4.62540747194623));
#14314=CARTESIAN_POINT('Ctrl Pts',(3.39448549072207,-2.37935805029673,4.62429930431288));
#14315=CARTESIAN_POINT('Ctrl Pts',(3.40670160391397,-2.29066952405396,4.61948654032727));
#14316=CARTESIAN_POINT('Ctrl Pts',(3.53409308711521,-2.16624811163355,4.61096917998937));
#14317=CARTESIAN_POINT('Ctrl Pts',(3.76064388390312,-2.21785387995996,4.59985539093258));
#14318=CARTESIAN_POINT('Ctrl Pts',(3.8401555119317,-2.4361800576391,4.58874160187577));
#14319=CARTESIAN_POINT('Ctrl Pts',(3.69985007633495,-2.62139021824623,4.57762781281896));
#14320=CARTESIAN_POINT('Ctrl Pts',(3.4682010273,-2.60396318498582,4.56651643617578));
#14321=CARTESIAN_POINT('Ctrl Pts',(3.39418812817678,-2.46796988817124,4.55910965588488));
#14322=CARTESIAN_POINT('Ctrl Pts',(3.39418406845602,-2.39999917228229,4.55540747194623));
#14323=CARTESIAN_POINT('Origin',(3.6,-2.4,5.35459252805377));
#14324=CARTESIAN_POINT('',(3.39480597714356,-2.40010391086475,4.69540747194623));
#14325=CARTESIAN_POINT('',(3.39421139045774,-2.39993212258527,4.68959252805377));
#14326=CARTESIAN_POINT('',(3.394525,-2.39999999999999,5.35459252805377));
#14327=CARTESIAN_POINT('Ctrl Pts',(3.39421139045774,-2.39993212258527,4.68959252805377));
#14328=CARTESIAN_POINT('Ctrl Pts',(3.39419531835948,-2.39619821368606,4.68938922436523));
#14329=CARTESIAN_POINT('Ctrl Pts',(3.3959796089401,-2.32444075084805,4.68548132432442));
#14330=CARTESIAN_POINT('Ctrl Pts',(3.47964553863801,-2.18905336016944,4.67786882793135));
#14331=CARTESIAN_POINT('Ctrl Pts',(3.71195459122784,-2.18447772567898,4.66675503887453));
#14332=CARTESIAN_POINT('Ctrl Pts',(3.84179033681535,-2.37717207306315,4.65564124981774));
#14333=CARTESIAN_POINT('Ctrl Pts',(3.75031264502696,-2.59076108085938,4.64452746076093));
#14334=CARTESIAN_POINT('Ctrl Pts',(3.52125208458385,-2.6297443079663,4.63341367170413));
#14335=CARTESIAN_POINT('Ctrl Pts',(3.40385053605922,-2.50163131684181,4.6251020274684));
#14336=CARTESIAN_POINT('Ctrl Pts',(3.39439166440737,-2.4168320934068,4.62049497958495));
#14337=CARTESIAN_POINT('Ctrl Pts',(3.39454319301877,-2.40018789160095,4.61959252805377));
#14338=CARTESIAN_POINT('Ctrl Pts',(3.39480597714356,-2.40010391086475,4.69540747194623));
#14339=CARTESIAN_POINT('Ctrl Pts',(3.39499357523214,-2.35913959871511,4.69319354909316));
#14340=CARTESIAN_POINT('Ctrl Pts',(3.42673278397032,-2.24936123585863,4.68727502988782));
#14341=CARTESIAN_POINT('Ctrl Pts',(3.60557055480924,-2.15719836203143,4.6776519143302));
#14342=CARTESIAN_POINT('Ctrl Pts',(3.8070124874506,-2.27299804520947,4.6665381252734));
#14343=CARTESIAN_POINT('Ctrl Pts',(3.81897354264718,-2.50504405790744,4.65542433621659));
#14344=CARTESIAN_POINT('Ctrl Pts',(3.63050563092984,-2.64094205312202,4.64431054715979));
#14345=CARTESIAN_POINT('Ctrl Pts',(3.4356920506335,-2.56474249848871,4.63430492573633));
#14346=CARTESIAN_POINT('Ctrl Pts',(3.39504387850492,-2.44777554718273,4.62800390066515));
#14347=CARTESIAN_POINT('Ctrl Pts',(3.39465252302706,-2.39982399270837,4.62540747194623));
#14348=CARTESIAN_POINT('Origin',(3.6,-2.4,5.35459252805377));
#14349=CARTESIAN_POINT('',(3.39427330737243,-2.40012021866021,4.76540747194624));
#14350=CARTESIAN_POINT('',(3.39474358824326,-2.39985490132356,4.75959252805377));
#14351=CARTESIAN_POINT('',(3.394525,-2.39999999999999,5.35459252805377));
#14352=CARTESIAN_POINT('Ctrl Pts',(3.39474358824326,-2.39985490132356,4.75959252805377));
#14353=CARTESIAN_POINT('Ctrl Pts',(3.39458577609892,-2.37565177668507,4.75828346914551));
#14354=CARTESIAN_POINT('Ctrl Pts',(3.40973684003147,-2.28314575562072,4.75326981388497));
#14355=CARTESIAN_POINT('Ctrl Pts',(3.546828337511,-2.16302646659663,4.74455156227216));
#14356=CARTESIAN_POINT('Ctrl Pts',(3.77025746015408,-2.22680624004484,4.73343777321537));
#14357=CARTESIAN_POINT('Ctrl Pts',(3.83784799866721,-2.44911222613084,4.72232398415856));
#14358=CARTESIAN_POINT('Ctrl Pts',(3.68773356662048,-2.62646523466876,4.71121019510175));
#14359=CARTESIAN_POINT('Ctrl Pts',(3.46153062411222,-2.59707961114918,4.7002997097335));
#14360=CARTESIAN_POINT('Ctrl Pts',(3.3944881838605,-2.46423743809455,4.6930938207175));
#14361=CARTESIAN_POINT('Ctrl Pts',(3.39421139045774,-2.39993212258527,4.68959252805377));
#14362=CARTESIAN_POINT('Ctrl Pts',(3.39427330737243,-2.40012021866021,4.76540747194624));
#14363=CARTESIAN_POINT('Ctrl Pts',(3.39469744970711,-2.3391019374956,4.76208779387343));
#14364=CARTESIAN_POINT('Ctrl Pts',(3.45579878082125,-2.20925256261312,4.75506351944836));
#14365=CARTESIAN_POINT('Ctrl Pts',(3.67655777933124,-2.16951665373617,4.74433464867103));
#14366=CARTESIAN_POINT('Ctrl Pts',(3.83516271561975,-2.33931916560024,4.73322085961422));
#14367=CARTESIAN_POINT('Ctrl Pts',(3.77852055137491,-2.56466353335787,4.72210707055742));
#14368=CARTESIAN_POINT('Ctrl Pts',(3.55847650189588,-2.63928950162157,4.71099328150062));
#14369=CARTESIAN_POINT('Ctrl Pts',(3.41270209403565,-2.52365597038275,4.70209341529688));
#14370=CARTESIAN_POINT('Ctrl Pts',(3.3946796640253,-2.4276859083356,4.69689814544542));
#14371=CARTESIAN_POINT('Ctrl Pts',(3.39480597714356,-2.40010391086475,4.69540747194623));
#14372=CARTESIAN_POINT('Origin',(3.6,-2.4,5.35459252805377));
#14373=CARTESIAN_POINT('',(3.39444175959654,-2.39982008597895,4.83540747194623));
#14374=CARTESIAN_POINT('',(3.39473575570154,-2.40014879661129,4.82959252805377));
#14375=CARTESIAN_POINT('',(3.394525,-2.39999999999999,5.35459252805377));
#14376=CARTESIAN_POINT('Ctrl Pts',(3.39473575570154,-2.40014879661129,4.82959252805377));
#14377=CARTESIAN_POINT('Ctrl Pts',(3.39503502367394,-2.35550570215801,4.82717771392578));
#14378=CARTESIAN_POINT('Ctrl Pts',(3.43129921618784,-2.24193240937533,4.82105830344552));
#14379=CARTESIAN_POINT('Ctrl Pts',(3.61869057055051,-2.15785470519124,4.81123429661299));
#14380=CARTESIAN_POINT('Ctrl Pts',(3.81357662274397,-2.28437687323548,4.80012050755619));
#14381=CARTESIAN_POINT('Ctrl Pts',(3.81297357001622,-2.51673020046272,4.78900671849938));
#14382=CARTESIAN_POINT('Ctrl Pts',(3.61743339336808,-2.64223905139592,4.77789292944258));
#14383=CARTESIAN_POINT('Ctrl Pts',(3.43084783163214,-2.55735665460818,4.76808819929404));
#14384=CARTESIAN_POINT('Ctrl Pts',(3.39503237960207,-2.44414587323265,4.76198806549777));
#14385=CARTESIAN_POINT('Ctrl Pts',(3.39474358824326,-2.39985490132356,4.75959252805377));
#14386=CARTESIAN_POINT('Ctrl Pts',(3.39444175959654,-2.39982008597895,4.83540747194623));
#14387=CARTESIAN_POINT('Ctrl Pts',(3.39432007222796,-2.3865422800919,4.83468663500598));
#14388=CARTESIAN_POINT('Ctrl Pts',(3.40154215697383,-2.30515767781734,4.83026120171345));
#14389=CARTESIAN_POINT('Ctrl Pts',(3.51011506636152,-2.17438004258061,4.82213117206865));
#14390=CARTESIAN_POINT('Ctrl Pts',(3.74080744720095,-2.20211890112026,4.81101738301186));
#14391=CARTESIAN_POINT('Ctrl Pts',(3.84261717475225,-2.41098057358878,4.79990359395505));
#14392=CARTESIAN_POINT('Ctrl Pts',(3.72235665078693,-2.60979160252334,4.78878980489825));
#14393=CARTESIAN_POINT('Ctrl Pts',(3.49010169673754,-2.61657799846968,4.77767601584144));
#14394=CARTESIAN_POINT('Ctrl Pts',(3.3977657533099,-2.4823139974067,4.76988190485744));
#14395=CARTESIAN_POINT('Ctrl Pts',(3.39422412786341,-2.40719531789781,4.7657923902257));
#14396=CARTESIAN_POINT('Ctrl Pts',(3.39427330737243,-2.40012021866021,4.76540747194624));
#14397=CARTESIAN_POINT('Origin',(3.6,-2.4,5.35459252805377));
#14398=CARTESIAN_POINT('',(3.39485784898994,-2.39999218980985,4.90540747194623));
#14399=CARTESIAN_POINT('',(3.39420666496973,-2.4000617379826,4.89959252805377));
#14400=CARTESIAN_POINT('',(3.394525,-2.39999999999999,5.35459252805377));
#14401=CARTESIAN_POINT('Ctrl Pts',(3.39420666496973,-2.4000617379826,4.89959252805377));
#14402=CARTESIAN_POINT('Ctrl Pts',(3.39446260190468,-2.33540634192885,4.89607195870605));
#14403=CARTESIAN_POINT('Ctrl Pts',(3.46215556821269,-2.20225412189412,4.88884679300607));
#14404=CARTESIAN_POINT('Ctrl Pts',(3.68890791813162,-2.17399322284688,4.87791703095382));
#14405=CARTESIAN_POINT('Ctrl Pts',(3.83809972557463,-2.3521230545377,4.86680324189701));
#14406=CARTESIAN_POINT('Ctrl Pts',(3.76935615396461,-2.57407519737118,4.85568945284021));
#14407=CARTESIAN_POINT('Ctrl Pts',(3.54559897400137,-2.63669433790405,4.8445756637834));
#14408=CARTESIAN_POINT('Ctrl Pts',(3.4094345739418,-2.51613221625325,4.83587668885459));
#14409=CARTESIAN_POINT('Ctrl Pts',(3.39457591295976,-2.42399322794668,4.83088231027805));
#14410=CARTESIAN_POINT('Ctrl Pts',(3.39473575570154,-2.40014879661129,4.82959252805377));
#14411=CARTESIAN_POINT('Ctrl Pts',(3.39485784898994,-2.39999218980985,4.90540747194623));
#14412=CARTESIAN_POINT('Ctrl Pts',(3.3948463830005,-2.36617331876133,4.90358087978625));
#14413=CARTESIAN_POINT('Ctrl Pts',(3.41876410056102,-2.26378009325356,4.898049691274));
#14414=CARTESIAN_POINT('Ctrl Pts',(3.5802619217345,-2.1579378700657,4.88881390640948));
#14415=CARTESIAN_POINT('Ctrl Pts',(3.7926651914697,-2.25213590538246,4.87770011735268));
#14416=CARTESIAN_POINT('Ctrl Pts',(3.8287198264784,-2.48167562339262,4.86658632829587));
#14417=CARTESIAN_POINT('Ctrl Pts',(3.65542461045338,-2.63645671704841,4.85547253923907));
#14418=CARTESIAN_POINT('Ctrl Pts',(3.44592887677019,-2.57880492333736,4.84507958712252));
#14419=CARTESIAN_POINT('Ctrl Pts',(3.39494545996352,-2.45478089066832,4.83839123135824));
#14420=CARTESIAN_POINT('Ctrl Pts',(3.39444175959654,-2.39982008597895,4.83540747194623));
#14421=CARTESIAN_POINT('Origin',(3.6,-2.4,5.35459252805377));
#14422=CARTESIAN_POINT('',(3.39447042869063,-2.40018396912367,4.97540747194623));
#14423=CARTESIAN_POINT('',(3.39455385196002,-2.39981229693528,4.96959252805377));
#14424=CARTESIAN_POINT('',(3.394525,-2.39999999999999,5.35459252805377));
#14425=CARTESIAN_POINT('Ctrl Pts',(3.39455385196002,-2.39981229693529,4.96959252805377));
#14426=CARTESIAN_POINT('Ctrl Pts',(3.39439994110979,-2.38281031884833,4.9686707998386));
#14427=CARTESIAN_POINT('Ctrl Pts',(3.40410690463755,-2.29764758883809,4.96404447527116));
#14428=CARTESIAN_POINT('Ctrl Pts',(3.52244569995759,-2.16985002334435,4.95571355435144));
#14429=CARTESIAN_POINT('Ctrl Pts',(3.75130082069111,-2.21002173048044,4.94459976529465));
#14430=CARTESIAN_POINT('Ctrl Pts',(3.84166858438312,-2.42408270226789,4.93348597623783));
#14431=CARTESIAN_POINT('Ctrl Pts',(3.71083435207858,-2.61610050352316,4.92237218718104));
#14432=CARTESIAN_POINT('Ctrl Pts',(3.47855218037073,-2.61031906317225,4.91125839812423));
#14433=CARTESIAN_POINT('Ctrl Pts',(3.3958002253152,-2.47484313295797,4.90366517841514));
#14434=CARTESIAN_POINT('Ctrl Pts',(3.39419328664854,-2.40344140123838,4.89977655505832));
#14435=CARTESIAN_POINT('Ctrl Pts',(3.39420666496973,-2.4000617379826,4.89959252805377));
#14436=CARTESIAN_POINT('Ctrl Pts',(3.39447042869063,-2.40018396912367,4.97540747194623));
#14437=CARTESIAN_POINT('Ctrl Pts',(3.39496908844141,-2.34615078794508,4.97247512456653));
#14438=CARTESIAN_POINT('Ctrl Pts',(3.44450059908404,-2.22304562253723,4.96583818083456));
#14439=CARTESIAN_POINT('Ctrl Pts',(3.65214584962031,-2.16279865748873,4.9554966407503));
#14440=CARTESIAN_POINT('Ctrl Pts',(3.82756721091734,-2.31516586178242,4.94438285169351));
#14441=CARTESIAN_POINT('Ctrl Pts',(3.79469372311971,-2.54518271468373,4.9332690626367));
#14442=CARTESIAN_POINT('Ctrl Pts',(3.58361486265069,-2.64231218244471,4.9221552735799));
#14443=CARTESIAN_POINT('Ctrl Pts',(3.41976019754822,-2.53813915804107,4.91286807668307));
#14444=CARTESIAN_POINT('Ctrl Pts',(3.39486963770596,-2.43476294104758,4.90728547613852));
#14445=CARTESIAN_POINT('Ctrl Pts',(3.39485784898994,-2.39999218980985,4.90540747194623));
#14446=CARTESIAN_POINT('Origin',(3.6,-2.4,5.35459252805377));
#14447=CARTESIAN_POINT('',(3.39425291505627,-2.39989343747799,5.04540747194623));
#14448=CARTESIAN_POINT('',(3.39484565493551,-2.40005255540929,5.03959252805377));
#14449=CARTESIAN_POINT('',(3.394525,-2.39999999999999,5.35459252805377));
#14450=CARTESIAN_POINT('Ctrl Pts',(3.39484565493551,-2.40005255540928,5.03959252805377));
#14451=CARTESIAN_POINT('Ctrl Pts',(3.39493157796431,-2.36251978536397,5.03756504461887));
#14452=CARTESIAN_POINT('Ctrl Pts',(3.42276239101834,-2.25628891765328,5.03183296483171));
#14453=CARTESIAN_POINT('Ctrl Pts',(3.59337897177386,-2.15722470850713,5.02239628869227));
#14454=CARTESIAN_POINT('Ctrl Pts',(3.8003783179889,-2.26276949623011,5.01128249963547));
#14455=CARTESIAN_POINT('Ctrl Pts',(3.82396911763155,-2.49392292422242,5.00016871057867));
#14456=CARTESIAN_POINT('Ctrl Pts',(3.64255844375993,-2.63910763258347,4.98905492152186));
#14457=CARTESIAN_POINT('Ctrl Pts',(3.44046962807591,-2.57154454308001,4.97886286068022));
#14458=CARTESIAN_POINT('Ctrl Pts',(3.39501853731303,-2.45114441665013,4.97237539619086));
#14459=CARTESIAN_POINT('Ctrl Pts',(3.39455385196002,-2.39981229693529,4.96959252805377));
#14460=CARTESIAN_POINT('Ctrl Pts',(3.39425291505627,-2.39989343747799,5.04540747194623));
#14461=CARTESIAN_POINT('Ctrl Pts',(3.39421423202935,-2.39376493107826,5.04507396569907));
#14462=CARTESIAN_POINT('Ctrl Pts',(3.39724233967252,-2.31959956972988,5.04103586309963));
#14463=CARTESIAN_POINT('Ctrl Pts',(3.48711398605093,-2.18496417501817,5.03329316414794));
#14464=CARTESIAN_POINT('Ctrl Pts',(3.71944061581356,-2.18853461914439,5.02217937509113));
#14465=CARTESIAN_POINT('Ctrl Pts',(3.84244191526684,-2.38566174871763,5.01106558603433));
#14466=CARTESIAN_POINT('Ctrl Pts',(3.74353337026135,-2.59591283022398,4.99995179697752));
#14467=CARTESIAN_POINT('Ctrl Pts',(3.51324710863985,-2.62684268245385,4.98883800792072));
#14468=CARTESIAN_POINT('Ctrl Pts',(3.40217618139952,-2.49676321865199,4.98065656624362));
#14469=CARTESIAN_POINT('Ctrl Pts',(3.3943391040451,-2.41441388913183,4.97617972091879));
#14470=CARTESIAN_POINT('Ctrl Pts',(3.39447042869063,-2.40018396912367,4.97540747194623));
#14471=CARTESIAN_POINT('Origin',(3.6,-2.4,5.35459252805377));
#14472=CARTESIAN_POINT('',(3.39479089893477,-2.39988380139174,5.11540747194623));
#14473=CARTESIAN_POINT('',(3.39436118987868,-2.40016037422423,5.10959252805377));
#14474=CARTESIAN_POINT('',(3.394525,-2.39999999999999,5.35459252805377));
#14475=CARTESIAN_POINT('Ctrl Pts',(3.39436118987868,-2.40016037422423,5.10959252805377));
#14476=CARTESIAN_POINT('Ctrl Pts',(3.39485595410064,-2.34250465429438,5.10645928939914));
#14477=CARTESIAN_POINT('Ctrl Pts',(3.45020483509149,-2.21584694899168,5.09962145439226));
#14478=CARTESIAN_POINT('Ctrl Pts',(3.66489494634582,-2.16596525152154,5.08907902303309));
#14479=CARTESIAN_POINT('Ctrl Pts',(3.83182128201397,-2.32759432498908,5.07796523397629));
#14480=CARTESIAN_POINT('Ctrl Pts',(3.78655899034249,-2.55549738341204,5.06685144491949));
#14481=CARTESIAN_POINT('Ctrl Pts',(3.57053712854092,-2.64107179875281,5.05573765586268));
#14482=CARTESIAN_POINT('Ctrl Pts',(3.4159720352905,-2.53063333972521,5.04665135024078));
#14483=CARTESIAN_POINT('Ctrl Pts',(3.39477458031215,-2.43109926700468,5.04126964097114));
#14484=CARTESIAN_POINT('Ctrl Pts',(3.39484565493551,-2.40005255540928,5.03959252805377));
#14485=CARTESIAN_POINT('Ctrl Pts',(3.39479089893477,-2.39988380139174,5.11540747194623));
#14486=CARTESIAN_POINT('Ctrl Pts',(3.39465312034679,-2.37325776527266,5.11396821047934));
#14487=CARTESIAN_POINT('Ctrl Pts',(3.41183995517004,-2.27826800227929,5.10882435266019));
#14488=CARTESIAN_POINT('Ctrl Pts',(3.55516853033383,-2.16130913937078,5.09997589848876));
#14489=CARTESIAN_POINT('Ctrl Pts',(3.77622352465696,-2.23288041708187,5.08886210943196));
#14490=CARTESIAN_POINT('Ctrl Pts',(3.83598040928192,-2.457419700552,5.07774832037515));
#14491=CARTESIAN_POINT('Ctrl Pts',(3.67974110927284,-2.62940130358481,5.06663453131835));
#14492=CARTESIAN_POINT('Ctrl Pts',(3.45739290427932,-2.59254974530072,5.05585424850871));
#14493=CARTESIAN_POINT('Ctrl Pts',(3.39464392413157,-2.46184054479285,5.04877856205133));
#14494=CARTESIAN_POINT('Ctrl Pts',(3.39425291505627,-2.39989343747799,5.04540747194623));
#14495=CARTESIAN_POINT('Origin',(3.6,-2.4,5.35459252805377));
#14496=CARTESIAN_POINT('',(3.39473290683218,-2.40022967700174,5.18540747194623));
#14497=CARTESIAN_POINT('',(3.39434265963601,-2.39985006386652,5.17959252805377));
#14498=CARTESIAN_POINT('',(3.394525,-2.39999999999999,5.35459252805377));
#14499=CARTESIAN_POINT('',(3.54698297828114,-2.59851743256717,5.2));
#14500=CARTESIAN_POINT('Ctrl Pts',(3.54698297828114,-2.59851743256717,5.2));
#14501=CARTESIAN_POINT('Ctrl Pts',(3.48097120902544,-2.58088801151799,5.19629540364773));
#14502=CARTESIAN_POINT('Ctrl Pts',(3.40750558819668,-2.51127201784738,5.19143122762981));
#14503=CARTESIAN_POINT('Ctrl Pts',(3.39457125535004,-2.42165321144002,5.18656705161189));
#14504=CARTESIAN_POINT('Ctrl Pts',(3.39473290683218,-2.40022967700174,5.18540747194623));
#14505=CARTESIAN_POINT('',(3.65313154707148,-2.59887322485902,5.2));
#14506=CARTESIAN_POINT('Origin',(3.6,-2.4,5.2));
#14507=CARTESIAN_POINT('Ctrl Pts',(3.65313161981587,-2.59887345085171,5.2));
#14508=CARTESIAN_POINT('Ctrl Pts',(3.58867174169549,-2.61600530781671,5.19636770818145));
#14509=CARTESIAN_POINT('Ctrl Pts',(3.45069167513782,-2.58406709125274,5.1895652175327));
#14510=CARTESIAN_POINT('Ctrl Pts',(3.3948280192206,-2.45815906572508,5.18276272688396));
#14511=CARTESIAN_POINT('Ctrl Pts',(3.39434265963601,-2.39985006386652,5.17959252805377));
#14512=CARTESIAN_POINT('Origin',(-3.6,-2.4,4.7));
#14513=CARTESIAN_POINT('',(-3.76675587540948,-2.40012144305632,4.38714803633902));
#14514=CARTESIAN_POINT('',(-3.76680083731002,-2.3999030629831,4.36785196366098));
#14515=CARTESIAN_POINT('',(-3.7666,-2.4,4.7));
#14516=CARTESIAN_POINT('',(-3.76351293272515,-2.4319230454628,4.3));
#14517=CARTESIAN_POINT('Ctrl Pts',(-3.76680083731002,-2.3999030629831,4.36785196366098));
#14518=CARTESIAN_POINT('Ctrl Pts',(-3.76684159509423,-2.39409443145766,
4.36746222055426));
#14519=CARTESIAN_POINT('Ctrl Pts',(-3.76656457427738,-2.38828969174785,
4.36707247744754));
#14520=CARTESIAN_POINT('Ctrl Pts',(-3.76595694000634,-2.38251974073322,
4.36668273434082));
#14521=CARTESIAN_POINT('Ctrl Pts',(-3.76018123887082,-2.32767505172373,
4.36297813798855));
#14522=CARTESIAN_POINT('Ctrl Pts',(-3.72453483587179,-2.27597349778246,
4.35927354163629));
#14523=CARTESIAN_POINT('Ctrl Pts',(-3.675321975809,-2.25108560394313,4.35556894528402));
#14524=CARTESIAN_POINT('Ctrl Pts',(-3.6261091157462,-2.22619771010379,4.35186434893175));
#14525=CARTESIAN_POINT('Ctrl Pts',(-3.56332979861965,-2.22812347636638,
4.34815975257948));
#14526=CARTESIAN_POINT('Ctrl Pts',(-3.51573443717815,-2.25596350777206,
4.34445515622722));
#14527=CARTESIAN_POINT('Ctrl Pts',(-3.46813907573665,-2.28380353917775,
4.34075055987495));
#14528=CARTESIAN_POINT('Ctrl Pts',(-3.43572766998022,-2.33755783572652,
4.33704596352268));
#14529=CARTESIAN_POINT('Ctrl Pts',(-3.43329506857802,-2.39266164758784,
4.33334136717041));
#14530=CARTESIAN_POINT('Ctrl Pts',(-3.43086246717583,-2.44776545944916,
4.32963677081814));
#14531=CARTESIAN_POINT('Ctrl Pts',(-3.45840867012789,-2.50421878662303,
4.32593217446588));
#14532=CARTESIAN_POINT('Ctrl Pts',(-3.5034058713341,-2.53611223252088,4.32222757811361));
#14533=CARTESIAN_POINT('Ctrl Pts',(-3.5484030725403,-2.56800567841873,4.31852298176134));
#14534=CARTESIAN_POINT('Ctrl Pts',(-3.61085127200066,-2.57533924304056,
4.31481838540907));
#14535=CARTESIAN_POINT('Ctrl Pts',(-3.66197494402253,-2.55491156986817,
4.3111137890568));
#14536=CARTESIAN_POINT('Ctrl Pts',(-3.7130986160444,-2.53448389669578,4.30740919270454));
#14537=CARTESIAN_POINT('Ctrl Pts',(-3.75289776062778,-2.48629498572916,
4.30370459635227));
#14538=CARTESIAN_POINT('Ctrl Pts',(-3.76351293272515,-2.4319230454628,4.3));
#14539=CARTESIAN_POINT('',(-3.60525667617797,-2.23318013248672,4.3));
#14540=CARTESIAN_POINT('Origin',(-3.6,-2.4,4.3));
#14541=CARTESIAN_POINT('',(-3.766345497777,-2.40006497186855,4.31714803633902));
#14542=CARTESIAN_POINT('Ctrl Pts',(-3.60525667255608,-2.23317994016621,
4.3));
#14543=CARTESIAN_POINT('Ctrl Pts',(-3.65930633468078,-2.23495318766097,
4.30363229181855));
#14544=CARTESIAN_POINT('Ctrl Pts',(-3.71251718041942,-2.26542183293127,
4.30726458363711));
#14545=CARTESIAN_POINT('Ctrl Pts',(-3.74128612006692,-2.31121589839408,
4.31089687545566));
#14546=CARTESIAN_POINT('Ctrl Pts',(-3.75778986656855,-2.33748637123519,
4.31298059575011));
#14547=CARTESIAN_POINT('Ctrl Pts',(-3.76624997632687,-2.36880031787527,
4.31506431604457));
#14548=CARTESIAN_POINT('Ctrl Pts',(-3.766345497777,-2.40006497186855,4.31714803633902));
#14549=CARTESIAN_POINT('',(-3.7666,-2.4,4.2));
#14550=CARTESIAN_POINT('',(-3.7666,-2.4,4.7));
#14551=CARTESIAN_POINT('Origin',(-3.6,-2.4,4.2));
#14552=CARTESIAN_POINT('Ctrl Pts',(-3.766345497777,-2.40006497186855,4.31714803633902));
#14553=CARTESIAN_POINT('Ctrl Pts',(-3.76641980162283,-2.42438499660917,
4.31876891239684));
#14554=CARTESIAN_POINT('Ctrl Pts',(-3.76143276745508,-2.44867519480749,
4.32038978845465));
#14555=CARTESIAN_POINT('Ctrl Pts',(-3.75123332790854,-2.47053847327949,
4.32201066451247));
#14556=CARTESIAN_POINT('Ctrl Pts',(-3.72792197948242,-2.52050813091336,
4.32571526086474));
#14557=CARTESIAN_POINT('Ctrl Pts',(-3.67738234157418,-2.55780017273342,
4.329419857217));
#14558=CARTESIAN_POINT('Ctrl Pts',(-3.6227496090289,-2.56532196535192,4.33312445356927));
#14559=CARTESIAN_POINT('Ctrl Pts',(-3.56811687648362,-2.57284375797042,
4.33682904992154));
#14560=CARTESIAN_POINT('Ctrl Pts',(-3.5093910493013,-2.55059530138736,4.34053364627381));
#14561=CARTESIAN_POINT('Ctrl Pts',(-3.47344562081921,-2.50877156715293,
4.34423824262608));
#14562=CARTESIAN_POINT('Ctrl Pts',(-3.43750019233712,-2.4669478329185,4.34794283897835));
#14563=CARTESIAN_POINT('Ctrl Pts',(-3.42433516255526,-2.40554882103269,
4.35164743533061));
#14564=CARTESIAN_POINT('Ctrl Pts',(-3.4399769373371,-2.35266772584057,4.35535203168288));
#14565=CARTESIAN_POINT('Ctrl Pts',(-3.45561871211893,-2.29978663064845,
4.35905662803515));
#14566=CARTESIAN_POINT('Ctrl Pts',(-3.50006729146445,-2.25542345215002,
4.36276122438742));
#14567=CARTESIAN_POINT('Ctrl Pts',(-3.55297985415763,-2.23988445249497,
4.36646582073969));
#14568=CARTESIAN_POINT('Ctrl Pts',(-3.60589241685081,-2.22434545283993,
4.37017041709195));
#14569=CARTESIAN_POINT('Ctrl Pts',(-3.66726896289165,-2.23763063202826,
4.37387501344422));
#14570=CARTESIAN_POINT('Ctrl Pts',(-3.70902050597011,-2.2736583534049,4.37757960979649));
#14571=CARTESIAN_POINT('Ctrl Pts',(-3.74496653400264,-2.3046764520682,4.38076908531067));
#14572=CARTESIAN_POINT('Ctrl Pts',(-3.76636579491573,-2.35255215149476,
4.38395856082485));
#14573=CARTESIAN_POINT('Ctrl Pts',(-3.76675587540948,-2.40012144305632,
4.38714803633902));
#14574=CARTESIAN_POINT('Origin',(-3.6,-2.4,4.7));
#14575=CARTESIAN_POINT('',(-3.76672469163696,-2.39986752250016,4.45714803633902));
#14576=CARTESIAN_POINT('',(-3.76637108132843,-2.3999167674636,4.43785196366098));
#14577=CARTESIAN_POINT('',(-3.7666,-2.4,4.7));
#14578=CARTESIAN_POINT('Ctrl Pts',(-3.76637108132843,-2.3999167674636,4.43785196366098));
#14579=CARTESIAN_POINT('Ctrl Pts',(-3.76647256500337,-2.37748041616576,
4.43635646533454));
#14580=CARTESIAN_POINT('Ctrl Pts',(-3.7622516281058,-2.3550806593951,4.43486096700809));
#14581=CARTESIAN_POINT('Ctrl Pts',(-3.7535269013147,-2.3345994559913,4.43336546868165));
#14582=CARTESIAN_POINT('Ctrl Pts',(-3.73191431207048,-2.28386413246858,
4.42966087232938));
#14583=CARTESIAN_POINT('Ctrl Pts',(-3.68266490417161,-2.24490171859149,
4.42595627597712));
#14584=CARTESIAN_POINT('Ctrl Pts',(-3.62831780053848,-2.23554372384707,
4.42225167962485));
#14585=CARTESIAN_POINT('Ctrl Pts',(-3.57397069690535,-2.22618572910265,
4.41854708327258));
#14586=CARTESIAN_POINT('Ctrl Pts',(-3.51452589753796,-2.2464321534909,4.41484248692031));
#14587=CARTESIAN_POINT('Ctrl Pts',(-3.47718894803579,-2.28701682605767,
4.41113789056804));
#14588=CARTESIAN_POINT('Ctrl Pts',(-3.43985199853362,-2.32760149862444,
4.40743329421577));
#14589=CARTESIAN_POINT('Ctrl Pts',(-3.42462289889666,-2.38852441936972,
4.40372869786351));
#14590=CARTESIAN_POINT('Ctrl Pts',(-3.4384707400222,-2.441904428893,4.40002410151124));
#14591=CARTESIAN_POINT('Ctrl Pts',(-3.45231858114774,-2.49528443841629,
4.39631950515897));
#14592=CARTESIAN_POINT('Ctrl Pts',(-3.49524336303579,-2.54112153671759,
4.3926149088067));
#14593=CARTESIAN_POINT('Ctrl Pts',(-3.54760150310682,-2.55843699301478,
4.38891031245443));
#14594=CARTESIAN_POINT('Ctrl Pts',(-3.59995964317784,-2.57575244931197,
4.38520571610217));
#14595=CARTESIAN_POINT('Ctrl Pts',(-3.66175114143183,-2.56454626360505,
4.3815011197499));
#14596=CARTESIAN_POINT('Ctrl Pts',(-3.70469439092283,-2.52994925871274,
4.37779652339763));
#14597=CARTESIAN_POINT('Ctrl Pts',(-3.74311978370889,-2.49899204150246,
4.37448167015208));
#14598=CARTESIAN_POINT('Ctrl Pts',(-3.76645418313973,-2.44930678746824,
4.37116681690653));
#14599=CARTESIAN_POINT('Ctrl Pts',(-3.76680083731002,-2.3999030629831,4.36785196366098));
#14600=CARTESIAN_POINT('Ctrl Pts',(-3.76675587540948,-2.40012144305632,
4.38714803633902));
#14601=CARTESIAN_POINT('Ctrl Pts',(-3.76681887592163,-2.40780419002449,
4.38766315717712));
#14602=CARTESIAN_POINT('Ctrl Pts',(-3.76633386603033,-2.41547894454867,
4.38817827801521));
#14603=CARTESIAN_POINT('Ctrl Pts',(-3.76527362096253,-2.42307339831024,
4.3886933988533));
#14604=CARTESIAN_POINT('Ctrl Pts',(-3.75764865276043,-2.47769045827401,
4.39239799520556));
#14605=CARTESIAN_POINT('Ctrl Pts',(-3.72027217624014,-2.52815431463659,
4.39610259155783));
#14606=CARTESIAN_POINT('Ctrl Pts',(-3.67024983212249,-2.55136949856929,
4.3998071879101));
#14607=CARTESIAN_POINT('Ctrl Pts',(-3.62022748800484,-2.57458468250198,
4.40351178426236));
#14608=CARTESIAN_POINT('Ctrl Pts',(-3.55755927628983,-2.57055119400479,
4.40721638061464));
#14609=CARTESIAN_POINT('Ctrl Pts',(-3.51092561732084,-2.54111518112976,
4.4109209769669));
#14610=CARTESIAN_POINT('Ctrl Pts',(-3.46429195835185,-2.51167916825472,
4.41462557331917));
#14611=CARTESIAN_POINT('Ctrl Pts',(-3.43369285212889,-2.45684063100183,
4.41833016967144));
#14612=CARTESIAN_POINT('Ctrl Pts',(-3.433132174149,-2.40169663743424,4.4220347660237));
#14613=CARTESIAN_POINT('Ctrl Pts',(-3.4325714961691,-2.34655264386664,4.42573936237597));
#14614=CARTESIAN_POINT('Ctrl Pts',(-3.46204924643229,-2.29110319398435,
4.42944395872824));
#14615=CARTESIAN_POINT('Ctrl Pts',(-3.50807475488023,-2.26072509261964,
4.43314855508051));
#14616=CARTESIAN_POINT('Ctrl Pts',(-3.55410026332817,-2.23034699125494,
4.43685315143278));
#14617=CARTESIAN_POINT('Ctrl Pts',(-3.61667352996086,-2.22504023840783,
4.44055774778505));
#14618=CARTESIAN_POINT('Ctrl Pts',(-3.66715754973313,-2.24723347480277,
4.44426234413731));
#14619=CARTESIAN_POINT('Ctrl Pts',(-3.71764156950539,-2.26942671119771,
4.44796694048958));
#14620=CARTESIAN_POINT('Ctrl Pts',(-3.75603634241723,-2.3191199368347,4.45167153684185));
#14621=CARTESIAN_POINT('Ctrl Pts',(-3.76477028031358,-2.37357077761011,
4.45537613319412));
#14622=CARTESIAN_POINT('Ctrl Pts',(-3.76616275698799,-2.38225203073804,
4.45596676757575));
#14623=CARTESIAN_POINT('Ctrl Pts',(-3.76680128976178,-2.39105421690488,
4.45655740195739));
#14624=CARTESIAN_POINT('Ctrl Pts',(-3.76672469163696,-2.39986752250016,
4.45714803633902));
#14625=CARTESIAN_POINT('Origin',(-3.6,-2.4,4.7));
#14626=CARTESIAN_POINT('',(-3.76633791767176,-2.39996197521538,4.52714803633902));
#14627=CARTESIAN_POINT('',(-3.76649857915956,-2.40014312937522,4.50785196366098));
#14628=CARTESIAN_POINT('',(-3.7666,-2.4,4.7));
#14629=CARTESIAN_POINT('Ctrl Pts',(-3.76649857915956,-2.40014312937522,
4.50785196366098));
#14630=CARTESIAN_POINT('Ctrl Pts',(-3.76617946285532,-2.36119271347016,
4.50525071011481));
#14631=CARTESIAN_POINT('Ctrl Pts',(-3.75254367029535,-2.32204100961925,
4.50264945656865));
#14632=CARTESIAN_POINT('Ctrl Pts',(-3.7275842614224,-2.29243603978678,4.50004820302248));
#14633=CARTESIAN_POINT('Ctrl Pts',(-3.69203811667935,-2.25027388169498,
4.49634360667021));
#14634=CARTESIAN_POINT('Ctrl Pts',(-3.63352511503972,-2.22747466102272,
4.49263901031794));
#14635=CARTESIAN_POINT('Ctrl Pts',(-3.57882406120147,-2.23447257256027,
4.48893441396567));
#14636=CARTESIAN_POINT('Ctrl Pts',(-3.52412300736323,-2.24147048409781,
4.4852298176134));
#14637=CARTESIAN_POINT('Ctrl Pts',(-3.47323390132638,-2.27826552784516,
4.48152522126114));
#14638=CARTESIAN_POINT('Ctrl Pts',(-3.44944643562249,-2.32801823904553,
4.47782062490887));
#14639=CARTESIAN_POINT('Ctrl Pts',(-3.42565896991859,-2.37777095024589,
4.4741160285566));
#14640=CARTESIAN_POINT('Ctrl Pts',(-3.42897314454765,-2.44048132889927,
4.47041143220433));
#14641=CARTESIAN_POINT('Ctrl Pts',(-3.45787219950101,-2.4874496233209,4.46670683585206));
#14642=CARTESIAN_POINT('Ctrl Pts',(-3.48677125445436,-2.53441791774253,
4.46300223949979));
#14643=CARTESIAN_POINT('Ctrl Pts',(-3.54125518973201,-2.56564412793241,
4.45929764314753));
#14644=CARTESIAN_POINT('Ctrl Pts',(-3.59638914182557,-2.56683738431542,
4.45559304679526));
#14645=CARTESIAN_POINT('Ctrl Pts',(-3.65152309391912,-2.56803064069842,
4.45188845044299));
#14646=CARTESIAN_POINT('Ctrl Pts',(-3.7073070628286,-2.53919094327454,4.44818385409072));
#14647=CARTESIAN_POINT('Ctrl Pts',(-3.73821116198855,-2.49351697797843,
4.44447925773846));
#14648=CARTESIAN_POINT('Ctrl Pts',(-3.75663967023947,-2.4662810102851,4.44227015971263));
#14649=CARTESIAN_POINT('Ctrl Pts',(-3.76622117317942,-2.43305896393576,
4.4400610616868));
#14650=CARTESIAN_POINT('Ctrl Pts',(-3.76637108132843,-2.3999167674636,4.43785196366098));
#14651=CARTESIAN_POINT('Ctrl Pts',(-3.76672469163696,-2.39986752250016,
4.45714803633902));
#14652=CARTESIAN_POINT('Ctrl Pts',(-3.76632084848944,-2.44633332149978,
4.46026199830965));
#14653=CARTESIAN_POINT('Ctrl Pts',(-3.74603891301781,-2.49310820101244,
4.46337596028029));
#14654=CARTESIAN_POINT('Ctrl Pts',(-3.71156690339415,-2.52409905358083,
4.46648992225092));
#14655=CARTESIAN_POINT('Ctrl Pts',(-3.67055648569751,-2.56096803286229,
4.47019451860319));
#14656=CARTESIAN_POINT('Ctrl Pts',(-3.60946254742337,-2.57549753551134,
4.47389911495546));
#14657=CARTESIAN_POINT('Ctrl Pts',(-3.55624507519594,-2.56103805534263,
4.47760371130773));
#14658=CARTESIAN_POINT('Ctrl Pts',(-3.5030276029685,-2.54657857517392,4.48130830765999));
#14659=CARTESIAN_POINT('Ctrl Pts',(-3.45768659678778,-2.50313011218745,
4.48501290401226));
#14660=CARTESIAN_POINT('Ctrl Pts',(-3.44097262555956,-2.45057710029542,
4.48871750036453));
#14661=CARTESIAN_POINT('Ctrl Pts',(-3.42425865433133,-2.39802408840339,
4.4924220967168));
#14662=CARTESIAN_POINT('Ctrl Pts',(-3.43617171805559,-2.33636652760581,
4.49612669306907));
#14663=CARTESIAN_POINT('Ctrl Pts',(-3.47125973540437,-2.29382235099447,
4.49983128942134));
#14664=CARTESIAN_POINT('Ctrl Pts',(-3.50634775275315,-2.25127817438312,
4.5035358857736));
#14665=CARTESIAN_POINT('Ctrl Pts',(-3.56461072372645,-2.22784738195801,
4.50724048212587));
#14666=CARTESIAN_POINT('Ctrl Pts',(-3.61938426936618,-2.23425320834927,
4.51094507847814));
#14667=CARTESIAN_POINT('Ctrl Pts',(-3.67415781500591,-2.24065903474052,
4.51464967483041));
#14668=CARTESIAN_POINT('Ctrl Pts',(-3.72544193531206,-2.27690147994813,
4.51835427118268));
#14669=CARTESIAN_POINT('Ctrl Pts',(-3.74976616178516,-2.3263939836064,4.52205886753495));
#14670=CARTESIAN_POINT('Ctrl Pts',(-3.76090458576616,-2.34905733490504,
4.52375525713631));
#14671=CARTESIAN_POINT('Ctrl Pts',(-3.76638989772718,-2.37449903782319,
4.52545164673766));
#14672=CARTESIAN_POINT('Ctrl Pts',(-3.76633791767176,-2.39996197521538,
4.52714803633902));
#14673=CARTESIAN_POINT('Origin',(-3.6,-2.4,4.7));
#14674=CARTESIAN_POINT('',(-3.7665852438883,-2.4001523433009,4.59714803633902));
#14675=CARTESIAN_POINT('',(-3.76687644757351,-2.39999932887962,4.57785196366098));
#14676=CARTESIAN_POINT('',(-3.7666,-2.4,4.7));
#14677=CARTESIAN_POINT('Ctrl Pts',(-3.76687644620932,-2.39999932888293,
4.57785196366098));
#14678=CARTESIAN_POINT('Ctrl Pts',(-3.76687974213825,-2.34481655618538,
4.57414495489509));
#14679=CARTESIAN_POINT('Ctrl Pts',(-3.73679498392134,-2.28963687265016,
4.57043794612919));
#14680=CARTESIAN_POINT('Ctrl Pts',(-3.69041339984634,-2.25973893422683,
4.5667309373633));
#14681=CARTESIAN_POINT('Ctrl Pts',(-3.64406199955899,-2.22986045251336,
4.56302634101103));
#14682=CARTESIAN_POINT('Ctrl Pts',(-3.58143498915818,-2.22523082136041,
4.55932174465877));
#14683=CARTESIAN_POINT('Ctrl Pts',(-3.53119397503756,-2.24796881775056,
4.5556171483065));
#14684=CARTESIAN_POINT('Ctrl Pts',(-3.48095296091694,-2.27070681414072,
4.55191255195423));
#14685=CARTESIAN_POINT('Ctrl Pts',(-3.44309794307651,-2.32081243807398,
4.54820795560196));
#14686=CARTESIAN_POINT('Ctrl Pts',(-3.43495348515474,-2.3753545665717,4.54450335924969));
#14687=CARTESIAN_POINT('Ctrl Pts',(-3.42680902723298,-2.42989669506942,
4.54079876289742));
#14688=CARTESIAN_POINT('Ctrl Pts',(-3.44837512922987,-2.4888753281316,4.53709416654516));
#14689=CARTESIAN_POINT('Ctrl Pts',(-3.48978194213576,-2.52529856004066,
4.53338957019289));
#14690=CARTESIAN_POINT('Ctrl Pts',(-3.53118875504166,-2.56172179194972,
4.52968497384062));
#14691=CARTESIAN_POINT('Ctrl Pts',(-3.59243627885656,-2.57558962270566,
4.52598037748835));
#14692=CARTESIAN_POINT('Ctrl Pts',(-3.64549423729516,-2.5605553606569,4.52227578113609));
#14693=CARTESIAN_POINT('Ctrl Pts',(-3.69855219573377,-2.54552109860814,
4.51857118478382));
#14694=CARTESIAN_POINT('Ctrl Pts',(-3.74342058879608,-2.50158474375469,
4.51486658843155));
#14695=CARTESIAN_POINT('Ctrl Pts',(-3.759565141404,-2.4488540185723,4.51116199207928));
#14696=CARTESIAN_POINT('Ctrl Pts',(-3.76437348603424,-2.43314918577593,
4.51005864927318));
#14697=CARTESIAN_POINT('Ctrl Pts',(-3.76663393493028,-2.41666426444364,
4.50895530646708));
#14698=CARTESIAN_POINT('Ctrl Pts',(-3.76649857915956,-2.40014312937522,
4.50785196366098));
#14699=CARTESIAN_POINT('Ctrl Pts',(-3.76633791767176,-2.39996197521538,
4.52714803633902));
#14700=CARTESIAN_POINT('Ctrl Pts',(-3.76627638304661,-2.43010531182154,
4.52915624308993));
#14701=CARTESIAN_POINT('Ctrl Pts',(-3.75845482433377,-2.46027840666142,
4.53116444984084));
#14702=CARTESIAN_POINT('Ctrl Pts',(-3.74306538783811,-2.48590718051351,
4.53317265659175));
#14703=CARTESIAN_POINT('Ctrl Pts',(-3.71467605477792,-2.53318531165342,
4.53687725294402));
#14704=CARTESIAN_POINT('Ctrl Pts',(-3.66053305601751,-2.56499901182434,
4.54058184929628));
#14705=CARTESIAN_POINT('Ctrl Pts',(-3.60541524194112,-2.56678856079501,
4.54428644564855));
#14706=CARTESIAN_POINT('Ctrl Pts',(-3.55029742786473,-2.56857810976569,
4.54799104200082));
#14707=CARTESIAN_POINT('Ctrl Pts',(-3.49420479847236,-2.54034350753613,
4.55169563835309));
#14708=CARTESIAN_POINT('Ctrl Pts',(-3.46280846367734,-2.49500647989383,
4.55540023470536));
#14709=CARTESIAN_POINT('Ctrl Pts',(-3.43141212888233,-2.44966945225154,
4.55910483105763));
#14710=CARTESIAN_POINT('Ctrl Pts',(-3.42471208868465,-2.38722999919651,
4.56280942740989));
#14711=CARTESIAN_POINT('Ctrl Pts',(-3.44577465447007,-2.33626389048712,
4.56651402376216));
#14712=CARTESIAN_POINT('Ctrl Pts',(-3.46683722025548,-2.28529778177773,
4.57021862011443));
#14713=CARTESIAN_POINT('Ctrl Pts',(-3.515662392024,-2.24580501741397,4.5739232164667));
#14714=CARTESIAN_POINT('Ctrl Pts',(-3.56990505305945,-2.23585968494016,
4.57762781281897));
#14715=CARTESIAN_POINT('Ctrl Pts',(-3.62414771409491,-2.22591435246634,
4.58133240917123));
#14716=CARTESIAN_POINT('Ctrl Pts',(-3.68380786439731,-2.24551645188247,
4.5850370055235));
#14717=CARTESIAN_POINT('Ctrl Pts',(-3.72158169788407,-2.28569497124226,
4.58874160187577));
#14718=CARTESIAN_POINT('Ctrl Pts',(-3.75015370460556,-2.31608587465984,
4.59154374669686));
#14719=CARTESIAN_POINT('Ctrl Pts',(-3.76620375900909,-2.35824929108539,
4.59434589151794));
#14720=CARTESIAN_POINT('Ctrl Pts',(-3.7665852438883,-2.4001523433009,4.59714803633902));
#14721=CARTESIAN_POINT('Origin',(-3.6,-2.4,4.7));
#14722=CARTESIAN_POINT('',(-3.76685427080137,-2.39994496470643,4.66714803633902));
#14723=CARTESIAN_POINT('',(-3.76649662121988,-2.39985729252779,4.64785196366098));
#14724=CARTESIAN_POINT('',(-3.7666,-2.4,4.7));
#14725=CARTESIAN_POINT('Ctrl Pts',(-3.76649662121988,-2.39985729252779,
4.64785196366098));
#14726=CARTESIAN_POINT('Ctrl Pts',(-3.76663205173418,-2.38326341802857,
4.64674379602763));
#14727=CARTESIAN_POINT('Ctrl Pts',(-3.76435139460867,-2.36670593234144,
4.64563562839428));
#14728=CARTESIAN_POINT('Ctrl Pts',(-3.7595015341574,-2.35093871131677,4.64452746076093));
#14729=CARTESIAN_POINT('Ctrl Pts',(-3.74328848588199,-2.29822900591163,
4.64082286440866));
#14730=CARTESIAN_POINT('Ctrl Pts',(-3.69836304774957,-2.25435098262799,
4.63711826805639));
#14731=CARTESIAN_POINT('Ctrl Pts',(-3.64528560126629,-2.23938566762668,
4.63341367170413));
#14732=CARTESIAN_POINT('Ctrl Pts',(-3.59220815478301,-2.22442035262536,
4.62970907535186));
#14733=CARTESIAN_POINT('Ctrl Pts',(-3.53097869994887,-2.23836774590636,
4.62600447899959));
#14734=CARTESIAN_POINT('Ctrl Pts',(-3.48961924396277,-2.27484474384805,
4.62229988264732));
#14735=CARTESIAN_POINT('Ctrl Pts',(-3.44825978797668,-2.31132174178974,
4.61859528629506));
#14736=CARTESIAN_POINT('Ctrl Pts',(-3.42677033083864,-2.37032834439211,
4.61489068994278));
#14737=CARTESIAN_POINT('Ctrl Pts',(-3.43498564446249,-2.42485984538296,
4.61118609359052));
#14738=CARTESIAN_POINT('Ctrl Pts',(-3.44320095808634,-2.47939134637381,
4.60748149723825));
#14739=CARTESIAN_POINT('Ctrl Pts',(-3.48112104247208,-2.52944774575313,
4.60377690088598));
#14740=CARTESIAN_POINT('Ctrl Pts',(-3.53139155597687,-2.55212044850799,
4.60007230453371));
#14741=CARTESIAN_POINT('Ctrl Pts',(-3.58166206948165,-2.57479315126284,
4.59636770818145));
#14742=CARTESIAN_POINT('Ctrl Pts',(-3.64428301210547,-2.57008215739322,
4.59266311182917));
#14743=CARTESIAN_POINT('Ctrl Pts',(-3.69059555437608,-2.54014347995252,
4.58895851547691));
#14744=CARTESIAN_POINT('Ctrl Pts',(-3.73687793816318,-2.51022429842083,
4.58525633153826));
#14745=CARTESIAN_POINT('Ctrl Pts',(-3.76687315457017,-2.45511027888938,
4.58155414759962));
#14746=CARTESIAN_POINT('Ctrl Pts',(-3.76687644620932,-2.39999932888293,
4.57785196366098));
#14747=CARTESIAN_POINT('Ctrl Pts',(-3.7665852438883,-2.4001523433009,4.59714803633902));
#14748=CARTESIAN_POINT('Ctrl Pts',(-3.76670810392422,-2.41364753218216,
4.59805048787021));
#14749=CARTESIAN_POINT('Ctrl Pts',(-3.76520580454733,-2.42711571583196,
4.59895293940139));
#14750=CARTESIAN_POINT('Ctrl Pts',(-3.76197323580484,-2.44015494667501,
4.59985539093257));
#14751=CARTESIAN_POINT('Ctrl Pts',(-3.74870342356775,-2.49368146344449,
4.60355998728484));
#14752=CARTESIAN_POINT('Ctrl Pts',(-3.70627628242244,-2.53997955767999,
4.60726458363711));
#14753=CARTESIAN_POINT('Ctrl Pts',(-3.65410883409218,-2.55786064402731,
4.61096917998938));
#14754=CARTESIAN_POINT('Ctrl Pts',(-3.60194138576191,-2.57574173037463,
4.61467377634165));
#14755=CARTESIAN_POINT('Ctrl Pts',(-3.54003363024668,-2.56520580883379,
4.61837837269391));
#14756=CARTESIAN_POINT('Ctrl Pts',(-3.49671800289895,-2.53107470364031,
4.62208296904618));
#14757=CARTESIAN_POINT('Ctrl Pts',(-3.45340237555123,-2.49694359844684,
4.62578756539845));
#14758=CARTESIAN_POINT('Ctrl Pts',(-3.42867887637101,-2.43921730960073,
4.62949216175072));
#14759=CARTESIAN_POINT('Ctrl Pts',(-3.43386235494986,-2.38431460052291,
4.63319675810299));
#14760=CARTESIAN_POINT('Ctrl Pts',(-3.43904583352872,-2.3294118914451,4.63690135445526));
#14761=CARTESIAN_POINT('Ctrl Pts',(-3.47413628986665,-2.27733276213558,
4.64060595080752));
#14762=CARTESIAN_POINT('Ctrl Pts',(-3.52307437764419,-2.25191152143151,
4.64431054715979));
#14763=CARTESIAN_POINT('Ctrl Pts',(-3.57201246542174,-2.22649028072744,
4.64801514351206));
#14764=CARTESIAN_POINT('Ctrl Pts',(-3.6347981846389,-2.22772692862883,4.65171973986433));
#14765=CARTESIAN_POINT('Ctrl Pts',(-3.68269729487669,-2.25505550621137,
4.65542433621659));
#14766=CARTESIAN_POINT('Ctrl Pts',(-3.73059640511449,-2.28238408379392,
4.65912893256886));
#14767=CARTESIAN_POINT('Ctrl Pts',(-3.76360890637291,-2.33580459105762,
4.66283352892113));
#14768=CARTESIAN_POINT('Ctrl Pts',(-3.76662644025744,-2.39086882993835,
4.6665381252734));
#14769=CARTESIAN_POINT('Ctrl Pts',(-3.76679203880333,-2.3938906876002,4.66674142896194));
#14770=CARTESIAN_POINT('Ctrl Pts',(-3.76686730212629,-2.39691749565456,
4.66694473265048));
#14771=CARTESIAN_POINT('Ctrl Pts',(-3.76685427080137,-2.39994496470643,
4.66714803633902));
#14772=CARTESIAN_POINT('Origin',(-3.6,-2.4,4.7));
#14773=CARTESIAN_POINT('',(-3.7664227625968,-2.39988235338239,4.73714803633902));
#14774=CARTESIAN_POINT('',(-3.76637219995946,-2.40008425137793,4.71785196366098));
#14775=CARTESIAN_POINT('',(-3.7666,-2.4,4.7));
#14776=CARTESIAN_POINT('Ctrl Pts',(-3.76637219995946,-2.40008425137793,
4.71785196366098));
#14777=CARTESIAN_POINT('Ctrl Pts',(-3.76622009461901,-2.36687021016323,
4.7156380408079));
#14778=CARTESIAN_POINT('Ctrl Pts',(-3.7565937463241,-2.33357496437374,4.71342411795483));
#14779=CARTESIAN_POINT('Ctrl Pts',(-3.73808953535598,-2.30630352370031,
4.71121019510175));
#14780=CARTESIAN_POINT('Ctrl Pts',(-3.70712611115225,-2.26066973862981,
4.70750559874949));
#14781=CARTESIAN_POINT('Ctrl Pts',(-3.65130474062691,-2.23190256095558,
4.70380100239722));
#14782=CARTESIAN_POINT('Ctrl Pts',(-3.5961723905296,-2.23316745266121,4.70009640604495));
#14783=CARTESIAN_POINT('Ctrl Pts',(-3.54104004043228,-2.23443234436684,
4.69639180969269));
#14784=CARTESIAN_POINT('Ctrl Pts',(-3.48659671076299,-2.26572930545233,
4.69268721334042));
#14785=CARTESIAN_POINT('Ctrl Pts',(-3.45775870005953,-2.31273510421107,
4.68898261698815));
#14786=CARTESIAN_POINT('Ctrl Pts',(-3.42892068935607,-2.35974090296982,
4.68527802063588));
#14787=CARTESIAN_POINT('Ctrl Pts',(-3.42568799761845,-2.42245553940182,
4.68157342428361));
#14788=CARTESIAN_POINT('Ctrl Pts',(-3.44954008455102,-2.47217730452778,
4.67786882793134));
#14789=CARTESIAN_POINT('Ctrl Pts',(-3.47339217148359,-2.52189906965374,
4.67416423157907));
#14790=CARTESIAN_POINT('Ctrl Pts',(-3.52432903708635,-2.55862796347366,
4.6704596352268));
#14791=CARTESIAN_POINT('Ctrl Pts',(-3.57903913598448,-2.56555479946389,
4.66675503887454));
#14792=CARTESIAN_POINT('Ctrl Pts',(-3.63374923488261,-2.57248163545412,
4.66305044252227));
#14793=CARTESIAN_POINT('Ctrl Pts',(-3.69223256707613,-2.54960641361466,
4.65934584617));
#14794=CARTESIAN_POINT('Ctrl Pts',(-3.72772390396368,-2.50739810893161,
4.65564124981774));
#14795=CARTESIAN_POINT('Ctrl Pts',(-3.75259860490409,-2.47781570803419,
4.65304482109882));
#14796=CARTESIAN_POINT('Ctrl Pts',(-3.76617930850818,-2.43873661999706,
4.6504483923799));
#14797=CARTESIAN_POINT('Ctrl Pts',(-3.76649662121988,-2.39985729252779,
4.64785196366098));
#14798=CARTESIAN_POINT('Ctrl Pts',(-3.76685427080137,-2.39994496470643,
4.66714803633902));
#14799=CARTESIAN_POINT('Ctrl Pts',(-3.76662984554536,-2.45208398518876,
4.67064932900275));
#14800=CARTESIAN_POINT('Ctrl Pts',(-3.74021751929721,-2.50441905534817,
4.67415062166648));
#14801=CARTESIAN_POINT('Ctrl Pts',(-3.6980405151982,-2.53504001717725,4.6776519143302));
#14802=CARTESIAN_POINT('Ctrl Pts',(-3.65341448974379,-2.56743899503768,
4.68135651068247));
#14803=CARTESIAN_POINT('Ctrl Pts',(-3.59113987232435,-2.57552898026078,
4.68506110703474));
#14804=CARTESIAN_POINT('Ctrl Pts',(-3.53971699472298,-2.55560754523587,
4.68876570338701));
#14805=CARTESIAN_POINT('Ctrl Pts',(-3.48829411712161,-2.53568611021095,
4.69247029973928));
#14806=CARTESIAN_POINT('Ctrl Pts',(-3.4477229793383,-2.48775325493802,4.69617489609154));
#14807=CARTESIAN_POINT('Ctrl Pts',(-3.4365711926336,-2.4337457224305,4.69987949244381));
#14808=CARTESIAN_POINT('Ctrl Pts',(-3.42541940592889,-2.37973818992299,
4.70358408879608));
#14809=CARTESIAN_POINT('Ctrl Pts',(-3.44368697030278,-2.31965598018089,
4.70728868514835));
#14810=CARTESIAN_POINT('Ctrl Pts',(-3.48301363133541,-2.28099605718198,
4.71099328150062));
#14811=CARTESIAN_POINT('Ctrl Pts',(-3.52234029236805,-2.24233613418307,
4.71469787785288));
#14812=CARTESIAN_POINT('Ctrl Pts',(-3.58272605005944,-2.22509849792735,
4.71840247420515));
#14813=CARTESIAN_POINT('Ctrl Pts',(-3.63653501999159,-2.23717205039129,
4.72210707055742));
#14814=CARTESIAN_POINT('Ctrl Pts',(-3.69034398992373,-2.24924560285524,
4.72581166690969));
#14815=CARTESIAN_POINT('Ctrl Pts',(-3.73757617209662,-2.29063034403885,
4.72951626326196));
#14816=CARTESIAN_POINT('Ctrl Pts',(-3.75661549051415,-2.342386312472,4.73322085961422));
#14817=CARTESIAN_POINT('Ctrl Pts',(-3.76334323815838,-2.36067483977454,
4.73452991852249));
#14818=CARTESIAN_POINT('Ctrl Pts',(-3.76655071734768,-2.38025835805218,
4.73583897743076));
#14819=CARTESIAN_POINT('Ctrl Pts',(-3.7664227625968,-2.39988235338239,4.73714803633902));
#14820=CARTESIAN_POINT('Origin',(-3.6,-2.4,4.7));
#14821=CARTESIAN_POINT('',(-3.76642911325459,-2.40012064491874,4.80714803633902));
#14822=CARTESIAN_POINT('',(-3.76680409091049,-2.40009747380892,4.78785196366098));
#14823=CARTESIAN_POINT('',(-3.7666,-2.4,4.7));
#14824=CARTESIAN_POINT('Ctrl Pts',(-3.76680409091049,-2.40009747380892,
4.78785196366098));
#14825=CARTESIAN_POINT('Ctrl Pts',(-3.76646019447366,-2.35062358790434,
4.78453228558818));
#14826=CARTESIAN_POINT('Ctrl Pts',(-3.74304697023447,-2.30086701998663,
4.78121260751538));
#14827=CARTESIAN_POINT('Ctrl Pts',(-3.70452480595454,-2.26991420375009,
4.77789292944258));
#14828=CARTESIAN_POINT('Ctrl Pts',(-3.66153597807928,-2.23537239348787,
4.77418833309031));
#14829=CARTESIAN_POINT('Ctrl Pts',(-3.59973129997326,-2.22424775044289,
4.77048373673805));
#14830=CARTESIAN_POINT('Ctrl Pts',(-3.54739603302806,-2.24163153058572,
4.76677914038578));
#14831=CARTESIAN_POINT('Ctrl Pts',(-3.49506076608285,-2.25901531072854,
4.76307454403351));
#14832=CARTESIAN_POINT('Ctrl Pts',(-3.45219491029846,-2.30490751405916,
4.75936994768124));
#14833=CARTESIAN_POINT('Ctrl Pts',(-3.43841626764055,-2.35830531349683,
4.75566535132897));
#14834=CARTESIAN_POINT('Ctrl Pts',(-3.42463762498264,-2.4117031129345,4.7519607549767));
#14835=CARTESIAN_POINT('Ctrl Pts',(-3.4399461954512,-2.47260650847922,4.74825615862444));
#14836=CARTESIAN_POINT('Ctrl Pts',(-3.47733592496581,-2.51314271581421,
4.74455156227217));
#14837=CARTESIAN_POINT('Ctrl Pts',(-3.51472565448041,-2.55367892314919,
4.7408469659199));
#14838=CARTESIAN_POINT('Ctrl Pts',(-3.57419654304106,-2.57384794227444,
4.73714236956763));
#14839=CARTESIAN_POINT('Ctrl Pts',(-3.62853140127509,-2.56441930722117,
4.73343777321536));
#14840=CARTESIAN_POINT('Ctrl Pts',(-3.68286625950912,-2.55499067216789,
4.7297331768631));
#14841=CARTESIAN_POINT('Ctrl Pts',(-3.73206508741654,-2.5159643829361,4.72602858051083));
#14842=CARTESIAN_POINT('Ctrl Pts',(-3.75361176242918,-2.46520104208683,
4.72232398415856));
#14843=CARTESIAN_POINT('Ctrl Pts',(-3.7622818183227,-2.4447746420856,4.72083331065936));
#14844=CARTESIAN_POINT('Ctrl Pts',(-3.76647461518129,-2.42244785405319,
4.71934263716017));
#14845=CARTESIAN_POINT('Ctrl Pts',(-3.76637219995946,-2.40008425137793,
4.71785196366098));
#14846=CARTESIAN_POINT('Ctrl Pts',(-3.7664227625968,-2.39988235338239,4.73714803633902));
#14847=CARTESIAN_POINT('Ctrl Pts',(-3.76618860934753,-2.43579365983134,
4.73954357378302));
#14848=CARTESIAN_POINT('Ctrl Pts',(-3.75478479773435,-2.47184051531438,
4.74193911122703));
#14849=CARTESIAN_POINT('Ctrl Pts',(-3.73334402642865,-2.50033503613074,
4.74433464867103));
#14850=CARTESIAN_POINT('Ctrl Pts',(-3.70018678926345,-2.54440059567364,
4.7480392450233));
#14851=CARTESIAN_POINT('Ctrl Pts',(-3.64302586027087,-2.57040451907673,
4.75174384137556));
#14852=CARTESIAN_POINT('Ctrl Pts',(-3.58802126272889,-2.56644596334232,
4.75544843772783));
#14853=CARTESIAN_POINT('Ctrl Pts',(-3.53301666518691,-2.56248740760791,
4.7591530340801));
#14854=CARTESIAN_POINT('Ctrl Pts',(-3.48016839909552,-2.52856637273599,
4.76285763043237));
#14855=CARTESIAN_POINT('Ctrl Pts',(-3.4536627731015,-2.48020701268106,4.76656222678464));
#14856=CARTESIAN_POINT('Ctrl Pts',(-3.42715714710748,-2.43184765262612,
4.77026682313691));
#14857=CARTESIAN_POINT('Ctrl Pts',(-3.42699416121083,-2.36904996738817,
4.77397141948918));
#14858=CARTESIAN_POINT('Ctrl Pts',(-3.45324840683133,-2.32055367370344,
4.77767601584144));
#14859=CARTESIAN_POINT('Ctrl Pts',(-3.47950265245184,-2.2720573800187,4.78138061219371));
#14860=CARTESIAN_POINT('Ctrl Pts',(-3.53217412958951,-2.23786247788719,
4.78508520854597));
#14861=CARTESIAN_POINT('Ctrl Pts',(-3.58715743806471,-2.23361845816768,
4.78878980489824));
#14862=CARTESIAN_POINT('Ctrl Pts',(-3.6421407465399,-2.22937443844816,4.79249440125051));
#14863=CARTESIAN_POINT('Ctrl Pts',(-3.69943588635261,-2.25508130114064,
4.79619899760278));
#14864=CARTESIAN_POINT('Ctrl Pts',(-3.73282141188201,-2.29897415476607,
4.79990359395505));
#14865=CARTESIAN_POINT('Ctrl Pts',(-3.75458352333835,-2.32758539144982,
4.80231840808304));
#14866=CARTESIAN_POINT('Ctrl Pts',(-3.76618646552292,-2.36392383602884,
4.80473322221103));
#14867=CARTESIAN_POINT('Ctrl Pts',(-3.76642911325459,-2.40012064491874,
4.80714803633902));
#14868=CARTESIAN_POINT('Origin',(-3.6,-2.4,4.7));
#14869=CARTESIAN_POINT('',(-3.76685810224694,-2.40005005741615,4.87714803633902));
#14870=CARTESIAN_POINT('',(-3.76666750911963,-2.3998541249347,4.85785196366098));
#14871=CARTESIAN_POINT('',(-3.7666,-2.4,4.7));
#14872=CARTESIAN_POINT('Ctrl Pts',(-3.76666750911963,-2.3998541249347,4.85785196366098));
#14873=CARTESIAN_POINT('Ctrl Pts',(-3.76676617376365,-2.38908842257499,
4.85713112672072));
#14874=CARTESIAN_POINT('Ctrl Pts',(-3.76581236816026,-2.37834012863908,
4.85641028978047));
#14875=CARTESIAN_POINT('Ctrl Pts',(-3.76374257749965,-2.36781121686714,
4.85568945284021));
#14876=CARTESIAN_POINT('Ctrl Pts',(-3.75310530504175,-2.31369999425172,
4.85198485648794));
#14877=CARTESIAN_POINT('Ctrl Pts',(-3.71299219872321,-2.26538317916478,
4.84828026013567));
#14878=CARTESIAN_POINT('Ctrl Pts',(-3.66176124910748,-2.24497323600586,
4.8445756637834));
#14879=CARTESIAN_POINT('Ctrl Pts',(-3.61053029949175,-2.22456329284695,
4.84087106743114));
#14880=CARTESIAN_POINT('Ctrl Pts',(-3.54818150657882,-2.23206022161606,
4.83716647107887));
#14881=CARTESIAN_POINT('Ctrl Pts',(-3.50324914898701,-2.26403301035152,
4.8334618747266));
#14882=CARTESIAN_POINT('Ctrl Pts',(-3.45831679139521,-2.29600579908698,
4.82975727837433));
#14883=CARTESIAN_POINT('Ctrl Pts',(-3.43080086912452,-2.35245444778878,
4.82605268202206));
#14884=CARTESIAN_POINT('Ctrl Pts',(-3.43329420002801,-2.40754491229296,
4.82234808566979));
#14885=CARTESIAN_POINT('Ctrl Pts',(-3.43578753093151,-2.46263537679713,
4.81864348931753));
#14886=CARTESIAN_POINT('Ctrl Pts',(-3.4682901150092,-2.51636765710367,4.81493889296526));
#14887=CARTESIAN_POINT('Ctrl Pts',(-3.51592696035573,-2.54415087044753,
4.81123429661299));
#14888=CARTESIAN_POINT('Ctrl Pts',(-3.56356380570226,-2.5719340837914,4.80752970026073));
#14889=CARTESIAN_POINT('Ctrl Pts',(-3.62633491231765,-2.57376823017258,
4.80382510390846));
#14890=CARTESIAN_POINT('Ctrl Pts',(-3.67551272732296,-2.54881390209942,
4.80012050755619));
#14891=CARTESIAN_POINT('Ctrl Pts',(-3.72469054232828,-2.52385957402626,
4.79641591120392));
#14892=CARTESIAN_POINT('Ctrl Pts',(-3.76027506572354,-2.47211677149876,
4.79271131485165));
#14893=CARTESIAN_POINT('Ctrl Pts',(-3.76598083859892,-2.41726588149528,
4.78900671849938));
#14894=CARTESIAN_POINT('Ctrl Pts',(-3.76657368490912,-2.41156671532445,
4.78862180021991));
#14895=CARTESIAN_POINT('Ctrl Pts',(-3.7668439658688,-2.40583399482793,4.78823688194045));
#14896=CARTESIAN_POINT('Ctrl Pts',(-3.76680409091049,-2.40009747380892,
4.78785196366098));
#14897=CARTESIAN_POINT('Ctrl Pts',(-3.76642911325459,-2.40012064491874,
4.80714803633902));
#14898=CARTESIAN_POINT('Ctrl Pts',(-3.76655871442242,-2.41945381020902,
4.8084378185633));
#14899=CARTESIAN_POINT('Ctrl Pts',(-3.76344749532011,-2.43874657022512,
4.80972760078758));
#14900=CARTESIAN_POINT('Ctrl Pts',(-3.75691244110645,-2.45679995321808,
4.81101738301185));
#14901=CARTESIAN_POINT('Ctrl Pts',(-3.73814203355539,-2.50865405348629,
4.81472197936412));
#14902=CARTESIAN_POINT('Ctrl Pts',(-3.69112530720718,-2.55028340946432,
4.81842657571639));
#14903=CARTESIAN_POINT('Ctrl Pts',(-3.63737973347804,-2.56263611033431,
4.82213117206866));
#14904=CARTESIAN_POINT('Ctrl Pts',(-3.58363415974891,-2.5749888112043,4.82583576842093));
#14905=CARTESIAN_POINT('Ctrl Pts',(-3.52315973863885,-2.55806485696625,
4.82954036477319));
#14906=CARTESIAN_POINT('Ctrl Pts',(-3.48363293188217,-2.51960959124259,
4.83324496112546));
#14907=CARTESIAN_POINT('Ctrl Pts',(-3.44410612512549,-2.48115432551893,
4.83694955747773));
#14908=CARTESIAN_POINT('Ctrl Pts',(-3.42552693272221,-2.42116774830966,
4.84065415383));
#14909=CARTESIAN_POINT('Ctrl Pts',(-3.43639822742686,-2.36710305682155,
4.84435875018227));
#14910=CARTESIAN_POINT('Ctrl Pts',(-3.44726952213151,-2.31303836533343,
4.84806334653454));
#14911=CARTESIAN_POINT('Ctrl Pts',(-3.48759130394411,-2.26489555956646,
4.8517679428868));
#14912=CARTESIAN_POINT('Ctrl Pts',(-3.53891008077804,-2.24470746756836,
4.85547253923907));
#14913=CARTESIAN_POINT('Ctrl Pts',(-3.59022885761198,-2.22451937557026,
4.85917713559134));
#14914=CARTESIAN_POINT('Ctrl Pts',(-3.65254462946725,-2.23228599734102,
4.86288173194361));
#14915=CARTESIAN_POINT('Ctrl Pts',(-3.69733822999987,-2.26445289438714,
4.86658632829587));
#14916=CARTESIAN_POINT('Ctrl Pts',(-3.73990669414912,-2.29502189057005,
4.87010689764359));
#14917=CARTESIAN_POINT('Ctrl Pts',(-3.76665058750282,-2.34762719015485,
4.87362746699131));
#14918=CARTESIAN_POINT('Ctrl Pts',(-3.76685810224694,-2.40005005741615,
4.87714803633902));
#14919=CARTESIAN_POINT('Origin',(-3.6,-2.4,4.7));
#14920=CARTESIAN_POINT('',(-3.76657660157387,-2.39984780956506,4.94714803633902));
#14921=CARTESIAN_POINT('',(-3.76633014204238,-2.3999936674641,4.92785196366098));
#14922=CARTESIAN_POINT('',(-3.7666,-2.4,4.7));
#14923=CARTESIAN_POINT('Ctrl Pts',(-3.76633014204238,-2.3999936674641,4.92785196366098));
#14924=CARTESIAN_POINT('Ctrl Pts',(-3.76633943871615,-2.37257318075516,
4.926025371501));
#14925=CARTESIAN_POINT('Ctrl Pts',(-3.75993532676097,-2.34515678209823,
4.92419877934102));
#14926=CARTESIAN_POINT('Ctrl Pts',(-3.74709395990921,-2.32118936363805,
4.92237218718104));
#14927=CARTESIAN_POINT('Ctrl Pts',(-3.72104978768541,-2.27257992966252,
4.91866759082877));
#14928=CARTESIAN_POINT('Ctrl Pts',(-3.66852675339565,-2.23815745462599,
4.9149629944765));
#14929=CARTESIAN_POINT('Ctrl Pts',(-3.61356232150655,-2.23367557941999,
4.91125839812423));
#14930=CARTESIAN_POINT('Ctrl Pts',(-3.55859788961746,-2.22919370421399,
4.90755380177196));
#14931=CARTESIAN_POINT('Ctrl Pts',(-3.50119206012902,-2.25465242883852,
4.90384920541969));
#14932=CARTESIAN_POINT('Ctrl Pts',(-3.4676169364208,-2.2984004236072,4.90014460906743));
#14933=CARTESIAN_POINT('Ctrl Pts',(-3.43404181271257,-2.34214841837589,
4.89644001271516));
#14934=CARTESIAN_POINT('Ctrl Pts',(-3.42429739478456,-2.40418568328873,
4.89273541636289));
#14935=CARTESIAN_POINT('Ctrl Pts',(-3.44284327075563,-2.45612051228373,
4.88903082001062));
#14936=CARTESIAN_POINT('Ctrl Pts',(-3.46138914672669,-2.50805534127872,
4.88532622365836));
#14937=CARTESIAN_POINT('Ctrl Pts',(-3.50822531659685,-2.54988773435588,
4.88162162730609));
#14938=CARTESIAN_POINT('Ctrl Pts',(-3.56191694164611,-2.56247285961735,
4.87791703095382));
#14939=CARTESIAN_POINT('Ctrl Pts',(-3.61560856669538,-2.57505798487881,
4.87421243460155));
#14940=CARTESIAN_POINT('Ctrl Pts',(-3.67615564692375,-2.55839584232458,
4.87050783824928));
#14941=CARTESIAN_POINT('Ctrl Pts',(-3.7158484677393,-2.52011195597552,4.86680324189701));
#14942=CARTESIAN_POINT('Ctrl Pts',(-3.74781789610229,-2.48927731291044,
4.863819482485));
#14943=CARTESIAN_POINT('Ctrl Pts',(-3.76625910668661,-2.44441658275108,
4.86083572307299));
#14944=CARTESIAN_POINT('Ctrl Pts',(-3.76666750911963,-2.3998541249347,4.85785196366098));
#14945=CARTESIAN_POINT('Ctrl Pts',(-3.76685810224694,-2.40005005741615,
4.87714803633902));
#14946=CARTESIAN_POINT('Ctrl Pts',(-3.76686894944607,-2.40279030260928,
4.87733206334357));
#14947=CARTESIAN_POINT('Ctrl Pts',(-3.76680728980785,-2.40553004933232,
4.87751609034813));
#14948=CARTESIAN_POINT('Ctrl Pts',(-3.76667159341225,-2.40826612418172,
4.87770011735268));
#14949=CARTESIAN_POINT('Ctrl Pts',(-3.76393992708203,-2.46334528460871,
4.88140471370495));
#14950=CARTESIAN_POINT('Ctrl Pts',(-3.73120516521163,-2.5169364331412,4.88510931005721));
#14951=CARTESIAN_POINT('Ctrl Pts',(-3.6834485571899,-2.54451327676931,4.88881390640948));
#14952=CARTESIAN_POINT('Ctrl Pts',(-3.63569194916816,-2.57209012039741,
4.89251850276175));
#14953=CARTESIAN_POINT('Ctrl Pts',(-3.57291349499508,-2.57365265912114,
4.89622309911402));
#14954=CARTESIAN_POINT('Ctrl Pts',(-3.52384411020076,-2.5484857882364,4.89992769546629));
#14955=CARTESIAN_POINT('Ctrl Pts',(-3.47477472540644,-2.52331891735167,
4.90363229181856));
#14956=CARTESIAN_POINT('Ctrl Pts',(-3.43941440999087,-2.47142263685848,
4.90733688817082));
#14957=CARTESIAN_POINT('Ctrl Pts',(-3.43394601281114,-2.41654757379038,
4.91104148452309));
#14958=CARTESIAN_POINT('Ctrl Pts',(-3.42847761563141,-2.36167251072229,
4.91474608087536));
#14959=CARTESIAN_POINT('Ctrl Pts',(-3.45290113668751,-2.30381866507929,
4.91845067722763));
#14960=CARTESIAN_POINT('Ctrl Pts',(-3.4960390130763,-2.2694631773857,4.9221552735799));
#14961=CARTESIAN_POINT('Ctrl Pts',(-3.53917688946509,-2.23510768969211,
4.92585986993217));
#14962=CARTESIAN_POINT('Ctrl Pts',(-3.60102912118658,-2.22425055994793,
4.92956446628443));
#14963=CARTESIAN_POINT('Ctrl Pts',(-3.65328868366947,-2.24186061512031,
4.9332690626367));
#14964=CARTESIAN_POINT('Ctrl Pts',(-3.70554824615237,-2.25947067029269,
4.93697365898897));
#14965=CARTESIAN_POINT('Ctrl Pts',(-3.74821513939667,-2.30554791038164,
4.94067825534123));
#14966=CARTESIAN_POINT('Ctrl Pts',(-3.76176261776726,-2.35900482523354,
4.9443828516935));
#14967=CARTESIAN_POINT('Ctrl Pts',(-3.76513332050279,-2.37230526124053,
4.94530457990868));
#14968=CARTESIAN_POINT('Ctrl Pts',(-3.76670139313906,-2.38606253416914,
4.94622630812385));
#14969=CARTESIAN_POINT('Ctrl Pts',(-3.76657660157387,-2.39984780956506,
4.94714803633902));
#14970=CARTESIAN_POINT('Origin',(-3.6,-2.4,4.7));
#14971=CARTESIAN_POINT('',(-3.76634000649331,-2.40004261214866,5.01714803633902));
#14972=CARTESIAN_POINT('',(-3.76664426409402,-2.40014916296054,4.99785196366098));
#14973=CARTESIAN_POINT('',(-3.7666,-2.4,4.7));
#14974=CARTESIAN_POINT('Ctrl Pts',(-3.76664426409402,-2.40014916296054,
4.99785196366098));
#14975=CARTESIAN_POINT('Ctrl Pts',(-3.76623994861442,-2.35633882629306,
4.99491961628127));
#14976=CARTESIAN_POINT('Ctrl Pts',(-3.74849621908403,-2.31223872253049,
4.99198726890157));
#14977=CARTESIAN_POINT('Ctrl Pts',(-3.71750016680111,-2.28150333241251,
4.98905492152186));
#14978=CARTESIAN_POINT('Ctrl Pts',(-3.678341142527,-2.24267361704367,4.98535032516959));
#14979=CARTESIAN_POINT('Ctrl Pts',(-3.61803053121903,-2.22517487203488,
4.98164572881732));
#14980=CARTESIAN_POINT('Ctrl Pts',(-3.56416982600182,-2.23701549741557,
4.97794113246506));
#14981=CARTESIAN_POINT('Ctrl Pts',(-3.51030912078461,-2.24885612279626,
4.97423653611279));
#14982=CARTESIAN_POINT('Ctrl Pts',(-3.46289832165815,-2.29003611856643,
4.97053193976052));
#14983=CARTESIAN_POINT('Ctrl Pts',(-3.44363524974256,-2.34170922607974,
4.96682734340825));
#14984=CARTESIAN_POINT('Ctrl Pts',(-3.42437217782697,-2.39338233359304,
4.96312274705598));
#14985=CARTESIAN_POINT('Ctrl Pts',(-3.43325683312225,-2.45554855284948,
4.95941815070371));
#14986=CARTESIAN_POINT('Ctrl Pts',(-3.46622310272193,-2.4997571611377,4.95571355435145));
#14987=CARTESIAN_POINT('Ctrl Pts',(-3.49918937232162,-2.54396576942592,
4.95200895799918));
#14988=CARTESIAN_POINT('Ctrl Pts',(-3.55623725622572,-2.57021676674591,
4.94830436164691));
#14989=CARTESIAN_POINT('Ctrl Pts',(-3.61125846689758,-2.56649623530203,
4.94459976529464));
#14990=CARTESIAN_POINT('Ctrl Pts',(-3.66627967756944,-2.56277570385816,
4.94089516894238));
#14991=CARTESIAN_POINT('Ctrl Pts',(-3.71927421500904,-2.52908364365041,
4.93719057259011));
#14992=CARTESIAN_POINT('Ctrl Pts',(-3.74598882864993,-2.48083941708926,
4.93348597623784));
#14993=CARTESIAN_POINT('Ctrl Pts',(-3.7595315068913,-2.45638253943781,4.93160797204555));
#14994=CARTESIAN_POINT('Ctrl Pts',(-3.76632058370052,-2.4281859427416,4.92972996785327));
#14995=CARTESIAN_POINT('Ctrl Pts',(-3.76633014204238,-2.3999936674641,4.92785196366098));
#14996=CARTESIAN_POINT('Ctrl Pts',(-3.76657660157387,-2.39984780956506,
4.94714803633902));
#14997=CARTESIAN_POINT('Ctrl Pts',(-3.76619983273375,-2.44146810829183,
4.94993090447612));
#14998=CARTESIAN_POINT('Ctrl Pts',(-3.75039179589374,-2.48334366291991,
4.95271377261321));
#14999=CARTESIAN_POINT('Ctrl Pts',(-3.7221733933057,-2.5136723837762,4.95549664075031));
#15000=CARTESIAN_POINT('Ctrl Pts',(-3.68460862697666,-2.55404643785209,
4.95920123710258));
#15001=CARTESIAN_POINT('Ctrl Pts',(-3.62505103082171,-2.57395795638902,
4.96290583345484));
#15002=CARTESIAN_POINT('Ctrl Pts',(-3.57075747641916,-2.56429432021831,
4.96661042980711));
#15003=CARTESIAN_POINT('Ctrl Pts',(-3.51646392201662,-2.5546306840476,4.97031502615938));
#15004=CARTESIAN_POINT('Ctrl Pts',(-3.46743440936648,-2.51539189316926,
4.97401962251165));
#15005=CARTESIAN_POINT('Ctrl Pts',(-3.44610757298242,-2.46453580233588,
4.97772421886392));
#15006=CARTESIAN_POINT('Ctrl Pts',(-3.42478073659837,-2.41367971150249,
4.98142881521618));
#15007=CARTESIAN_POINT('Ctrl Pts',(-3.43115657648041,-2.35120632071406,
4.98513341156845));
#15008=CARTESIAN_POINT('Ctrl Pts',(-3.46231715328677,-2.30570693229799,
4.98883800792072));
#15009=CARTESIAN_POINT('Ctrl Pts',(-3.49347773009313,-2.26020754388192,
4.99254260427299));
#15010=CARTESIAN_POINT('Ctrl Pts',(-3.54942304382382,-2.2316821578382,4.99624720062526));
#15011=CARTESIAN_POINT('Ctrl Pts',(-3.60454940455119,-2.2331855772681,4.99995179697753));
#15012=CARTESIAN_POINT('Ctrl Pts',(-3.65967576527857,-2.23468899669801,
5.00365639332979));
#15013=CARTESIAN_POINT('Ctrl Pts',(-3.71398317300263,-2.26622122160152,
5.00736098968206));
#15014=CARTESIAN_POINT('Ctrl Pts',(-3.74261753436876,-2.31335135359861,
5.01106558603433));
#15015=CARTESIAN_POINT('Ctrl Pts',(-3.75828879455967,-2.33914513862194,
5.01309306946923));
#15016=CARTESIAN_POINT('Ctrl Pts',(-3.76627033973982,-2.36961088421597,
5.01512055290412));
#15017=CARTESIAN_POINT('Ctrl Pts',(-3.76634000649331,-2.40004261214866,
5.01714803633902));
#15018=CARTESIAN_POINT('Origin',(-3.6,-2.4,4.7));
#15019=CARTESIAN_POINT('',(-3.76673281282141,-2.40013003219325,5.08714803633902));
#15020=CARTESIAN_POINT('',(-3.7668206250807,-2.39991359866148,5.06785196366098));
#15021=CARTESIAN_POINT('',(-3.7666,-2.4,4.7));
#15022=CARTESIAN_POINT('Ctrl Pts',(-3.7668206250807,-2.39991359866148,5.06785196366098));
#15023=CARTESIAN_POINT('Ctrl Pts',(-3.76685198944486,-2.39494457920613,
5.06751845741382));
#15024=CARTESIAN_POINT('Ctrl Pts',(-3.7666492146414,-2.38997815520014,5.06718495116665));
#15025=CARTESIAN_POINT('Ctrl Pts',(-3.7662039619217,-2.38503356610626,5.06685144491949));
#15026=CARTESIAN_POINT('Ctrl Pts',(-3.76125808275068,-2.33010893762799,
5.06314684856722));
#15027=CARTESIAN_POINT('Ctrl Pts',(-3.72639327521678,-2.27787848097877,
5.05944225221495));
#15028=CARTESIAN_POINT('Ctrl Pts',(-3.67756563230702,-2.25224574125102,
5.05573765586268));
#15029=CARTESIAN_POINT('Ctrl Pts',(-3.62873798939725,-2.22661300152326,
5.05203305951042));
#15030=CARTESIAN_POINT('Ctrl Pts',(-3.56594751111163,-2.22757797871697,
5.04832846315815));
#15031=CARTESIAN_POINT('Ctrl Pts',(-3.51793060783244,-2.25469905531577,
5.04462386680588));
#15032=CARTESIAN_POINT('Ctrl Pts',(-3.46991370455325,-2.28182013191457,
5.04091927045361));
#15033=CARTESIAN_POINT('Ctrl Pts',(-3.43667037628051,-2.33509730791846,
5.03721467410135));
#15034=CARTESIAN_POINT('Ctrl Pts',(-3.43341462472151,-2.39014797674899,
5.03351007774908));
#15035=CARTESIAN_POINT('Ctrl Pts',(-3.43015887316251,-2.44519864557951,
5.02980548139681));
#15036=CARTESIAN_POINT('Ctrl Pts',(-3.45689069831725,-2.50202280723666,
5.02610088504454));
#15037=CARTESIAN_POINT('Ctrl Pts',(-3.50137612681596,-2.53461456435925,
5.02239628869227));
#15038=CARTESIAN_POINT('Ctrl Pts',(-3.54586155531466,-2.56720632148184,
5.01869169234));
#15039=CARTESIAN_POINT('Ctrl Pts',(-3.60810058715733,-2.57556567406988,
5.01498709598774));
#15040=CARTESIAN_POINT('Ctrl Pts',(-3.65960917750461,-2.5558669157941,5.01128249963547));
#15041=CARTESIAN_POINT('Ctrl Pts',(-3.71111776785188,-2.53616815751832,
5.0075779032832));
#15042=CARTESIAN_POINT('Ctrl Pts',(-3.75189591670377,-2.48841128837874,
5.00387330693093));
#15043=CARTESIAN_POINT('Ctrl Pts',(-3.7632812725096,-2.4344525109445,5.00016871057867));
#15044=CARTESIAN_POINT('Ctrl Pts',(-3.76565462941201,-2.42320442708544,
4.9993964616061));
#15045=CARTESIAN_POINT('Ctrl Pts',(-3.7667507426838,-2.41168684356181,4.99862421263354));
#15046=CARTESIAN_POINT('Ctrl Pts',(-3.76664426409402,-2.40014916296054,
4.99785196366098));
#15047=CARTESIAN_POINT('Ctrl Pts',(-3.76634000649331,-2.40004261214866,
5.01714803633902));
#15048=CARTESIAN_POINT('Ctrl Pts',(-3.76639763409716,-2.42521541658955,
5.01882514925639));
#15049=CARTESIAN_POINT('Ctrl Pts',(-3.76104161906272,-2.45036494470439,
5.02050226217376));
#15050=CARTESIAN_POINT('Ctrl Pts',(-3.75014621732021,-2.47282762178721,
5.02217937509113));
#15051=CARTESIAN_POINT('Ctrl Pts',(-3.72607922389733,-2.52244571888807,
5.0258839714434));
#15052=CARTESIAN_POINT('Ctrl Pts',(-3.67498392204337,-2.55895387399913,
5.02958856779567));
#15053=CARTESIAN_POINT('Ctrl Pts',(-3.62024436531629,-2.56564393553624,
5.03329316414794));
#15054=CARTESIAN_POINT('Ctrl Pts',(-3.5655048085892,-2.57233399707334,5.03699776050021));
#15055=CARTESIAN_POINT('Ctrl Pts',(-3.50712099698899,-2.54920596503651,
5.04070235685248));
#15056=CARTESIAN_POINT('Ctrl Pts',(-3.47181261508692,-2.50684448916664,
5.04440695320474));
#15057=CARTESIAN_POINT('Ctrl Pts',(-3.43650423318484,-2.46448301329678,
5.04811154955701));
#15058=CARTESIAN_POINT('Ctrl Pts',(-3.42427128098091,-2.4028880935939,5.05181614590928));
#15059=CARTESIAN_POINT('Ctrl Pts',(-3.44071223414431,-2.35024904491843,
5.05552074226155));
#15060=CARTESIAN_POINT('Ctrl Pts',(-3.45715318730771,-2.29760999624296,
5.05922533861381));
#15061=CARTESIAN_POINT('Ctrl Pts',(-3.50226804583846,-2.2539268185949,5.06292993496608));
#15062=CARTESIAN_POINT('Ctrl Pts',(-3.55540974746646,-2.23919126462175,
5.06663453131835));
#15063=CARTESIAN_POINT('Ctrl Pts',(-3.60855144909447,-2.2244557106486,5.07033912767062));
#15064=CARTESIAN_POINT('Ctrl Pts',(-3.66971999381974,-2.23866778035036,
5.07404372402289));
#15065=CARTESIAN_POINT('Ctrl Pts',(-3.71092123316877,-2.27532344228896,
5.07774832037516));
#15066=CARTESIAN_POINT('Ctrl Pts',(-3.74576802981578,-2.30632572323287,
5.08088155902978));
#15067=CARTESIAN_POINT('Ctrl Pts',(-3.76633165591099,-2.35338253179949,
5.0840147976844));
#15068=CARTESIAN_POINT('Ctrl Pts',(-3.76673281282141,-2.40013003219325,
5.08714803633902));
#15069=CARTESIAN_POINT('Origin',(-3.6,-2.4,4.7));
#15070=CARTESIAN_POINT('',(-3.76674783764939,-2.3998784327954,5.15714803633902));
#15071=CARTESIAN_POINT('',(-3.76638442554721,-2.39990578503699,5.13785196366098));
#15072=CARTESIAN_POINT('',(-3.7666,-2.4,4.7));
#15073=CARTESIAN_POINT('',(-3.47309291201476,-2.29206413469515,5.2));
#15074=CARTESIAN_POINT('Ctrl Pts',(-3.76674783764939,-2.3998784327954,5.15714803633902));
#15075=CARTESIAN_POINT('Ctrl Pts',(-3.7663543041176,-2.44715561431286,5.16031823516921));
#15076=CARTESIAN_POINT('Ctrl Pts',(-3.74524548348422,-2.49473161213543,
5.1634884339994));
#15077=CARTESIAN_POINT('Ctrl Pts',(-3.70967617757414,-2.52575977295725,
5.16665863282959));
#15078=CARTESIAN_POINT('Ctrl Pts',(-3.66811098624533,-2.56201832251683,
5.17036322918186));
#15079=CARTESIAN_POINT('Ctrl Pts',(-3.60679922558629,-2.57567991185357,
5.17406782553412));
#15080=CARTESIAN_POINT('Ctrl Pts',(-3.55380862744679,-2.56038491971217,
5.17777242188639));
#15081=CARTESIAN_POINT('Ctrl Pts',(-3.5008180293073,-2.54508992757078,5.18147701823866));
#15082=CARTESIAN_POINT('Ctrl Pts',(-3.45614859368735,-2.50083835395125,
5.18518161459093));
#15083=CARTESIAN_POINT('Ctrl Pts',(-3.44024450358536,-2.44813181223257,
5.1888862109432));
#15084=CARTESIAN_POINT('Ctrl Pts',(-3.42434041348337,-2.39542527051388,
5.19259080729547));
#15085=CARTESIAN_POINT('Ctrl Pts',(-3.43720166889934,-2.33426376069605,
5.19629540364773));
#15086=CARTESIAN_POINT('Ctrl Pts',(-3.47309291201476,-2.29206413469515,
5.2));
#15087=CARTESIAN_POINT('',(-3.7271475418302,-2.29187968016137,5.2));
#15088=CARTESIAN_POINT('Origin',(-3.6,-2.4,5.2));
#15089=CARTESIAN_POINT('Ctrl Pts',(-3.72714769448933,-2.29187956305504,
5.2));
#15090=CARTESIAN_POINT('Ctrl Pts',(-3.69206190113039,-2.25072743961435,
5.19636770818144));
#15091=CARTESIAN_POINT('Ctrl Pts',(-3.6350641341643,-2.22812240899828,5.19273541636289));
#15092=CARTESIAN_POINT('Ctrl Pts',(-3.58132375070445,-2.23418207790235,
5.18910312454434));
#15093=CARTESIAN_POINT('Ctrl Pts',(-3.52651360920706,-2.24036237079714,
5.18539852819207));
#15094=CARTESIAN_POINT('Ctrl Pts',(-3.47509182514536,-2.27635992272048,
5.1816939318398));
#15095=CARTESIAN_POINT('Ctrl Pts',(-3.45055836147391,-2.3257410419838,5.17798933548753));
#15096=CARTESIAN_POINT('Ctrl Pts',(-3.42602489780247,-2.37512216124712,
5.17428473913526));
#15097=CARTESIAN_POINT('Ctrl Pts',(-3.42837975452128,-2.43788684785041,
5.170580142783));
#15098=CARTESIAN_POINT('Ctrl Pts',(-3.45656193213921,-2.48529019920904,
5.16687554643073));
#15099=CARTESIAN_POINT('Ctrl Pts',(-3.48474410975714,-2.53269355056767,
5.16317095007846));
#15100=CARTESIAN_POINT('Ctrl Pts',(-3.53875360827419,-2.56473556668165,
5.15946635372619));
#15101=CARTESIAN_POINT('Ctrl Pts',(-3.59386432904901,-2.56676216280164,
5.15576175737392));
#15102=CARTESIAN_POINT('Ctrl Pts',(-3.64897504982384,-2.56878875892163,
5.15205716102165));
#15103=CARTESIAN_POINT('Ctrl Pts',(-3.70518699285644,-2.54079993504764,
5.14835256466939));
#15104=CARTESIAN_POINT('Ctrl Pts',(-3.73677861120293,-2.49559987891255,
5.14464796831712));
#15105=CARTESIAN_POINT('Ctrl Pts',(-3.75609666594378,-2.46796035917884,
5.14238263343174));
#15106=CARTESIAN_POINT('Ctrl Pts',(-3.76620859684834,-2.43388515114326,
5.14011729854636));
#15107=CARTESIAN_POINT('Ctrl Pts',(-3.76638442554721,-2.39990578503699,
5.13785196366098));
#15108=CARTESIAN_POINT('Origin',(-3.6,-2.4,5.35459252805377));
#15109=CARTESIAN_POINT('',(-3.8057227013582,-2.39988044337606,4.34540747194623));
#15110=CARTESIAN_POINT('',(-3.80516111137892,-2.40008013262119,4.33959252805377));
#15111=CARTESIAN_POINT('',(-3.805475,-2.39999999999999,5.35459252805377));
#15112=CARTESIAN_POINT('',(-3.41173724903364,-2.48232321801035,4.3));
#15113=CARTESIAN_POINT('Ctrl Pts',(-3.80516111137892,-2.40008013262119,
4.33959252805377));
#15114=CARTESIAN_POINT('Ctrl Pts',(-3.80504330063484,-2.36152007992449,
4.33750880775931));
#15115=CARTESIAN_POINT('Ctrl Pts',(-3.77605833105766,-2.25423615375421,
4.33172049111259));
#15116=CARTESIAN_POINT('Ctrl Pts',(-3.60297473301061,-2.15700944143379,
4.32222757811361));
#15117=CARTESIAN_POINT('Ctrl Pts',(-3.39749761512046,-2.26611614077921,
4.3111137890568));
#15118=CARTESIAN_POINT('Ctrl Pts',(-3.38436282049399,-2.419721374356,4.30370459635227));
#15119=CARTESIAN_POINT('Ctrl Pts',(-3.41173724903364,-2.48232321801035,
4.3));
#15120=CARTESIAN_POINT('',(-3.47764162637991,-2.56553534042572,4.3));
#15121=CARTESIAN_POINT('Origin',(-3.6,-2.4,4.3));
#15122=CARTESIAN_POINT('Ctrl Pts',(-3.8057227013582,-2.39988044337606,4.34540747194623));
#15123=CARTESIAN_POINT('Ctrl Pts',(-3.8057729696998,-2.39271640638513,4.34501772883951));
#15124=CARTESIAN_POINT('Ctrl Pts',(-3.80218373546239,-2.3175070024762,4.34092338938053));
#15125=CARTESIAN_POINT('Ctrl Pts',(-3.70962995644976,-2.18326697275372,
4.33312445356927));
#15126=CARTESIAN_POINT('Ctrl Pts',(-3.47734459894833,-2.19039236572141,
4.32201066451247));
#15127=CARTESIAN_POINT('Ctrl Pts',(-3.35820162590419,-2.3879909133699,4.31096917998938));
#15128=CARTESIAN_POINT('Ctrl Pts',(-3.42405718781536,-2.52582031335719,
4.30363229181855));
#15129=CARTESIAN_POINT('Ctrl Pts',(-3.47764149510761,-2.56553553810743,
4.3));
#15130=CARTESIAN_POINT('Origin',(-3.6,-2.4,5.35459252805377));
#15131=CARTESIAN_POINT('',(-3.80519266468163,-2.39989734570579,4.41540747194623));
#15132=CARTESIAN_POINT('',(-3.80566724789774,-2.40014978098439,4.40959252805377));
#15133=CARTESIAN_POINT('',(-3.805475,-2.39999999999999,5.35459252805377));
#15134=CARTESIAN_POINT('Ctrl Pts',(-3.80566724789774,-2.40014978098439,
4.40959252805377));
#15135=CARTESIAN_POINT('Ctrl Pts',(-3.80518614471975,-2.34148051217519,
4.40640305253959));
#15136=CARTESIAN_POINT('Ctrl Pts',(-3.74813829229662,-2.21384966330463,
4.39950898067315));
#15137=CARTESIAN_POINT('Ctrl Pts',(-3.53156901893564,-2.16697244735031,
4.38891031245443));
#15138=CARTESIAN_POINT('Ctrl Pts',(-3.36710794136624,-2.33111753922242,
4.37779652339762));
#15139=CARTESIAN_POINT('Ctrl Pts',(-3.41581894666805,-2.55829572590735,
4.36668273434083));
#15140=CARTESIAN_POINT('Ctrl Pts',(-3.63310626972243,-2.64061568298545,
4.35556894528402));
#15141=CARTESIAN_POINT('Ctrl Pts',(-3.7850442261316,-2.5285041432322,4.34653887652167));
#15142=CARTESIAN_POINT('Ctrl Pts',(-3.80525275353212,-2.43007507309885,
4.34121340411158));
#15143=CARTESIAN_POINT('Ctrl Pts',(-3.80516111137892,-2.40008013262119,
4.33959252805377));
#15144=CARTESIAN_POINT('Ctrl Pts',(-3.80519266468163,-2.39989734570579,
4.41540747194623));
#15145=CARTESIAN_POINT('Ctrl Pts',(-3.80531782889597,-2.37222562131849,
4.41391197361979));
#15146=CARTESIAN_POINT('Ctrl Pts',(-3.78721617857279,-2.2761634023784,4.40871187894108));
#15147=CARTESIAN_POINT('Ctrl Pts',(-3.64121277969171,-2.16065653443092,
4.3998071879101));
#15148=CARTESIAN_POINT('Ctrl Pts',(-3.42126523797479,-2.23556891230323,
4.38869339885329));
#15149=CARTESIAN_POINT('Ctrl Pts',(-3.36491711226222,-2.46098554747977,
4.37757960979649));
#15150=CARTESIAN_POINT('Ctrl Pts',(-3.52374009350676,-2.63058418685777,
4.36646582073969));
#15151=CARTESIAN_POINT('Ctrl Pts',(-3.74435278297668,-2.59057501347053,
4.3557417747896));
#15152=CARTESIAN_POINT('Ctrl Pts',(-3.80529515774691,-2.46081219780934,
4.34872232519178));
#15153=CARTESIAN_POINT('Ctrl Pts',(-3.8057227013582,-2.39988044337606,4.34540747194623));
#15154=CARTESIAN_POINT('Origin',(-3.6,-2.4,5.35459252805377));
#15155=CARTESIAN_POINT('',(-3.80534991328218,-2.40017652766129,4.48540747194623));
#15156=CARTESIAN_POINT('',(-3.80562878759967,-2.39983660975823,4.47959252805377));
#15157=CARTESIAN_POINT('',(-3.805475,-2.39999999999999,5.35459252805377));
#15158=CARTESIAN_POINT('Ctrl Pts',(-3.80562878759967,-2.39983660975823,
4.47959252805377));
#15159=CARTESIAN_POINT('Ctrl Pts',(-3.80572325938657,-2.3889667780224,4.47900189367213));
#15160=CARTESIAN_POINT('Ctrl Pts',(-3.79999615684062,-2.31001856287219,
4.47470666293823));
#15161=CARTESIAN_POINT('Ctrl Pts',(-3.69773850858379,-2.17766949547173,
4.46670683585206));
#15162=CARTESIAN_POINT('Ctrl Pts',(-3.46621554409366,-2.19730464027232,
4.45559304679525));
#15163=CARTESIAN_POINT('Ctrl Pts',(-3.35714698343348,-2.40246926898597,
4.44447925773846));
#15164=CARTESIAN_POINT('Ctrl Pts',(-3.47036459479899,-2.60537350263611,
4.43336546868164));
#15165=CARTESIAN_POINT('Ctrl Pts',(-3.70223885894321,-2.62029753112878,
4.42225167962485));
#15166=CARTESIAN_POINT('Ctrl Pts',(-3.80084480548257,-2.48716469502641,
4.41432736608222));
#15167=CARTESIAN_POINT('Ctrl Pts',(-3.80574494915964,-2.40962524577001,
4.41010764889186));
#15168=CARTESIAN_POINT('Ctrl Pts',(-3.80566724789774,-2.40014978098439,
4.40959252805377));
#15169=CARTESIAN_POINT('Ctrl Pts',(-3.80534991328218,-2.40017652766129,
4.48540747194623));
#15170=CARTESIAN_POINT('Ctrl Pts',(-3.8049563333145,-2.35213729171836,4.48280621840006));
#15171=CARTESIAN_POINT('Ctrl Pts',(-3.76418777806192,-2.23508077339291,
4.47650036850163));
#15172=CARTESIAN_POINT('Ctrl Pts',(-3.56918135654791,-2.15909775573836,
4.46648992225092));
#15173=CARTESIAN_POINT('Ctrl Pts',(-3.38089013692747,-2.29524052189659,
4.45537613319412));
#15174=CARTESIAN_POINT('Ctrl Pts',(-3.39315268252002,-2.52727080497827,
4.44426234413731));
#15175=CARTESIAN_POINT('Ctrl Pts',(-3.59474487821944,-2.64280871984201,
4.43314855508051));
#15176=CARTESIAN_POINT('Ctrl Pts',(-3.77337323688511,-2.5504598261374,4.42353026435015));
#15177=CARTESIAN_POINT('Ctrl Pts',(-3.80500777646484,-2.44077305290937,
4.41761656997206));
#15178=CARTESIAN_POINT('Ctrl Pts',(-3.80519266468163,-2.39989734570579,
4.41540747194623));
#15179=CARTESIAN_POINT('Origin',(-3.6,-2.4,5.35459252805377));
#15180=CARTESIAN_POINT('',(-3.80581595477291,-2.39999917227814,4.55540747194623));
#15181=CARTESIAN_POINT('',(-3.80515176250663,-2.39995310238523,4.54959252805377));
#15182=CARTESIAN_POINT('',(-3.805475,-2.39999999999999,5.35459252805377));
#15183=CARTESIAN_POINT('Ctrl Pts',(-3.80515176250663,-2.39995310238523,
4.54959252805377));
#15184=CARTESIAN_POINT('Ctrl Pts',(-3.80521587176166,-2.36854855820361,
4.54789613845241));
#15185=CARTESIAN_POINT('Ctrl Pts',(-3.78367651299531,-2.26864576859469,
4.54249515249878));
#15186=CARTESIAN_POINT('Ctrl Pts',(-3.62821111895818,-2.15877850380716,
4.53338957019289));
#15187=CARTESIAN_POINT('Ctrl Pts',(-3.4126363777684,-2.24547313898512,4.52227578113608));
#15188=CARTESIAN_POINT('Ctrl Pts',(-3.3685576844537,-2.47360796440317,4.51116199207928));
#15189=CARTESIAN_POINT('Ctrl Pts',(-3.53632076809686,-2.63436858142862,
4.50004820302248));
#15190=CARTESIAN_POINT('Ctrl Pts',(-3.75035693907624,-2.58346600089298,
4.4895250483473));
#15191=CARTESIAN_POINT('Ctrl Pts',(-3.80513071034435,-2.45714489336835,
4.4827064900244));
#15192=CARTESIAN_POINT('Ctrl Pts',(-3.80562878759967,-2.39983660975823,
4.47959252805377));
#15193=CARTESIAN_POINT('Ctrl Pts',(-3.80581595309039,-2.39999917228222,
4.55540747194623));
#15194=CARTESIAN_POINT('Ctrl Pts',(-3.80581595573579,-2.39995488126346,
4.55540505953261));
#15195=CARTESIAN_POINT('Ctrl Pts',(-3.805795885724,-2.33189557869137,4.55169805076671));
#15196=CARTESIAN_POINT('Ctrl Pts',(-3.73158417960078,-2.19586944742698,
4.54428644564855));
#15197=CARTESIAN_POINT('Ctrl Pts',(-3.49986236155564,-2.17873967321655,
4.53317265659175));
#15198=CARTESIAN_POINT('Ctrl Pts',(-3.35979765944108,-2.36413198553984,
4.52205886753494));
#15199=CARTESIAN_POINT('Ctrl Pts',(-3.43959288407154,-2.58235469793693,
4.51094507847814));
#15200=CARTESIAN_POINT('Ctrl Pts',(-3.66621056034765,-2.6336660879353,4.49983128942134));
#15201=CARTESIAN_POINT('Ctrl Pts',(-3.79336822690886,-2.50914983096546,
4.4913187539107));
#15202=CARTESIAN_POINT('Ctrl Pts',(-3.80551685342017,-2.42055275952314,
4.48651081475233));
#15203=CARTESIAN_POINT('Ctrl Pts',(-3.80534991328218,-2.40017652766129,
4.48540747194623));
#15204=CARTESIAN_POINT('Origin',(-3.6,-2.4,5.35459252805377));
#15205=CARTESIAN_POINT('',(-3.80534749847032,-2.39982399268994,4.62540747194623));
#15206=CARTESIAN_POINT('',(-3.80545680064795,-2.40018789159516,4.61959252805377));
#15207=CARTESIAN_POINT('',(-3.805475,-2.39999999999999,5.35459252805377));
#15208=CARTESIAN_POINT('Ctrl Pts',(-3.80545680064795,-2.40018789159516,
4.61959252805377));
#15209=CARTESIAN_POINT('Ctrl Pts',(-3.80498629881388,-2.34850704133116,
4.61679038323269));
#15210=CARTESIAN_POINT('Ctrl Pts',(-3.75902064354221,-2.22775548399901,
4.61028364205933));
#15211=CARTESIAN_POINT('Ctrl Pts',(-3.55620097341096,-2.16111650777606,
4.60007230453371));
#15212=CARTESIAN_POINT('Ctrl Pts',(-3.37554637252617,-2.307240921179,4.58895851547691));
#15213=CARTESIAN_POINT('Ctrl Pts',(-3.40033672233922,-2.53826877141577,
4.57784472642011));
#15214=CARTESIAN_POINT('Ctrl Pts',(-3.60788113454322,-2.64273764704216,
4.5667309373633));
#15215=CARTESIAN_POINT('Ctrl Pts',(-3.7776337191139,-2.54299330423865,4.55731353790786));
#15216=CARTESIAN_POINT('Ctrl Pts',(-3.80507586918669,-2.43713018575349,
4.55160073480468));
#15217=CARTESIAN_POINT('Ctrl Pts',(-3.80515176250663,-2.39995310238523,
4.54959252805377));
#15218=CARTESIAN_POINT('Ctrl Pts',(-3.80534749847032,-2.39982399268994,
4.62540747194623));
#15219=CARTESIAN_POINT('Ctrl Pts',(-3.8055145307928,-2.37935804813576,4.62429930431288));
#15220=CARTESIAN_POINT('Ctrl Pts',(-3.79329841632202,-2.29066951260838,
4.61948654032727));
#15221=CARTESIAN_POINT('Ctrl Pts',(-3.66590691978443,-2.16624808716256,
4.61096917998938));
#15222=CARTESIAN_POINT('Ctrl Pts',(-3.4393560992794,-2.21785386089149,4.59985539093257));
#15223=CARTESIAN_POINT('Ctrl Pts',(-3.35984446292695,-2.43618006142673,
4.58874160187577));
#15224=CARTESIAN_POINT('Ctrl Pts',(-3.50014991321196,-2.62139024142312,
4.57762781281897));
#15225=CARTESIAN_POINT('Ctrl Pts',(-3.73179898649779,-2.60396320633826,
4.56651643617578));
#15226=CARTESIAN_POINT('Ctrl Pts',(-3.80581189336919,-2.46796989528688,
4.55910965588487));
#15227=CARTESIAN_POINT('Ctrl Pts',(-3.80581595309039,-2.39999917228222,
4.55540747194623));
#15228=CARTESIAN_POINT('Origin',(-3.6,-2.4,5.35459252805377));
#15229=CARTESIAN_POINT('',(-3.80519404433776,-2.40010391087563,4.69540747194623));
#15230=CARTESIAN_POINT('',(-3.80578860319875,-2.39993212258736,4.68959252805377));
#15231=CARTESIAN_POINT('',(-3.805475,-2.39999999999999,5.35459252805377));
#15232=CARTESIAN_POINT('Ctrl Pts',(-3.80578860319875,-2.39993212258736,
4.68959252805377));
#15233=CARTESIAN_POINT('Ctrl Pts',(-3.80580467529652,-2.39619821380325,
4.68938922436523));
#15234=CARTESIAN_POINT('Ctrl Pts',(-3.8040203847709,-2.32444075317719,4.68548132432442));
#15235=CARTESIAN_POINT('Ctrl Pts',(-3.72035445765201,-2.18905336667194,
4.67786882793134));
#15236=CARTESIAN_POINT('Ctrl Pts',(-3.4880454122232,-2.18447773232253,4.66675503887454));
#15237=CARTESIAN_POINT('Ctrl Pts',(-3.35820967063793,-2.37717207376684,
4.65564124981773));
#15238=CARTESIAN_POINT('Ctrl Pts',(-3.4496873596065,-2.5907610749791,4.64452746076093));
#15239=CARTESIAN_POINT('Ctrl Pts',(-3.67874791298872,-2.62974430088435,
4.63341367170412));
#15240=CARTESIAN_POINT('Ctrl Pts',(-3.79614945789441,-2.50163131370898,
4.62510202746841));
#15241=CARTESIAN_POINT('Ctrl Pts',(-3.80560832925468,-2.41683209288794,
4.62049497958495));
#15242=CARTESIAN_POINT('Ctrl Pts',(-3.80545680064795,-2.40018789159516,
4.61959252805377));
#15243=CARTESIAN_POINT('Ctrl Pts',(-3.80519404433776,-2.40010391087563,
4.69540747194623));
#15244=CARTESIAN_POINT('Ctrl Pts',(-3.80500644622954,-2.35913959443751,
4.69319354909316));
#15245=CARTESIAN_POINT('Ctrl Pts',(-3.77326723416865,-2.24936122008858,
4.68727502988781));
#15246=CARTESIAN_POINT('Ctrl Pts',(-3.59442944460758,-2.15719833661306,
4.6776519143302));
#15247=CARTESIAN_POINT('Ctrl Pts',(-3.3929874908777,-2.27299803191391,4.6665381252734));
#15248=CARTESIAN_POINT('Ctrl Pts',(-3.38102643442896,-2.50504406890429,
4.65542433621659));
#15249=CARTESIAN_POINT('Ctrl Pts',(-3.5694943658766,-2.64094207834572,4.64431054715979));
#15250=CARTESIAN_POINT('Ctrl Pts',(-3.76430796656755,-2.56474251573525,
4.63430492573634));
#15251=CARTESIAN_POINT('Ctrl Pts',(-3.8049561429515,-2.44777555218424,4.62800390066515));
#15252=CARTESIAN_POINT('Ctrl Pts',(-3.80534749847032,-2.39982399268994,
4.62540747194623));
#15253=CARTESIAN_POINT('Origin',(-3.6,-2.4,5.35459252805377));
#15254=CARTESIAN_POINT('',(-3.80572671416466,-2.40012021867279,4.76540747194623));
#15255=CARTESIAN_POINT('',(-3.80525640542964,-2.39985490132803,4.75959252805377));
#15256=CARTESIAN_POINT('',(-3.805475,-2.39999999999999,5.35459252805377));
#15257=CARTESIAN_POINT('Ctrl Pts',(-3.80525640542964,-2.39985490132803,
4.75959252805377));
#15258=CARTESIAN_POINT('Ctrl Pts',(-3.80541421756911,-2.37565177743561,
4.7582834691455));
#15259=CARTESIAN_POINT('Ctrl Pts',(-3.7902631541036,-2.2831457592228,4.75326981388497));
#15260=CARTESIAN_POINT('Ctrl Pts',(-3.65317166084996,-2.16302647390142,
4.74455156227217));
#15261=CARTESIAN_POINT('Ctrl Pts',(-3.42974254509416,-2.22680624538361,
4.73343777321536));
#15262=CARTESIAN_POINT('Ctrl Pts',(-3.36215200866455,-2.44911222461694,
4.72232398415856));
#15263=CARTESIAN_POINT('Ctrl Pts',(-3.51226643608395,-2.62646522768789,
4.71121019510176));
#15264=CARTESIAN_POINT('Ctrl Pts',(-3.73846937161942,-2.59707960507412,
4.70029970973349));
#15265=CARTESIAN_POINT('Ctrl Pts',(-3.80551180980452,-2.46423743611441,
4.6930938207175));
#15266=CARTESIAN_POINT('Ctrl Pts',(-3.80578860319875,-2.39993212258736,
4.68959252805377));
#15267=CARTESIAN_POINT('Ctrl Pts',(-3.80572671416466,-2.40012021867279,
4.76540747194623));
#15268=CARTESIAN_POINT('Ctrl Pts',(-3.80530257178557,-2.33910193112031,
4.76208779387343));
#15269=CARTESIAN_POINT('Ctrl Pts',(-3.74420123427486,-2.20925254264417,
4.75506351944836));
#15270=CARTESIAN_POINT('Ctrl Pts',(-3.52344221265408,-2.16951662960737,
4.74433464867103));
#15271=CARTESIAN_POINT('Ctrl Pts',(-3.36483725976158,-2.33931915924769,
4.73322085961422));
#15272=CARTESIAN_POINT('Ctrl Pts',(-3.42147942993616,-2.56466355059616,
4.72210707055742));
#15273=CARTESIAN_POINT('Ctrl Pts',(-3.64152350245114,-2.63928952667227,
4.71099328150061));
#15274=CARTESIAN_POINT('Ctrl Pts',(-3.78729792557216,-2.52365598332802,
4.70209341529689));
#15275=CARTESIAN_POINT('Ctrl Pts',(-3.80532035746924,-2.42768591123397,
4.69689814544542));
#15276=CARTESIAN_POINT('Ctrl Pts',(-3.80519404433776,-2.40010391087563,
4.69540747194623));
#15277=CARTESIAN_POINT('Origin',(-3.6,-2.4,5.35459252805377));
#15278=CARTESIAN_POINT('',(-3.80555826192291,-2.39982008596012,4.83540747194623));
#15279=CARTESIAN_POINT('',(-3.80526423797111,-2.40014879660671,4.82959252805377));
#15280=CARTESIAN_POINT('',(-3.805475,-2.39999999999999,5.35459252805377));
#15281=CARTESIAN_POINT('Ctrl Pts',(-3.80526423797112,-2.40014879660671,
4.82959252805377));
#15282=CARTESIAN_POINT('Ctrl Pts',(-3.80496497000794,-2.35550570352956,
4.82717771392578));
#15283=CARTESIAN_POINT('Ctrl Pts',(-3.7687007786119,-2.24193241424781,4.82105830344552));
#15284=CARTESIAN_POINT('Ctrl Pts',(-3.58130943002562,-2.15785471265546,
4.81123429661298));
#15285=CARTESIAN_POINT('Ctrl Pts',(-3.38642338383962,-2.28437687679961,
4.8001205075562));
#15286=CARTESIAN_POINT('Ctrl Pts',(-3.38702643654876,-2.51673019686447,
4.78900671849938));
#15287=CARTESIAN_POINT('Ctrl Pts',(-3.58256660716932,-2.64223904392882,
4.77789292944258));
#15288=CARTESIAN_POINT('Ctrl Pts',(-3.76915216315368,-2.5573566497576,4.76808819929404));
#15289=CARTESIAN_POINT('Ctrl Pts',(-3.80496761407973,-2.44414587187183,
4.76198806549777));
#15290=CARTESIAN_POINT('Ctrl Pts',(-3.80525640542964,-2.39985490132803,
4.75959252805377));
#15291=CARTESIAN_POINT('Ctrl Pts',(-3.80555826192291,-2.39982008596012,
4.83540747194623));
#15292=CARTESIAN_POINT('Ctrl Pts',(-3.80567994930423,-2.38654227868304,
4.83468663500597));
#15293=CARTESIAN_POINT('Ctrl Pts',(-3.79845786380229,-2.30515766788849,
4.83026120171345));
#15294=CARTESIAN_POINT('Ctrl Pts',(-3.68988494304833,-2.17438001896094,
4.82213117206866));
#15295=CARTESIAN_POINT('Ctrl Pts',(-3.45919253805822,-2.20211888040452,
4.81101738301185));
#15296=CARTESIAN_POINT('Ctrl Pts',(-3.35738279984868,-2.41098057473832,
4.79990359395505));
#15297=CARTESIAN_POINT('Ctrl Pts',(-3.47764333640382,-2.60979162448597,
4.78878980489824));
#15298=CARTESIAN_POINT('Ctrl Pts',(-3.7098983147675,-2.61657802114276,4.77767601584144));
#15299=CARTESIAN_POINT('Ctrl Pts',(-3.80223426786157,-2.48231400602396,
4.76988190485744));
#15300=CARTESIAN_POINT('Ctrl Pts',(-3.80577589367883,-2.40719531865107,
4.7657923902257));
#15301=CARTESIAN_POINT('Ctrl Pts',(-3.80572671416466,-2.40012021867279,
4.76540747194623));
#15302=CARTESIAN_POINT('Origin',(-3.6,-2.4,5.35459252805377));
#15303=CARTESIAN_POINT('',(-3.80514217248594,-2.39999218980904,4.90540747194623));
#15304=CARTESIAN_POINT('',(-3.80579332868662,-2.40006173798069,4.89959252805377));
#15305=CARTESIAN_POINT('',(-3.805475,-2.39999999999999,5.35459252805377));
#15306=CARTESIAN_POINT('Ctrl Pts',(-3.80579332868662,-2.40006173798069,
4.89959252805377));
#15307=CARTESIAN_POINT('Ctrl Pts',(-3.80553739175956,-2.33540634391997,
4.89607195870605));
#15308=CARTESIAN_POINT('Ctrl Pts',(-3.73784442753819,-2.20225412798971,
4.88884679300607));
#15309=CARTESIAN_POINT('Ctrl Pts',(-3.511092084609,-2.17399322981363,4.87791703095382));
#15310=CARTESIAN_POINT('Ctrl Pts',(-3.36190028176488,-2.35212305601353,
4.86680324189701));
#15311=CARTESIAN_POINT('Ctrl Pts',(-3.43064385125587,-2.57407519200526,
4.85568945284021));
#15312=CARTESIAN_POINT('Ctrl Pts',(-3.6544010243217,-2.63669433060785,4.84457566378341));
#15313=CARTESIAN_POINT('Ctrl Pts',(-3.79056542018395,-2.51613221267343,
4.83587668885459));
#15314=CARTESIAN_POINT('Ctrl Pts',(-3.80542408070796,-2.42399322720708,
4.83088231027805));
#15315=CARTESIAN_POINT('Ctrl Pts',(-3.80526423797112,-2.40014879660671,
4.82959252805377));
#15316=CARTESIAN_POINT('Ctrl Pts',(-3.80514217248594,-2.39999218980904,
4.90540747194623));
#15317=CARTESIAN_POINT('Ctrl Pts',(-3.80515363847659,-2.36617331522009,
4.90358087978625));
#15318=CARTESIAN_POINT('Ctrl Pts',(-3.78123591841218,-2.26378007899297,
4.898049691274));
#15319=CARTESIAN_POINT('Ctrl Pts',(-3.61973808033182,-2.15793784472475,
4.88881390640949));
#15320=CARTESIAN_POINT('Ctrl Pts',(-3.4073347883606,-2.25213588990288,4.87770011735268));
#15321=CARTESIAN_POINT('Ctrl Pts',(-3.37128014957741,-2.48167563194308,
4.86658632829587));
#15322=CARTESIAN_POINT('Ctrl Pts',(-3.54457538374435,-2.63645674180255,
4.85547253923907));
#15323=CARTESIAN_POINT('Ctrl Pts',(-3.75407113935919,-2.57880494205606,
4.84507958712253));
#15324=CARTESIAN_POINT('Ctrl Pts',(-3.8050545615032,-2.45478089640322,4.83839123135824));
#15325=CARTESIAN_POINT('Ctrl Pts',(-3.80555826192291,-2.39982008596012,
4.83540747194623));
#15326=CARTESIAN_POINT('Origin',(-3.6,-2.4,5.35459252805377));
#15327=CARTESIAN_POINT('',(-3.80552959282545,-2.40018396914357,4.97540747194623));
#15328=CARTESIAN_POINT('',(-3.80544614170703,-2.39981229694107,4.96959252805377));
#15329=CARTESIAN_POINT('',(-3.805475,-2.39999999999999,5.35459252805377));
#15330=CARTESIAN_POINT('Ctrl Pts',(-3.80544614170703,-2.39981229694107,
4.96959252805377));
#15331=CARTESIAN_POINT('Ctrl Pts',(-3.80560005255251,-2.38281031937819,
4.9686707998386));
#15332=CARTESIAN_POINT('Ctrl Pts',(-3.79589308932397,-2.29764759199308,
4.96404447527115));
#15333=CARTESIAN_POINT('Ctrl Pts',(-3.67755429765177,-2.16985003043886,
4.95571355435145));
#15334=CARTESIAN_POINT('Ctrl Pts',(-3.44869918397279,-2.21002173633656,
4.94459976529464));
#15335=CARTESIAN_POINT('Ctrl Pts',(-3.3583314230664,-2.42408270152555,4.93348597623784));
#15336=CARTESIAN_POINT('Ctrl Pts',(-3.48916565133794,-2.61610049686178,
4.92237218718103));
#15337=CARTESIAN_POINT('Ctrl Pts',(-3.7214478158856,-2.61031905668909,4.91125839812423));
#15338=CARTESIAN_POINT('Ctrl Pts',(-3.80419976839027,-2.4748431306509,4.90366517841514));
#15339=CARTESIAN_POINT('Ctrl Pts',(-3.8058067070074,-2.4034414011323,4.89977655505832));
#15340=CARTESIAN_POINT('Ctrl Pts',(-3.80579332868662,-2.40006173798069,
4.89959252805377));
#15341=CARTESIAN_POINT('Ctrl Pts',(-3.80552959282545,-2.40018396914357,
4.97540747194623));
#15342=CARTESIAN_POINT('Ctrl Pts',(-3.80503093302249,-2.34615078230832,
4.97247512456653));
#15343=CARTESIAN_POINT('Ctrl Pts',(-3.75549941719541,-2.22304560401132,
4.96583818083455));
#15344=CARTESIAN_POINT('Ctrl Pts',(-3.54785414492032,-2.16279863265717,
4.9554966407503));
#15345=CARTESIAN_POINT('Ctrl Pts',(-3.37243276525931,-2.31516585290104,
4.94438285169351));
#15346=CARTESIAN_POINT('Ctrl Pts',(-3.40530625649813,-2.54518272988275,
4.9332690626367));
#15347=CARTESIAN_POINT('Ctrl Pts',(-3.61638513906469,-2.64231220781178,
4.9221552735799));
#15348=CARTESIAN_POINT('Ctrl Pts',(-3.78023982132068,-2.53813917250258,
4.91286807668307));
#15349=CARTESIAN_POINT('Ctrl Pts',(-3.80513038376869,-2.43476294468685,
4.90728547613852));
#15350=CARTESIAN_POINT('Ctrl Pts',(-3.80514217248594,-2.39999218980904,
4.90540747194623));
#15351=CARTESIAN_POINT('Origin',(-3.6,-2.4,5.35459252805377));
#15352=CARTESIAN_POINT('',(-3.80574710647333,-2.39989343748479,5.04540747194623));
#15353=CARTESIAN_POINT('',(-3.80515433874078,-2.40005255540964,5.03959252805377));
#15354=CARTESIAN_POINT('',(-3.805475,-2.39999999999999,5.35459252805377));
#15355=CARTESIAN_POINT('Ctrl Pts',(-3.80515433874078,-2.40005255540964,
5.03959252805377));
#15356=CARTESIAN_POINT('Ctrl Pts',(-3.80506841571452,-2.36251978652027,
5.03756504461887));
#15357=CARTESIAN_POINT('Ctrl Pts',(-3.77723760351786,-2.25628892207963,
5.0318329648317));
#15358=CARTESIAN_POINT('Ctrl Pts',(-3.60662102802227,-2.15722471599323,
5.02239628869228));
#15359=CARTESIAN_POINT('Ctrl Pts',(-3.39962168818772,-2.262769500459,5.01128249963546));
#15360=CARTESIAN_POINT('Ctrl Pts',(-3.37603088927244,-2.49392292132789,
5.00016871057867));
#15361=CARTESIAN_POINT('Ctrl Pts',(-3.55744155755193,-2.63910762521254,
4.98905492152185));
#15362=CARTESIAN_POINT('Ctrl Pts',(-3.75953036700652,-2.57154453779223,
4.97886286068023));
#15363=CARTESIAN_POINT('Ctrl Pts',(-3.80498145636834,-2.45114441507362,
4.97237539619086));
#15364=CARTESIAN_POINT('Ctrl Pts',(-3.80544614170703,-2.39981229694107,
4.96959252805377));
#15365=CARTESIAN_POINT('Ctrl Pts',(-3.80574710647333,-2.39989343748479,
5.04540747194623));
#15366=CARTESIAN_POINT('Ctrl Pts',(-3.80578578950289,-2.39376493044645,
5.04507396569907));
#15367=CARTESIAN_POINT('Ctrl Pts',(-3.80275768152815,-2.31959956136467,
5.04103586309964));
#15368=CARTESIAN_POINT('Ctrl Pts',(-3.71288602579316,-2.18496415245566,
5.03329316414794));
#15369=CARTESIAN_POINT('Ctrl Pts',(-3.4805593716682,-2.1885345970333,5.02217937509112));
#15370=CARTESIAN_POINT('Ctrl Pts',(-3.35755805936012,-2.38566174720256,
5.01106558603434));
#15371=CARTESIAN_POINT('Ctrl Pts',(-3.45646661470834,-2.59591285074103,
4.99995179697752));
#15372=CARTESIAN_POINT('Ctrl Pts',(-3.68675290044432,-2.62684270619768,
4.98883800792072));
#15373=CARTESIAN_POINT('Ctrl Pts',(-3.79782383930996,-2.49676322878239,
4.98065656624362));
#15374=CARTESIAN_POINT('Ctrl Pts',(-3.80566091748472,-2.41441389064144,
4.9761797209188));
#15375=CARTESIAN_POINT('Ctrl Pts',(-3.80552959282545,-2.40018396914357,
4.97540747194623));
#15376=CARTESIAN_POINT('Origin',(-3.6,-2.4,5.35459252805377));
#15377=CARTESIAN_POINT('',(-3.80520912268496,-2.39988380060309,5.11540747194623));
#15378=CARTESIAN_POINT('',(-3.8056388038084,-2.40016037433918,5.10959252805377));
#15379=CARTESIAN_POINT('',(-3.805475,-2.39999999999999,5.35459252805377));
#15380=CARTESIAN_POINT('Ctrl Pts',(-3.8056388038084,-2.40016037433918,5.10959252805377));
#15381=CARTESIAN_POINT('Ctrl Pts',(-3.80514403960571,-2.34250465619148,
5.10645928939915));
#15382=CARTESIAN_POINT('Ctrl Pts',(-3.74979516025411,-2.21584695448232,
5.09962145439226));
#15383=CARTESIAN_POINT('Ctrl Pts',(-3.53510505567384,-2.16596525884485,
5.0890790230331));
#15384=CARTESIAN_POINT('Ctrl Pts',(-3.36817872512274,-2.32759432716241,
5.07796523397629));
#15385=CARTESIAN_POINT('Ctrl Pts',(-3.41344101541272,-2.5554973786501,5.06685144491949));
#15386=CARTESIAN_POINT('Ctrl Pts',(-3.62946287054873,-2.64107179130501,
5.05573765586269));
#15387=CARTESIAN_POINT('Ctrl Pts',(-3.78402795903722,-2.53063333570257,
5.04665135024078));
#15388=CARTESIAN_POINT('Ctrl Pts',(-3.80522541336203,-2.43109926604885,
5.04126964097114));
#15389=CARTESIAN_POINT('Ctrl Pts',(-3.80515433874078,-2.40005255540964,
5.03959252805377));
#15390=CARTESIAN_POINT('Ctrl Pts',(-3.80520912268496,-2.39988380060309,
5.11540747194623));
#15391=CARTESIAN_POINT('Ctrl Pts',(-3.80534690105405,-2.37325776244818,
5.11396821047934));
#15392=CARTESIAN_POINT('Ctrl Pts',(-3.78816006360229,-2.27826799235566,
5.10882435266019));
#15393=CARTESIAN_POINT('Ctrl Pts',(-3.64483147519039,-2.16130911215383,
5.09997589848876));
#15394=CARTESIAN_POINT('Ctrl Pts',(-3.42377645640768,-2.23288040078699,
5.08886210943196));
#15395=CARTESIAN_POINT('Ctrl Pts',(-3.36401956629289,-2.45741970591997,
5.07774832037515));
#15396=CARTESIAN_POINT('Ctrl Pts',(-3.52025888222192,-2.62940132794335,
5.06663453131835));
#15397=CARTESIAN_POINT('Ctrl Pts',(-3.74260711073009,-2.59254976529191,
5.05585424850871));
#15398=CARTESIAN_POINT('Ctrl Pts',(-3.8053560973714,-2.46184055125472,5.04877856205134));
#15399=CARTESIAN_POINT('Ctrl Pts',(-3.80574710647333,-2.39989343748479,
5.04540747194623));
#15400=CARTESIAN_POINT('Origin',(-3.6,-2.4,5.35459252805377));
#15401=CARTESIAN_POINT('',(-3.80526708169851,-2.40022955265959,5.18540747194623));
#15402=CARTESIAN_POINT('',(-3.80565733457988,-2.39985006589819,5.17959252805377));
#15403=CARTESIAN_POINT('',(-3.805475,-2.39999999999999,5.35459252805377));
#15404=CARTESIAN_POINT('',(-3.65301702171886,-2.59851743256717,5.2));
#15405=CARTESIAN_POINT('Ctrl Pts',(-3.65301702171886,-2.59851743256717,
5.2));
#15406=CARTESIAN_POINT('Ctrl Pts',(-3.71902879097456,-2.58088801151799,
5.19629540364773));
#15407=CARTESIAN_POINT('Ctrl Pts',(-3.79249438127854,-2.51127182149751,
5.19143122762981));
#15408=CARTESIAN_POINT('Ctrl Pts',(-3.80542872863858,-2.42165306802236,
5.18656705161189));
#15409=CARTESIAN_POINT('Ctrl Pts',(-3.80526708169851,-2.40022955265959,
5.18540747194623));
#15410=CARTESIAN_POINT('',(-3.54686845990025,-2.59887322544328,5.2));
#15411=CARTESIAN_POINT('Origin',(-3.6,-2.4,5.2));
#15412=CARTESIAN_POINT('Ctrl Pts',(-3.54686838721289,-2.59887345127292,
5.2));
#15413=CARTESIAN_POINT('Ctrl Pts',(-3.61132827149734,-2.61600531405712,
5.19636770818144));
#15414=CARTESIAN_POINT('Ctrl Pts',(-3.74930830903252,-2.58406706978518,
5.18956521753271));
#15415=CARTESIAN_POINT('Ctrl Pts',(-3.80517197262043,-2.45815906273072,
5.18276272688396));
#15416=CARTESIAN_POINT('Ctrl Pts',(-3.80565733457988,-2.39985006589818,
5.17959252805377));
#15417=CARTESIAN_POINT('Origin',(-3.6,2.4,4.7));
#15418=CARTESIAN_POINT('',(-3.76675586981256,2.39987855699196,4.38714803633902));
#15419=CARTESIAN_POINT('',(-3.76680083090633,2.40009693666208,4.36785196366098));
#15420=CARTESIAN_POINT('',(-3.7666,2.4,4.7));
#15421=CARTESIAN_POINT('',(-3.76351293272515,2.3680769545372,4.3));
#15422=CARTESIAN_POINT('Ctrl Pts',(-3.76680083090633,2.40009693666208,4.36785196366098));
#15423=CARTESIAN_POINT('Ctrl Pts',(-3.76684158871352,2.40590556800081,4.36746222055426));
#15424=CARTESIAN_POINT('Ctrl Pts',(-3.76656456795221,2.41171030753034,4.36707247744754));
#15425=CARTESIAN_POINT('Ctrl Pts',(-3.76595693377405,2.41748025837345,4.36668273434082));
#15426=CARTESIAN_POINT('Ctrl Pts',(-3.76018123352143,2.47232494575256,4.36297813798855));
#15427=CARTESIAN_POINT('Ctrl Pts',(-3.72453483477909,2.52402649885475,4.35927354163629));
#15428=CARTESIAN_POINT('Ctrl Pts',(-3.67532197505843,2.54891439179576,4.35556894528402));
#15429=CARTESIAN_POINT('Ctrl Pts',(-3.62610911533777,2.57380228473677,4.35186434893175));
#15430=CARTESIAN_POINT('Ctrl Pts',(-3.56332979463879,2.5718765175166,4.34815975257948));
#15431=CARTESIAN_POINT('Ctrl Pts',(-3.51573443689162,2.5440364869014,4.34445515622722));
#15432=CARTESIAN_POINT('Ctrl Pts',(-3.46813907914445,2.5161964562862,4.34075055987495));
#15433=CARTESIAN_POINT('Ctrl Pts',(-3.43572768434908,2.46244216227597,4.33704596352268));
#15434=CARTESIAN_POINT('Ctrl Pts',(-3.43329507915076,2.40733835292718,4.33334136717041));
#15435=CARTESIAN_POINT('Ctrl Pts',(-3.43086247395245,2.35223454357839,4.32963677081815));
#15436=CARTESIAN_POINT('Ctrl Pts',(-3.45840865835118,2.29578121889103,4.32593217446588));
#15437=CARTESIAN_POINT('Ctrl Pts',(-3.50340586780517,2.26388777182752,4.32222757811361));
#15438=CARTESIAN_POINT('Ctrl Pts',(-3.54840307725917,2.23199432476401,4.31852298176134));
#15439=CARTESIAN_POINT('Ctrl Pts',(-3.61085131176843,2.22466075532434,4.31481838540907));
#15440=CARTESIAN_POINT('Ctrl Pts',(-3.66197498261058,2.24508842770105,4.3111137890568));
#15441=CARTESIAN_POINT('Ctrl Pts',(-3.71309865345273,2.26551610007776,4.30740919270453));
#15442=CARTESIAN_POINT('Ctrl Pts',(-3.75289776062778,2.31370501427083,4.30370459635227));
#15443=CARTESIAN_POINT('Ctrl Pts',(-3.76351293272515,2.3680769545372,4.3));
#15444=CARTESIAN_POINT('',(-3.60525668225574,2.5668198662348,4.3));
#15445=CARTESIAN_POINT('Origin',(-3.6,2.4,4.3));
#15446=CARTESIAN_POINT('',(-3.76634548976639,2.39993502697971,4.31714803633902));
#15447=CARTESIAN_POINT('Ctrl Pts',(-3.60525667864057,2.56682005840211,4.3));
#15448=CARTESIAN_POINT('Ctrl Pts',(-3.65930634748376,2.56504681426963,4.30363229181856));
#15449=CARTESIAN_POINT('Ctrl Pts',(-3.71251717627762,2.53457816039784,4.30726458363711));
#15450=CARTESIAN_POINT('Ctrl Pts',(-3.74128611123357,2.48878409483897,4.31089687545566));
#15451=CARTESIAN_POINT('Ctrl Pts',(-3.75778985504382,2.46251362194275,4.31298059575011));
#15452=CARTESIAN_POINT('Ctrl Pts',(-3.76624996614321,2.43119967804664,4.31506431604457));
#15453=CARTESIAN_POINT('Ctrl Pts',(-3.76634548976639,2.39993502697971,4.31714803633902));
#15454=CARTESIAN_POINT('',(-3.7666,2.4,4.2));
#15455=CARTESIAN_POINT('',(-3.7666,2.4,4.7));
#15456=CARTESIAN_POINT('Origin',(-3.6,2.4,4.2));
#15457=CARTESIAN_POINT('Ctrl Pts',(-3.76634548976639,2.39993502697971,4.31714803633902));
#15458=CARTESIAN_POINT('Ctrl Pts',(-3.7664197953026,2.37561500451544,4.31876891239683));
#15459=CARTESIAN_POINT('Ctrl Pts',(-3.76143276332865,2.35132480870382,4.32038978845465));
#15460=CARTESIAN_POINT('Ctrl Pts',(-3.75123332497294,2.32946153149726,4.32201066451247));
#15461=CARTESIAN_POINT('Ctrl Pts',(-3.72792197926853,2.27949187675561,4.32571526086474));
#15462=CARTESIAN_POINT('Ctrl Pts',(-3.67738233884271,2.24219983197054,4.329419857217));
#15463=CARTESIAN_POINT('Ctrl Pts',(-3.62274960712982,2.23467803877973,4.33312445356927));
#15464=CARTESIAN_POINT('Ctrl Pts',(-3.56811687541693,2.22715624558892,4.33682904992154));
#15465=CARTESIAN_POINT('Ctrl Pts',(-3.50939105241698,2.24940470399237,4.34053364627381));
#15466=CARTESIAN_POINT('Ctrl Pts',(-3.473445625673,2.29122843734541,4.34423824262608));
#15467=CARTESIAN_POINT('Ctrl Pts',(-3.43750019892903,2.33305217069845,4.34794283897834));
#15468=CARTESIAN_POINT('Ctrl Pts',(-3.42433516844104,2.39445117900107,4.35164743533061));
#15469=CARTESIAN_POINT('Ctrl Pts',(-3.43997694242044,2.44733227209049,4.35535203168288));
#15470=CARTESIAN_POINT('Ctrl Pts',(-3.45561871639985,2.50021336517992,4.35905662803515));
#15471=CARTESIAN_POINT('Ctrl Pts',(-3.50006729484665,2.54457654305613,4.36276122438742));
#15472=CARTESIAN_POINT('Ctrl Pts',(-3.55297985590111,2.56011554237715,4.36646582073968));
#15473=CARTESIAN_POINT('Ctrl Pts',(-3.60589241695558,2.57565454169817,4.37017041709195));
#15474=CARTESIAN_POINT('Ctrl Pts',(-3.6672689606177,2.562369362464,4.37387501344422));
#15475=CARTESIAN_POINT('Ctrl Pts',(-3.70902050221487,2.52634164219194,4.37757960979649));
#15476=CARTESIAN_POINT('Ctrl Pts',(-3.74496652897209,2.49532354447962,4.38076908531067));
#15477=CARTESIAN_POINT('Ctrl Pts',(-3.76636578927508,2.4474478468568,4.38395856082485));
#15478=CARTESIAN_POINT('Ctrl Pts',(-3.76675586981256,2.39987855699196,4.38714803633902));
#15479=CARTESIAN_POINT('Origin',(-3.6,2.4,4.7));
#15480=CARTESIAN_POINT('',(-3.76672468602162,2.4001324774977,4.45714803633902));
#15481=CARTESIAN_POINT('',(-3.7663710759754,2.40008323252274,4.43785196366098));
#15482=CARTESIAN_POINT('',(-3.7666,2.4,4.7));
#15483=CARTESIAN_POINT('Ctrl Pts',(-3.7663710759754,2.40008323252274,4.43785196366098));
#15484=CARTESIAN_POINT('Ctrl Pts',(-3.76647255964094,2.42251958309795,4.43635646533454));
#15485=CARTESIAN_POINT('Ctrl Pts',(-3.76225162287627,2.44491933914913,4.43486096700809));
#15486=CARTESIAN_POINT('Ctrl Pts',(-3.75352689637225,2.46540054190021,4.43336546868165));
#15487=CARTESIAN_POINT('Ctrl Pts',(-3.73191430783919,2.516135863806,4.42966087232938));
#15488=CARTESIAN_POINT('Ctrl Pts',(-3.6826649015976,2.55509827647583,4.42595627597711));
#15489=CARTESIAN_POINT('Ctrl Pts',(-3.62831779967194,2.56445627090432,4.42225167962485));
#15490=CARTESIAN_POINT('Ctrl Pts',(-3.57397069774627,2.57381426533281,4.41854708327258));
#15491=CARTESIAN_POINT('Ctrl Pts',(-3.51452590013653,2.55356784151996,4.41484248692031));
#15492=CARTESIAN_POINT('Ctrl Pts',(-3.47718895189484,2.51298317028118,4.41113789056804));
#15493=CARTESIAN_POINT('Ctrl Pts',(-3.43985200365314,2.4723984990424,4.40743329421577));
#15494=CARTESIAN_POINT('Ctrl Pts',(-3.42462290477948,2.41147558037768,4.40372869786351));
#15495=CARTESIAN_POINT('Ctrl Pts',(-3.43847074534366,2.35809557252044,4.40002410151124));
#15496=CARTESIAN_POINT('Ctrl Pts',(-3.45231858590785,2.30471556466319,4.39631950515897));
#15497=CARTESIAN_POINT('Ctrl Pts',(-3.49524336590988,2.25887846761341,4.3926149088067));
#15498=CARTESIAN_POINT('Ctrl Pts',(-3.54760150451765,2.24156301194163,4.38891031245443));
#15499=CARTESIAN_POINT('Ctrl Pts',(-3.59995964312543,2.22424755626985,4.38520571610216));
#15500=CARTESIAN_POINT('Ctrl Pts',(-3.66175114033895,2.23545374197608,4.3815011197499));
#15501=CARTESIAN_POINT('Ctrl Pts',(-3.70469438806425,2.2700507456572,4.37779652339763));
#15502=CARTESIAN_POINT('Ctrl Pts',(-3.74311977927038,2.30100796178371,4.37448167015208));
#15503=CARTESIAN_POINT('Ctrl Pts',(-3.76645417654063,2.35069321376496,4.37116681690653));
#15504=CARTESIAN_POINT('Ctrl Pts',(-3.76680083090633,2.40009693666208,4.36785196366098));
#15505=CARTESIAN_POINT('Ctrl Pts',(-3.76675586981256,2.39987855699196,4.38714803633902));
#15506=CARTESIAN_POINT('Ctrl Pts',(-3.76681887033176,2.39219581029783,4.38766315717711));
#15507=CARTESIAN_POINT('Ctrl Pts',(-3.76633386046459,2.38452105604489,4.3881782780152));
#15508=CARTESIAN_POINT('Ctrl Pts',(-3.76527361543791,2.37692660254772,4.38869339885329));
#15509=CARTESIAN_POINT('Ctrl Pts',(-3.75764864753156,2.32230954448549,4.39239799520556));
#15510=CARTESIAN_POINT('Ctrl Pts',(-3.72027217218665,2.27184568967097,4.39610259155783));
#15511=CARTESIAN_POINT('Ctrl Pts',(-3.67024982973388,2.2486305064859,4.3998071879101));
#15512=CARTESIAN_POINT('Ctrl Pts',(-3.62022748728111,2.22541532330082,4.40351178426237));
#15513=CARTESIAN_POINT('Ctrl Pts',(-3.55755927772049,2.22944881174518,4.40721638061463));
#15514=CARTESIAN_POINT('Ctrl Pts',(-3.51092562033288,2.25888482364762,4.4109209769669));
#15515=CARTESIAN_POINT('Ctrl Pts',(-3.46429196294527,2.28832083555005,4.41462557331917));
#15516=CARTESIAN_POINT('Ctrl Pts',(-3.43369285773067,2.34315937091056,4.41833016967144));
#15517=CARTESIAN_POINT('Ctrl Pts',(-3.43313217976425,2.39830336261017,4.42203476602371));
#15518=CARTESIAN_POINT('Ctrl Pts',(-3.43257150179783,2.45344735430978,4.42573936237597));
#15519=CARTESIAN_POINT('Ctrl Pts',(-3.46204925107959,2.5088968023485,4.42944395872824));
#15520=CARTESIAN_POINT('Ctrl Pts',(-3.5080747579799,2.53927490269551,4.43314855508051));
#15521=CARTESIAN_POINT('Ctrl Pts',(-3.55410026488021,2.56965300304252,4.43685315143278));
#15522=CARTESIAN_POINT('Ctrl Pts',(-3.61667352939907,2.57495975569782,4.44055774778505));
#15523=CARTESIAN_POINT('Ctrl Pts',(-3.66715754746926,2.55276652004746,4.44426234413731));
#15524=CARTESIAN_POINT('Ctrl Pts',(-3.71764156553946,2.53057328439709,4.44796694048958));
#15525=CARTESIAN_POINT('Ctrl Pts',(-3.756036337161,2.48088006044104,4.45167153684185));
#15526=CARTESIAN_POINT('Ctrl Pts',(-3.76477027476388,2.4264292215015,4.45537613319412));
#15527=CARTESIAN_POINT('Ctrl Pts',(-3.7661627513915,2.41774796866627,4.45596676757575));
#15528=CARTESIAN_POINT('Ctrl Pts',(-3.76680128414385,2.40894578279607,4.45655740195739));
#15529=CARTESIAN_POINT('Ctrl Pts',(-3.76672468602162,2.4001324774977,4.45714803633902));
#15530=CARTESIAN_POINT('Origin',(-3.6,2.4,4.7));
#15531=CARTESIAN_POINT('',(-3.76633791206845,2.40003802478337,4.52714803633902));
#15532=CARTESIAN_POINT('',(-3.76649857382306,2.39985687062932,4.50785196366098));
#15533=CARTESIAN_POINT('',(-3.7666,2.4,4.7));
#15534=CARTESIAN_POINT('Ctrl Pts',(-3.76649857382306,2.39985687062932,4.50785196366098));
#15535=CARTESIAN_POINT('Ctrl Pts',(-3.76617945752874,2.43880728528579,4.50525071011481));
#15536=CARTESIAN_POINT('Ctrl Pts',(-3.75254366540545,2.47795898788161,4.50264945656864));
#15537=CARTESIAN_POINT('Ctrl Pts',(-3.72758425733276,2.50756395676541,4.50004820302248));
#15538=CARTESIAN_POINT('Ctrl Pts',(-3.6920381137294,2.54972611350612,4.49634360667021));
#15539=CARTESIAN_POINT('Ctrl Pts',(-3.63352511396685,2.57252533344874,4.49263901031794));
#15540=CARTESIAN_POINT('Ctrl Pts',(-3.57882406188105,2.56552742213501,4.48893441396567));
#15541=CARTESIAN_POINT('Ctrl Pts',(-3.52412300979526,2.55852951082128,4.4852298176134));
#15542=CARTESIAN_POINT('Ctrl Pts',(-3.47323390538621,2.52173446825121,4.48152522126114));
#15543=CARTESIAN_POINT('Ctrl Pts',(-3.44944644044618,2.47198175864633,4.47782062490887));
#15544=CARTESIAN_POINT('Ctrl Pts',(-3.42565897550616,2.42222904904145,4.4741160285566));
#15545=CARTESIAN_POINT('Ctrl Pts',(-3.42897315003517,2.35951867240177,4.47041143220433));
#15546=CARTESIAN_POINT('Ctrl Pts',(-3.45787220405951,2.31255037948392,4.46670683585206));
#15547=CARTESIAN_POINT('Ctrl Pts',(-3.48677125808385,2.26558208656607,4.46300223949979));
#15548=CARTESIAN_POINT('Ctrl Pts',(-3.54125519160353,2.23435587737005,4.45929764314752));
#15549=CARTESIAN_POINT('Ctrl Pts',(-3.59638914193523,2.23316262102818,4.45559304679526));
#15550=CARTESIAN_POINT('Ctrl Pts',(-3.65152309226694,2.23196936468632,4.45188845044299));
#15551=CARTESIAN_POINT('Ctrl Pts',(-3.70730705941068,2.26080906119861,4.44818385409072));
#15552=CARTESIAN_POINT('Ctrl Pts',(-3.73821115757027,2.30648302502563,4.44447925773845));
#15553=CARTESIAN_POINT('Ctrl Pts',(-3.75663966522468,2.33371899184293,4.44227015971263));
#15554=CARTESIAN_POINT('Ctrl Pts',(-3.76622116784026,2.36694103711801,4.4400610616868));
#15555=CARTESIAN_POINT('Ctrl Pts',(-3.7663710759754,2.40008323252274,4.43785196366098));
#15556=CARTESIAN_POINT('Ctrl Pts',(-3.76672468602162,2.4001324774977,4.45714803633902));
#15557=CARTESIAN_POINT('Ctrl Pts',(-3.76632084288778,2.35366668006347,4.46026199830966));
#15558=CARTESIAN_POINT('Ctrl Pts',(-3.74603890809821,2.30689180212375,4.46337596028029));
#15559=CARTESIAN_POINT('Ctrl Pts',(-3.71156689963546,2.27590095059859,4.46648992225092));
#15560=CARTESIAN_POINT('Ctrl Pts',(-3.67055648331992,2.23903197255825,4.47019451860319));
#15561=CARTESIAN_POINT('Ctrl Pts',(-3.60946254710462,2.2245024704006,4.47389911495546));
#15562=CARTESIAN_POINT('Ctrl Pts',(-3.55624507667009,2.23896195008268,4.47760371130773));
#15563=CARTESIAN_POINT('Ctrl Pts',(-3.50302760623556,2.25342142976477,4.48130830766));
#15564=CARTESIAN_POINT('Ctrl Pts',(-3.45768660158179,2.29686989128659,4.48501290401227));
#15565=CARTESIAN_POINT('Ctrl Pts',(-3.4409726309165,2.34942290140806,4.48871750036453));
#15566=CARTESIAN_POINT('Ctrl Pts',(-3.4242586602512,2.40197591152952,4.4924220967168));
#15567=CARTESIAN_POINT('Ctrl Pts',(-3.43617172357437,2.46363347025063,4.49612669306907));
#15568=CARTESIAN_POINT('Ctrl Pts',(-3.47125973974121,2.50617764542895,4.49983128942133));
#15569=CARTESIAN_POINT('Ctrl Pts',(-3.50634775590806,2.54872182060726,4.5035358857736));
#15570=CARTESIAN_POINT('Ctrl Pts',(-3.56461072491859,2.57215261224279,4.50724048212587));
#15571=CARTESIAN_POINT('Ctrl Pts',(-3.61938426871317,2.56574678606726,4.51094507847814));
#15572=CARTESIAN_POINT('Ctrl Pts',(-3.67415781250775,2.55934095989172,4.51464967483041));
#15573=CARTESIAN_POINT('Ctrl Pts',(-3.72544193108638,2.52309851590513,4.51835427118267));
#15574=CARTESIAN_POINT('Ctrl Pts',(-3.7497661567401,2.47360601391412,4.52205886753494));
#15575=CARTESIAN_POINT('Ctrl Pts',(-3.7609045803459,2.45094266337894,4.5237552571363));
#15576=CARTESIAN_POINT('Ctrl Pts',(-3.76638989212213,2.42550096131782,4.52545164673766));
#15577=CARTESIAN_POINT('Ctrl Pts',(-3.76633791206845,2.40003802478337,4.52714803633902));
#15578=CARTESIAN_POINT('Origin',(-3.6,2.4,4.7));
#15579=CARTESIAN_POINT('',(-3.76658523827666,2.39984765670423,4.59714803633902));
#15580=CARTESIAN_POINT('',(-3.76687644222506,2.40000067112036,4.57785196366098));
#15581=CARTESIAN_POINT('',(-3.7666,2.4,4.7));
#15582=CARTESIAN_POINT('Ctrl Pts',(-3.76687644086079,2.40000067111705,4.57785196366098));
#15583=CARTESIAN_POINT('Ctrl Pts',(-3.76687973678962,2.45518344204594,4.57414495489509));
#15584=CARTESIAN_POINT('Ctrl Pts',(-3.73679497953693,2.51036312381259,4.57043794612919));
#15585=CARTESIAN_POINT('Ctrl Pts',(-3.69041339694851,2.54026106127768,4.5667309373633));
#15586=CARTESIAN_POINT('Ctrl Pts',(-3.64406199814677,2.57013954203352,4.56302634101103));
#15587=CARTESIAN_POINT('Ctrl Pts',(-3.58143498975323,2.57476917303812,4.55932174465876));
#15588=CARTESIAN_POINT('Ctrl Pts',(-3.53119397724287,2.55203117737673,4.55561714830649));
#15589=CARTESIAN_POINT('Ctrl Pts',(-3.4809529647325,2.52929318171533,4.55191255195423));
#15590=CARTESIAN_POINT('Ctrl Pts',(-3.44309794810529,2.47918755938795,4.54820795560196));
#15591=CARTESIAN_POINT('Ctrl Pts',(-3.43495349044459,2.42464543263837,4.54450335924969));
#15592=CARTESIAN_POINT('Ctrl Pts',(-3.42680903278389,2.37010330588879,4.54079876289742));
#15593=CARTESIAN_POINT('Ctrl Pts',(-3.44837513408969,2.31112467471701,4.53709416654516));
#15594=CARTESIAN_POINT('Ctrl Pts',(-3.48978194566841,2.27470144397531,4.53338957019289));
#15595=CARTESIAN_POINT('Ctrl Pts',(-3.53118875724712,2.23827821323361,4.52968497384062));
#15596=CARTESIAN_POINT('Ctrl Pts',(-3.59243627909875,2.22441038292198,4.52598037748835));
#15597=CARTESIAN_POINT('Ctrl Pts',(-3.64549423583691,2.23944464448895,4.52227578113608));
#15598=CARTESIAN_POINT('Ctrl Pts',(-3.69855219257508,2.25447890605592,4.51857118478381));
#15599=CARTESIAN_POINT('Ctrl Pts',(-3.74342058419978,2.29841525950148,4.51486658843154));
#15600=CARTESIAN_POINT('Ctrl Pts',(-3.75956513629004,2.35114598299368,4.51116199207928));
#15601=CARTESIAN_POINT('Ctrl Pts',(-3.76437348076611,2.36685081528665,4.51005864927318));
#15602=CARTESIAN_POINT('Ctrl Pts',(-3.76663392958958,2.3833357360905,4.50895530646708));
#15603=CARTESIAN_POINT('Ctrl Pts',(-3.76649857382306,2.39985687062932,4.50785196366098));
#15604=CARTESIAN_POINT('Ctrl Pts',(-3.76633791206845,2.40003802478337,4.52714803633902));
#15605=CARTESIAN_POINT('Ctrl Pts',(-3.76627637744537,2.36989468919261,4.52915624308993));
#15606=CARTESIAN_POINT('Ctrl Pts',(-3.758454818996,2.33972159536913,4.53116444984084));
#15607=CARTESIAN_POINT('Ctrl Pts',(-3.74306538301875,2.31409282238037,4.53317265659175));
#15608=CARTESIAN_POINT('Ctrl Pts',(-3.71467605091489,2.26681469283306,4.53687725294402));
#15609=CARTESIAN_POINT('Ctrl Pts',(-3.66053305397837,2.23500099373388,4.54058184929628));
#15610=CARTESIAN_POINT('Ctrl Pts',(-3.6054152417587,2.23321144482349,4.54428644564855));
#15611=CARTESIAN_POINT('Ctrl Pts',(-3.55029742953903,2.23142189591311,4.54799104200082));
#15612=CARTESIAN_POINT('Ctrl Pts',(-3.49420480203621,2.25965649719153,4.55169563835309));
#15613=CARTESIAN_POINT('Ctrl Pts',(-3.46280846829882,2.30499352330658,4.55540023470536));
#15614=CARTESIAN_POINT('Ctrl Pts',(-3.43141213456143,2.35033054942163,4.55910483105762));
#15615=CARTESIAN_POINT('Ctrl Pts',(-3.42471209458945,2.41277000037331,4.56280942740989));
#15616=CARTESIAN_POINT('Ctrl Pts',(-3.44577465966535,2.46373610736585,4.56651402376216));
#15617=CARTESIAN_POINT('Ctrl Pts',(-3.46683722474125,2.51470221435838,4.57021862011443));
#15618=CARTESIAN_POINT('Ctrl Pts',(-3.51566239486502,2.55419497739177,4.5739232164667));
#15619=CARTESIAN_POINT('Ctrl Pts',(-3.56990505407324,2.56414030953056,4.57762781281897));
#15620=CARTESIAN_POINT('Ctrl Pts',(-3.62414771328146,2.57408564166935,4.58133240917123));
#15621=CARTESIAN_POINT('Ctrl Pts',(-3.68380786157412,2.55448354291355,4.5850370055235));
#15622=CARTESIAN_POINT('Ctrl Pts',(-3.72158169378842,2.51430502490722,4.58874160187577));
#15623=CARTESIAN_POINT('Ctrl Pts',(-3.75015369954742,2.4839141225134,4.59154374669685));
#15624=CARTESIAN_POINT('Ctrl Pts',(-3.76620375341029,2.44175070750818,4.59434589151794));
#15625=CARTESIAN_POINT('Ctrl Pts',(-3.76658523827666,2.39984765670423,4.59714803633902));
#15626=CARTESIAN_POINT('Origin',(-3.6,2.4,4.7));
#15627=CARTESIAN_POINT('',(-3.76685426518066,2.40005503529171,4.66714803633902));
#15628=CARTESIAN_POINT('',(-3.76649661588353,2.40014270746765,4.64785196366098));
#15629=CARTESIAN_POINT('',(-3.7666,2.4,4.7));
#15630=CARTESIAN_POINT('Ctrl Pts',(-3.76649661588353,2.40014270746765,4.64785196366098));
#15631=CARTESIAN_POINT('Ctrl Pts',(-3.76663204639349,2.41673658143502,4.64674379602763));
#15632=CARTESIAN_POINT('Ctrl Pts',(-3.76435138934107,2.43329406659146,4.64563562839428));
#15633=CARTESIAN_POINT('Ctrl Pts',(-3.75950152904524,2.44906128711078,4.64452746076093));
#15634=CARTESIAN_POINT('Ctrl Pts',(-3.74328848128947,2.50177099082653,4.64082286440866));
#15635=CARTESIAN_POINT('Ctrl Pts',(-3.69836304459695,2.54564901270383,4.63711826805639));
#15636=CARTESIAN_POINT('Ctrl Pts',(-3.64528559981485,2.5606143272255,4.63341367170412));
#15637=CARTESIAN_POINT('Ctrl Pts',(-3.59220815503275,2.57557964174716,4.62970907535186));
#15638=CARTESIAN_POINT('Ctrl Pts',(-3.53097870216106,2.56163224891319,4.62600447899959));
#15639=CARTESIAN_POINT('Ctrl Pts',(-3.48961924750057,2.52515525214062,4.62229988264732));
#15640=CARTESIAN_POINT('Ctrl Pts',(-3.44825979284008,2.48867825536805,4.61859528629505));
#15641=CARTESIAN_POINT('Ctrl Pts',(-3.4267703363908,2.42967165465689,4.61489068994278));
#15642=CARTESIAN_POINT('Ctrl Pts',(-3.43498564975134,2.37514015541382,4.61118609359051));
#15643=CARTESIAN_POINT('Ctrl Pts',(-3.44320096311188,2.32060865617075,4.60748149723825));
#15644=CARTESIAN_POINT('Ctrl Pts',(-3.48112104628225,2.27055225839578,4.60377690088598));
#15645=CARTESIAN_POINT('Ctrl Pts',(-3.53139155817582,2.2478795563676,4.60007230453371));
#15646=CARTESIAN_POINT('Ctrl Pts',(-3.58166207006939,2.22520685433943,4.59636770818145));
#15647=CARTESIAN_POINT('Ctrl Pts',(-3.64428301068616,2.22991784805805,4.59266311182918));
#15648=CARTESIAN_POINT('Ctrl Pts',(-3.69059555147242,2.25985652453919,4.58895851547691));
#15649=CARTESIAN_POINT('Ctrl Pts',(-3.73687793377613,2.28977570511195,4.58525633153827));
#15650=CARTESIAN_POINT('Ctrl Pts',(-3.76687314922176,2.34488972287695,4.58155414759963));
#15651=CARTESIAN_POINT('Ctrl Pts',(-3.76687644086079,2.40000067111705,4.57785196366098));
#15652=CARTESIAN_POINT('Ctrl Pts',(-3.76658523827666,2.39984765670423,4.59714803633902));
#15653=CARTESIAN_POINT('Ctrl Pts',(-3.76670809830844,2.38635246827757,4.5980504878702));
#15654=CARTESIAN_POINT('Ctrl Pts',(-3.76520579898216,2.37288428508147,4.59895293940139));
#15655=CARTESIAN_POINT('Ctrl Pts',(-3.76197323034856,2.35984505467766,4.59985539093257));
#15656=CARTESIAN_POINT('Ctrl Pts',(-3.74870341855848,2.30631853971129,4.60355998728484));
#15657=CARTESIAN_POINT('Ctrl Pts',(-3.70627627884239,2.26002044703541,4.60726458363711));
#15658=CARTESIAN_POINT('Ctrl Pts',(-3.65410883226945,2.24213936129044,4.61096917998938));
#15659=CARTESIAN_POINT('Ctrl Pts',(-3.60194138569651,2.22425827554546,4.61467377634165));
#15660=CARTESIAN_POINT('Ctrl Pts',(-3.54003363226672,2.23479419673139,4.61837837269391));
#15661=CARTESIAN_POINT('Ctrl Pts',(-3.49671800637814,2.26892530077511,4.62208296904618));
#15662=CARTESIAN_POINT('Ctrl Pts',(-3.45340238048956,2.30305640481884,4.62578756539845));
#15663=CARTESIAN_POINT('Ctrl Pts',(-3.42867888214219,2.36078269172036,4.62949216175072));
#15664=CARTESIAN_POINT('Ctrl Pts',(-3.43386236054643,2.4156853989487,4.63319675810298));
#15665=CARTESIAN_POINT('Ctrl Pts',(-3.43904583895067,2.47058810617705,4.63690135445525));
#15666=CARTESIAN_POINT('Ctrl Pts',(-3.47413629410653,2.52266723373221,4.64060595080752));
#15667=CARTESIAN_POINT('Ctrl Pts',(-3.52307438023553,2.54808847357993,4.64431054715979));
#15668=CARTESIAN_POINT('Ctrl Pts',(-3.57201246636453,2.57350971342765,4.64801514351206));
#15669=CARTESIAN_POINT('Ctrl Pts',(-3.63479818346667,2.57227306556792,4.65171973986433));
#15670=CARTESIAN_POINT('Ctrl Pts',(-3.68269729209092,2.54494448890598,4.65542433621659));
#15671=CARTESIAN_POINT('Ctrl Pts',(-3.73059640071517,2.51761591224403,4.65912893256886));
#15672=CARTESIAN_POINT('Ctrl Pts',(-3.76360890086153,2.46419540677987,4.66283352892113));
#15673=CARTESIAN_POINT('Ctrl Pts',(-3.76662643464441,2.40913116975406,4.6665381252734));
#15674=CARTESIAN_POINT('Ctrl Pts',(-3.76679203318471,2.406109312194,4.66674142896194));
#15675=CARTESIAN_POINT('Ctrl Pts',(-3.76686729650514,2.4030825042416,4.66694473265048));
#15676=CARTESIAN_POINT('Ctrl Pts',(-3.76685426518066,2.40005503529171,4.66714803633902));
#15677=CARTESIAN_POINT('Origin',(-3.6,2.4,4.7));
#15678=CARTESIAN_POINT('',(-3.76642275699063,2.40011764661364,4.73714803633902));
#15679=CARTESIAN_POINT('',(-3.76637219462709,2.39991574862477,4.71785196366098));
#15680=CARTESIAN_POINT('',(-3.7666,2.4,4.7));
#15681=CARTESIAN_POINT('Ctrl Pts',(-3.76637219462709,2.39991574862477,4.71785196366098));
#15682=CARTESIAN_POINT('Ctrl Pts',(-3.76622008929152,2.43312978877493,4.7156380408079));
#15683=CARTESIAN_POINT('Ctrl Pts',(-3.75659374130514,2.46642503349729,4.71342411795483));
#15684=CARTESIAN_POINT('Ctrl Pts',(-3.73808953093009,2.49369647329664,4.71121019510175));
#15685=CARTESIAN_POINT('Ctrl Pts',(-3.70712610771876,2.53933025690454,4.70750559874949));
#15686=CARTESIAN_POINT('Ctrl Pts',(-3.65130473898255,2.56809743365675,4.70380100239722));
#15687=CARTESIAN_POINT('Ctrl Pts',(-3.59617239065227,2.56683254199167,4.70009640604495));
#15688=CARTESIAN_POINT('Ctrl Pts',(-3.541040042322,2.56556765032658,4.69639180969268));
#15689=CARTESIAN_POINT('Ctrl Pts',(-3.48659671439765,2.53427069024418,4.69268721334041));
#15690=CARTESIAN_POINT('Ctrl Pts',(-3.45775870461848,2.48726489299201,4.68898261698815));
#15691=CARTESIAN_POINT('Ctrl Pts',(-3.4289206948393,2.44025909573984,4.68527802063588));
#15692=CARTESIAN_POINT('Ctrl Pts',(-3.4256880032053,2.3775444613179,4.68157342428361));
#15693=CARTESIAN_POINT('Ctrl Pts',(-3.44954008937339,2.32782269778556,4.67786882793134));
#15694=CARTESIAN_POINT('Ctrl Pts',(-3.47339217554148,2.27810093425323,4.67416423157907));
#15695=CARTESIAN_POINT('Ctrl Pts',(-3.52432903951166,2.2413720416105,4.67045963522681));
#15696=CARTESIAN_POINT('Ctrl Pts',(-3.57903913665629,2.23444520584228,4.66675503887454));
#15697=CARTESIAN_POINT('Ctrl Pts',(-3.63374923380092,2.22751837007406,4.66305044252227));
#15698=CARTESIAN_POINT('Ctrl Pts',(-3.69223256411999,2.25039359118035,4.65934584617));
#15699=CARTESIAN_POINT('Ctrl Pts',(-3.72772389987002,2.29260189451059,4.65564124981773));
#15700=CARTESIAN_POINT('Ctrl Pts',(-3.75259860001318,2.32218429445987,4.65304482109882));
#15701=CARTESIAN_POINT('Ctrl Pts',(-3.766179303182,2.36126338124449,4.6504483923799));
#15702=CARTESIAN_POINT('Ctrl Pts',(-3.76649661588353,2.40014270746765,4.64785196366098));
#15703=CARTESIAN_POINT('Ctrl Pts',(-3.76685426518066,2.40005503529171,4.66714803633902));
#15704=CARTESIAN_POINT('Ctrl Pts',(-3.76662983993221,2.34791601656576,4.67064932900275));
#15705=CARTESIAN_POINT('Ctrl Pts',(-3.7402175145738,2.29558094816933,4.67415062166648));
#15706=CARTESIAN_POINT('Ctrl Pts',(-3.69804051189557,2.26495998737175,4.6776519143302));
#15707=CARTESIAN_POINT('Ctrl Pts',(-3.65341448794446,2.23256101060272,4.68135651068247));
#15708=CARTESIAN_POINT('Ctrl Pts',(-3.59113987262282,2.22447102565214,4.68506110703474));
#15709=CARTESIAN_POINT('Ctrl Pts',(-3.53971699675369,2.24439246000598,4.68876570338701));
#15710=CARTESIAN_POINT('Ctrl Pts',(-3.48829412088457,2.26431389435981,4.69247029973927));
#15711=CARTESIAN_POINT('Ctrl Pts',(-3.44772298446796,2.31224674801807,4.69617489609154));
#15712=CARTESIAN_POINT('Ctrl Pts',(-3.43657119813891,2.36625427870627,4.69987949244381));
#15713=CARTESIAN_POINT('Ctrl Pts',(-3.42541941180987,2.42026180939447,4.70358408879608));
#15714=CARTESIAN_POINT('Ctrl Pts',(-3.44368697556839,2.48034401711262,4.70728868514835));
#15715=CARTESIAN_POINT('Ctrl Pts',(-3.48301363527625,2.51900393880922,4.71099328150062));
#15716=CARTESIAN_POINT('Ctrl Pts',(-3.52234029498412,2.55766386050582,4.71469787785288));
#15717=CARTESIAN_POINT('Ctrl Pts',(-3.58272605064134,2.57490149618086,4.71840247420515));
#15718=CARTESIAN_POINT('Ctrl Pts',(-3.63653501876085,2.56282794412363,4.72210707055742));
#15719=CARTESIAN_POINT('Ctrl Pts',(-3.69034398688037,2.5507543920664,4.72581166690969));
#15720=CARTESIAN_POINT('Ctrl Pts',(-3.73757616746218,2.50936965227689,4.72951626326196));
#15721=CARTESIAN_POINT('Ctrl Pts',(-3.75661548523835,2.45761368558721,4.73322085961422));
#15722=CARTESIAN_POINT('Ctrl Pts',(-3.76334323265594,2.43932515890074,4.73452991852249));
#15723=CARTESIAN_POINT('Ctrl Pts',(-3.76655071173719,2.4197416412828,4.73583897743076));
#15724=CARTESIAN_POINT('Ctrl Pts',(-3.76642275699063,2.40011764661364,4.73714803633902));
#15725=CARTESIAN_POINT('Origin',(-3.6,2.4,4.7));
#15726=CARTESIAN_POINT('',(-3.76642910764821,2.39987935508533,4.80714803633902));
#15727=CARTESIAN_POINT('',(-3.76680408556428,2.39990252619421,4.78785196366098));
#15728=CARTESIAN_POINT('',(-3.7666,2.4,4.7));
#15729=CARTESIAN_POINT('Ctrl Pts',(-3.76680408556428,2.39990252619421,4.78785196366098));
#15730=CARTESIAN_POINT('Ctrl Pts',(-3.76646018913848,2.44937641051311,4.78453228558818));
#15731=CARTESIAN_POINT('Ctrl Pts',(-3.74304696564969,2.49913297683607,4.78121260751538));
#15732=CARTESIAN_POINT('Ctrl Pts',(-3.70452480260444,2.53008579208055,4.77789292944258));
#15733=CARTESIAN_POINT('Ctrl Pts',(-3.66153597610701,2.56462760123568,4.77418833309031));
#15734=CARTESIAN_POINT('Ctrl Pts',(-3.59973129998187,2.5757522439241,4.77048373673804));
#15735=CARTESIAN_POINT('Ctrl Pts',(-3.54739603471406,2.55836846433844,4.76677914038578));
#15736=CARTESIAN_POINT('Ctrl Pts',(-3.49506076944624,2.54098468475278,4.76307454403351));
#15737=CARTESIAN_POINT('Ctrl Pts',(-3.45219491503573,2.49509248289304,4.75936994768124));
#15738=CARTESIAN_POINT('Ctrl Pts',(-3.43841627281944,2.44169468516681,4.75566535132897));
#15739=CARTESIAN_POINT('Ctrl Pts',(-3.42463763060315,2.38829688744059,4.7519607549767));
#15740=CARTESIAN_POINT('Ctrl Pts',(-3.43994620058106,2.32739349384788,4.74825615862443));
#15741=CARTESIAN_POINT('Ctrl Pts',(-3.4773359288973,2.28685728781211,4.74455156227217));
#15742=CARTESIAN_POINT('Ctrl Pts',(-3.51472565721353,2.24632108177635,4.7408469659199));
#15743=CARTESIAN_POINT('Ctrl Pts',(-3.57419654386808,2.22615206329753,4.73714236956763));
#15744=CARTESIAN_POINT('Ctrl Pts',(-3.62853140036063,2.23558069804861,4.73343777321536));
#15745=CARTESIAN_POINT('Ctrl Pts',(-3.68286625685319,2.24500933279969,4.7297331768631));
#15746=CARTESIAN_POINT('Ctrl Pts',(-3.73206508318374,2.28403562078066,4.72602858051083));
#15747=CARTESIAN_POINT('Ctrl Pts',(-3.7536117575058,2.33479896000292,4.72232398415856));
#15748=CARTESIAN_POINT('Ctrl Pts',(-3.76228181312143,2.35522535934946,4.72083331065937));
#15749=CARTESIAN_POINT('Ctrl Pts',(-3.76647460984564,2.37755214666628,4.71934263716017));
#15750=CARTESIAN_POINT('Ctrl Pts',(-3.76637219462709,2.39991574862477,4.71785196366098));
#15751=CARTESIAN_POINT('Ctrl Pts',(-3.76642275699063,2.40011764661364,4.73714803633902));
#15752=CARTESIAN_POINT('Ctrl Pts',(-3.76618860374924,2.36420634137441,4.73954357378302));
#15753=CARTESIAN_POINT('Ctrl Pts',(-3.75478479252022,2.32815948710566,4.74193911122702));
#15754=CARTESIAN_POINT('Ctrl Pts',(-3.73334402193678,2.29966496724918,4.74433464867103));
#15755=CARTESIAN_POINT('Ctrl Pts',(-3.70018678588852,2.25559940919069,4.74803924502329));
#15756=CARTESIAN_POINT('Ctrl Pts',(-3.64302585882149,2.22959548666357,4.75174384137557));
#15757=CARTESIAN_POINT('Ctrl Pts',(-3.58802126313241,2.23355404226464,4.75544843772783));
#15758=CARTESIAN_POINT('Ctrl Pts',(-3.53301666744333,2.2375125978657,4.7591530340801));
#15759=CARTESIAN_POINT('Ctrl Pts',(-3.48016840313221,2.27143363159494,4.76285763043237));
#15760=CARTESIAN_POINT('Ctrl Pts',(-3.45366277803107,2.31979299002082,4.76656222678463));
#15761=CARTESIAN_POINT('Ctrl Pts',(-3.42715715292992,2.36815234844671,4.7702668231369));
#15762=CARTESIAN_POINT('Ctrl Pts',(-3.42699416703876,2.43095003156924,4.77397141948917));
#15763=CARTESIAN_POINT('Ctrl Pts',(-3.45324841177486,2.47944632362031,4.77767601584144));
#15764=CARTESIAN_POINT('Ctrl Pts',(-3.47950265651095,2.52794261567138,4.78138061219371));
#15765=CARTESIAN_POINT('Ctrl Pts',(-3.53217413187432,2.56213751665099,4.78508520854598));
#15766=CARTESIAN_POINT('Ctrl Pts',(-3.58715743849732,2.56638153622754,4.78878980489824));
#15767=CARTESIAN_POINT('Ctrl Pts',(-3.64214074512033,2.57062555580409,4.79249440125051));
#15768=CARTESIAN_POINT('Ctrl Pts',(-3.69943588300298,2.54491869397758,4.79619899760278));
#15769=CARTESIAN_POINT('Ctrl Pts',(-3.73282140740775,2.50102584183074,4.79990359395505));
#15770=CARTESIAN_POINT('Ctrl Pts',(-3.754583518131,2.4724146061108,4.80231840808304));
#15771=CARTESIAN_POINT('Ctrl Pts',(-3.76618645992471,2.43607616275589,4.80473322221103));
#15772=CARTESIAN_POINT('Ctrl Pts',(-3.76642910764821,2.39987935508533,4.80714803633902));
#15773=CARTESIAN_POINT('Origin',(-3.6,2.4,4.7));
#15774=CARTESIAN_POINT('',(-3.76685809662611,2.39994994258553,4.87714803633902));
#15775=CARTESIAN_POINT('',(-3.7666675037778,2.40014587506062,4.85785196366098));
#15776=CARTESIAN_POINT('',(-3.7666,2.4,4.7));
#15777=CARTESIAN_POINT('Ctrl Pts',(-3.7666675037778,2.40014587506062,4.85785196366098));
#15778=CARTESIAN_POINT('Ctrl Pts',(-3.76676616841865,2.41091157707528,4.85713112672072));
#15779=CARTESIAN_POINT('Ctrl Pts',(-3.76581236284584,2.4216598706667,4.85641028978047));
#15780=CARTESIAN_POINT('Ctrl Pts',(-3.76374257225157,2.43218878210118,4.85568945284021));
#15781=CARTESIAN_POINT('Ctrl Pts',(-3.7531053001346,2.48630000298229,4.85198485648794));
#15782=CARTESIAN_POINT('Ctrl Pts',(-3.71299219510172,2.53461681652064,4.84828026013567));
#15783=CARTESIAN_POINT('Ctrl Pts',(-3.66176124712798,2.5550267590254,4.8445756637834));
#15784=CARTESIAN_POINT('Ctrl Pts',(-3.61053029915424,2.57543670153016,4.84087106743113));
#15785=CARTESIAN_POINT('Ctrl Pts',(-3.54818150823965,2.56793977300133,4.83716647107887));
#15786=CARTESIAN_POINT('Ctrl Pts',(-3.50324915208796,2.53596698529063,4.8334618747266));
#15787=CARTESIAN_POINT('Ctrl Pts',(-3.45831679593627,2.50399419757992,4.82975727837433));
#15788=CARTESIAN_POINT('Ctrl Pts',(-3.43080087454749,2.44754555068734,4.82605268202206));
#15789=CARTESIAN_POINT('Ctrl Pts',(-3.43329420537107,2.39245508794886,4.8223480856698));
#15790=CARTESIAN_POINT('Ctrl Pts',(-3.43578753619466,2.33736462521039,4.81864348931753));
#15791=CARTESIAN_POINT('Ctrl Pts',(-3.46829011923061,2.28363234662601,4.81493889296526));
#15792=CARTESIAN_POINT('Ctrl Pts',(-3.51592696305034,2.25584913417262,4.81123429661299));
#15793=CARTESIAN_POINT('Ctrl Pts',(-3.56356380687008,2.22806592171924,4.80752970026072));
#15794=CARTESIAN_POINT('Ctrl Pts',(-3.62633491147359,2.22623177539684,4.80382510390846));
#15795=CARTESIAN_POINT('Ctrl Pts',(-3.67551272490272,2.25118610267019,4.80012050755619));
#15796=CARTESIAN_POINT('Ctrl Pts',(-3.72469053833185,2.27614042994354,4.79641591120392));
#15797=CARTESIAN_POINT('Ctrl Pts',(-3.76027506058658,2.32788323081264,4.79271131485165));
#15798=CARTESIAN_POINT('Ctrl Pts',(-3.76598083327909,2.38273411905811,4.78900671849938));
#15799=CARTESIAN_POINT('Ctrl Pts',(-3.76657367957029,2.38843328504628,4.78862180021992));
#15800=CARTESIAN_POINT('Ctrl Pts',(-3.76684396052131,2.39416600535905,4.78823688194045));
#15801=CARTESIAN_POINT('Ctrl Pts',(-3.76680408556428,2.39990252619421,4.78785196366098));
#15802=CARTESIAN_POINT('Ctrl Pts',(-3.76642910764821,2.39987935508533,4.80714803633902));
#15803=CARTESIAN_POINT('Ctrl Pts',(-3.76655870881167,2.38054619044631,4.8084378185633));
#15804=CARTESIAN_POINT('Ctrl Pts',(-3.76344748981416,2.36125343108011,4.80972760078758));
#15805=CARTESIAN_POINT('Ctrl Pts',(-3.75691243582065,2.3432000486953,4.81101738301185));
#15806=CARTESIAN_POINT('Ctrl Pts',(-3.73814202890189,2.29134595017387,4.81472197936412));
#15807=CARTESIAN_POINT('Ctrl Pts',(-3.6911253041375,2.24971659559817,4.81842657571639));
#15808=CARTESIAN_POINT('Ctrl Pts',(-3.63737973221885,2.2373638951443,4.82213117206866));
#15809=CARTESIAN_POINT('Ctrl Pts',(-3.58363416030021,2.22501119469043,4.82583576842093));
#15810=CARTESIAN_POINT('Ctrl Pts',(-3.52315974122731,2.24193514835838,4.82954036477319));
#15811=CARTESIAN_POINT('Ctrl Pts',(-3.48363293580215,2.28039041278662,4.83324496112546));
#15812=CARTESIAN_POINT('Ctrl Pts',(-3.44410613037699,2.31884567721486,4.83694955747773));
#15813=CARTESIAN_POINT('Ctrl Pts',(-3.42552693859956,2.3788322524034,4.84065415383));
#15814=CARTESIAN_POINT('Ctrl Pts',(-3.436398232938,2.43289694207027,4.84435875018227));
#15815=CARTESIAN_POINT('Ctrl Pts',(-3.44726952727644,2.48696163173715,4.84806334653453));
#15816=CARTESIAN_POINT('Ctrl Pts',(-3.48759130773074,2.53510443588236,4.8517679428868));
#15817=CARTESIAN_POINT('Ctrl Pts',(-3.53891008283594,2.5552925272004,4.85547253923907));
#15818=CARTESIAN_POINT('Ctrl Pts',(-3.59022885794113,2.57548061851844,4.85917713559134));
#15819=CARTESIAN_POINT('Ctrl Pts',(-3.65254462769722,2.56771399700931,4.86288173194361));
#15820=CARTESIAN_POINT('Ctrl Pts',(-3.6973382267209,2.53554710104677,4.86658632829587));
#15821=CARTESIAN_POINT('Ctrl Pts',(-3.73990668943618,2.50497810589362,4.87010689764359));
#15822=CARTESIAN_POINT('Ctrl Pts',(-3.76665058188897,2.4523728080809,4.8736274669913));
#15823=CARTESIAN_POINT('Ctrl Pts',(-3.76685809662611,2.39994994258553,4.87714803633902));
#15824=CARTESIAN_POINT('Origin',(-3.6,2.4,4.7));
#15825=CARTESIAN_POINT('',(-3.76657659596252,2.40015219042981,4.94714803633902));
#15826=CARTESIAN_POINT('',(-3.76633013671136,2.4000063325357,4.92785196366098));
#15827=CARTESIAN_POINT('',(-3.7666,2.4,4.7));
#15828=CARTESIAN_POINT('Ctrl Pts',(-3.76633013671136,2.4000063325357,4.92785196366098));
#15829=CARTESIAN_POINT('Ctrl Pts',(-3.76633943338483,2.42742681836579,4.926025371501));
#15830=CARTESIAN_POINT('Ctrl Pts',(-3.75993532163491,2.454843216144,4.92419877934102));
#15831=CARTESIAN_POINT('Ctrl Pts',(-3.74709395519472,2.478810633836,4.92237218718103));
#15832=CARTESIAN_POINT('Ctrl Pts',(-3.72104978380566,2.52742006625356,4.91866759082877));
#15833=CARTESIAN_POINT('Ctrl Pts',(-3.66852675119931,2.56184254018683,4.9149629944765));
#15834=CARTESIAN_POINT('Ctrl Pts',(-3.61356232107187,2.56632441524918,4.91125839812423));
#15835=CARTESIAN_POINT('Ctrl Pts',(-3.55859789094443,2.57080629031153,4.90755380177196));
#15836=CARTESIAN_POINT('Ctrl Pts',(-3.5011920632959,2.54534756650297,4.90384920541969));
#15837=CARTESIAN_POINT('Ctrl Pts',(-3.46761694066379,2.50159957313644,4.90014460906742));
#15838=CARTESIAN_POINT('Ctrl Pts',(-3.43404181803167,2.45785157976992,4.89644001271516));
#15839=CARTESIAN_POINT('Ctrl Pts',(-3.42429740041597,2.39581431684543,4.89273541636289));
#15840=CARTESIAN_POINT('Ctrl Pts',(-3.44284327579263,2.34387948951498,4.88903082001062));
#15841=CARTESIAN_POINT('Ctrl Pts',(-3.46138915116929,2.29194466218454,4.88532622365835));
#15842=CARTESIAN_POINT('Ctrl Pts',(-3.50822531953831,2.25011227044814,4.88162162730609));
#15843=CARTESIAN_POINT('Ctrl Pts',(-3.56191694286671,2.23752714559004,4.87791703095382));
#15844=CARTESIAN_POINT('Ctrl Pts',(-3.61560856619511,2.22494202073194,4.87421243460155));
#15845=CARTESIAN_POINT('Ctrl Pts',(-3.6761556444829,2.24160416275214,4.87050783824928));
#15846=CARTESIAN_POINT('Ctrl Pts',(-3.71584846402625,2.27988804787417,4.86680324189701));
#15847=CARTESIAN_POINT('Ctrl Pts',(-3.7478178913646,2.31072268995097,4.863819482485));
#15848=CARTESIAN_POINT('Ctrl Pts',(-3.76625910135787,2.35558341867251,4.86083572307299));
#15849=CARTESIAN_POINT('Ctrl Pts',(-3.7666675037778,2.40014587506062,4.85785196366098));
#15850=CARTESIAN_POINT('Ctrl Pts',(-3.76685809662611,2.39994994258553,4.87714803633902));
#15851=CARTESIAN_POINT('Ctrl Pts',(-3.76686894382487,2.39720969748472,4.87733206334357));
#15852=CARTESIAN_POINT('Ctrl Pts',(-3.76680728418873,2.39446995085397,4.87751609034812));
#15853=CARTESIAN_POINT('Ctrl Pts',(-3.76667158779769,2.39173387609673,4.87770011735268));
#15854=CARTESIAN_POINT('Ctrl Pts',(-3.76393992155949,2.33665471752516,4.88140471370494));
#15855=CARTESIAN_POINT('Ctrl Pts',(-3.73120516079181,2.28306357079796,4.88510931005722));
#15856=CARTESIAN_POINT('Ctrl Pts',(-3.68344855437882,2.25548672809881,4.88881390640948));
#15857=CARTESIAN_POINT('Ctrl Pts',(-3.63569194796583,2.22790988539967,4.89251850276175));
#15858=CARTESIAN_POINT('Ctrl Pts',(-3.57291349590753,2.22634734672859,4.89622309911402));
#15859=CARTESIAN_POINT('Ctrl Pts',(-3.52384411276617,2.25151421676554,4.89992769546629));
#15860=CARTESIAN_POINT('Ctrl Pts',(-3.47477472962482,2.27668108680249,4.90363229181855));
#15861=CARTESIAN_POINT('Ctrl Pts',(-3.43941441540042,2.32857736554749,4.90733688817082));
#15862=CARTESIAN_POINT('Ctrl Pts',(-3.43394601840489,2.38345242676704,4.91104148452309));
#15863=CARTESIAN_POINT('Ctrl Pts',(-3.42847762140937,2.4383274879866,4.91474608087536));
#15864=CARTESIAN_POINT('Ctrl Pts',(-3.45290114164273,2.49618133168073,4.91845067722763));
#15865=CARTESIAN_POINT('Ctrl Pts',(-3.49603901657836,2.530536818217,4.9221552735799));
#15866=CARTESIAN_POINT('Ctrl Pts',(-3.539176891514,2.56489230475327,4.92585986993216));
#15867=CARTESIAN_POINT('Ctrl Pts',(-3.60102912115191,2.5757494341317,4.92956446628443));
#15868=CARTESIAN_POINT('Ctrl Pts',(-3.65328868187437,2.55813937955255,4.9332690626367));
#15869=CARTESIAN_POINT('Ctrl Pts',(-3.70554824259683,2.54052932497339,4.93697365898897));
#15870=CARTESIAN_POINT('Ctrl Pts',(-3.74821513440384,2.49445208643666,4.94067825534123));
#15871=CARTESIAN_POINT('Ctrl Pts',(-3.76176261231807,2.4409951733855,4.9443828516935));
#15872=CARTESIAN_POINT('Ctrl Pts',(-3.76513331494005,2.42769473782655,4.94530457990868));
#15873=CARTESIAN_POINT('Ctrl Pts',(-3.7667013875235,2.41393746536136,4.94622630812385));
#15874=CARTESIAN_POINT('Ctrl Pts',(-3.76657659596252,2.40015219042981,4.94714803633902));
#15875=CARTESIAN_POINT('Origin',(-3.6,2.4,4.7));
#15876=CARTESIAN_POINT('',(-3.76634000089015,2.39995738785102,5.01714803633902));
#15877=CARTESIAN_POINT('',(-3.76664425875303,2.39985083704439,4.99785196366098));
#15878=CARTESIAN_POINT('',(-3.7666,2.4,4.7));
#15879=CARTESIAN_POINT('Ctrl Pts',(-3.76664425875303,2.39985083704439,4.99785196366098));
#15880=CARTESIAN_POINT('Ctrl Pts',(-3.76623994328637,2.44366117230771,4.99491961628127));
#15881=CARTESIAN_POINT('Ctrl Pts',(-3.74849621432459,2.48776127465667,4.99198726890157));
#15882=CARTESIAN_POINT('Ctrl Pts',(-3.71750016303509,2.5184966637895,4.98905492152186));
#15883=CARTESIAN_POINT('Ctrl Pts',(-3.67834114001603,2.55732637791376,4.98535032516959));
#15884=CARTESIAN_POINT('Ctrl Pts',(-3.61803053064114,2.57482512236184,4.98164572881732));
#15885=CARTESIAN_POINT('Ctrl Pts',(-3.56416982715023,2.56298449736068,4.97794113246505));
#15886=CARTESIAN_POINT('Ctrl Pts',(-3.51030912365932,2.55114387235952,4.97423653611279));
#15887=CARTESIAN_POINT('Ctrl Pts',(-3.46289832605237,2.50996387790913,4.97053193976052));
#15888=CARTESIAN_POINT('Ctrl Pts',(-3.44363525475417,2.45829077205198,4.96682734340825));
#15889=CARTESIAN_POINT('Ctrl Pts',(-3.42437218345597,2.40661766619482,4.96312274705598));
#15890=CARTESIAN_POINT('Ctrl Pts',(-3.4332568384665,2.34445144893089,4.95941815070372));
#15891=CARTESIAN_POINT('Ctrl Pts',(-3.4662231070096,2.30024284205961,4.95571355435145));
#15892=CARTESIAN_POINT('Ctrl Pts',(-3.4991893755527,2.25603423518832,4.95200895799918));
#15893=CARTESIAN_POINT('Ctrl Pts',(-3.55623725762836,2.22978323870968,4.94830436164691));
#15894=CARTESIAN_POINT('Ctrl Pts',(-3.61125846653673,2.23350377003431,4.94459976529464));
#15895=CARTESIAN_POINT('Ctrl Pts',(-3.66627967544511,2.23722430135893,4.94089516894237));
#15896=CARTESIAN_POINT('Ctrl Pts',(-3.71927421118621,2.27091636048683,4.9371905725901));
#15897=CARTESIAN_POINT('Ctrl Pts',(-3.74598882397087,2.31916058550171,4.93348597623784));
#15898=CARTESIAN_POINT('Ctrl Pts',(-3.75953150177818,2.3436174623693,4.93160797204555));
#15899=CARTESIAN_POINT('Ctrl Pts',(-3.76632057836981,2.37181405816179,4.92972996785327));
#15900=CARTESIAN_POINT('Ctrl Pts',(-3.76633013671136,2.4000063325357,4.92785196366098));
#15901=CARTESIAN_POINT('Ctrl Pts',(-3.76657659596252,2.40015219042981,4.94714803633902));
#15902=CARTESIAN_POINT('Ctrl Pts',(-3.76619982713509,2.35853189310505,4.94993090447612));
#15903=CARTESIAN_POINT('Ctrl Pts',(-3.7503917908276,2.31665633988757,4.95271377261321));
#15904=CARTESIAN_POINT('Ctrl Pts',(-3.72217338919013,2.28632762005297,4.95549664075031));
#15905=CARTESIAN_POINT('Ctrl Pts',(-3.68460862412651,2.24595356733716,4.95920123710258));
#15906=CARTESIAN_POINT('Ctrl Pts',(-3.62505102997782,2.22604204947114,4.96290583345484));
#15907=CARTESIAN_POINT('Ctrl Pts',(-3.57075747740423,2.23570568531624,4.96661042980711));
#15908=CARTESIAN_POINT('Ctrl Pts',(-3.51646392483064,2.24536932116134,4.97031502615938));
#15909=CARTESIAN_POINT('Ctrl Pts',(-3.46743441383215,2.28460811071757,4.97401962251165));
#15910=CARTESIAN_POINT('Ctrl Pts',(-3.44610757816651,2.33546419983794,4.97772421886392));
#15911=CARTESIAN_POINT('Ctrl Pts',(-3.42478074250087,2.38632028895831,4.98142881521618));
#15912=CARTESIAN_POINT('Ctrl Pts',(-3.43115658216808,2.44879367764282,4.98513341156845));
#15913=CARTESIAN_POINT('Ctrl Pts',(-3.46231715792478,2.49429306452592,4.98883800792072));
#15914=CARTESIAN_POINT('Ctrl Pts',(-3.49347773368148,2.53979245140902,4.99254260427299));
#15915=CARTESIAN_POINT('Ctrl Pts',(-3.54942304552767,2.56831783649071,4.99624720062526));
#15916=CARTESIAN_POINT('Ctrl Pts',(-3.60454940439799,2.56681441711196,4.99995179697753));
#15917=CARTESIAN_POINT('Ctrl Pts',(-3.6596757632683,2.5653109977332,5.00365639332979));
#15918=CARTESIAN_POINT('Ctrl Pts',(-3.71398316916273,2.533778773894,5.00736098968206));
#15919=CARTESIAN_POINT('Ctrl Pts',(-3.7426175295644,2.48664864348361,5.01106558603433));
#15920=CARTESIAN_POINT('Ctrl Pts',(-3.75828878922747,2.46085485932866,5.01309306946923));
#15921=CARTESIAN_POINT('Ctrl Pts',(-3.76627033413891,2.43038911475947,5.01512055290412));
#15922=CARTESIAN_POINT('Ctrl Pts',(-3.76634000089015,2.39995738785102,5.01714803633902));
#15923=CARTESIAN_POINT('Origin',(-3.6,2.4,4.7));
#15924=CARTESIAN_POINT('',(-3.76673280722786,2.39986996770474,5.08714803633902));
#15925=CARTESIAN_POINT('',(-3.76682061973634,2.40008640134019,5.06785196366098));
#15926=CARTESIAN_POINT('',(-3.7666,2.4,4.7));
#15927=CARTESIAN_POINT('Ctrl Pts',(-3.76682061973634,2.40008640134019,5.06785196366098));
#15928=CARTESIAN_POINT('Ctrl Pts',(-3.76685198409984,2.40505542063702,5.06751845741382));
#15929=CARTESIAN_POINT('Ctrl Pts',(-3.76664920930319,2.41002184448446,5.06718495116665));
#15930=CARTESIAN_POINT('Ctrl Pts',(-3.76620395659798,2.41496643342036,5.06685144491949));
#15931=CARTESIAN_POINT('Ctrl Pts',(-3.76125807758801,2.46989106014367,5.06314684856722));
#15932=CARTESIAN_POINT('Ctrl Pts',(-3.7263932711654,2.5221215151067,5.05944225221495));
#15933=CARTESIAN_POINT('Ctrl Pts',(-3.67756562981921,2.54775425401002,5.05573765586269));
#15934=CARTESIAN_POINT('Ctrl Pts',(-3.62873798847301,2.57338699291335,5.05203305951042));
#15935=CARTESIAN_POINT('Ctrl Pts',(-3.56594751220322,2.57242201575698,5.04832846315815));
#15936=CARTESIAN_POINT('Ctrl Pts',(-3.51793061046379,2.54530094002895,5.04462386680588));
#15937=CARTESIAN_POINT('Ctrl Pts',(-3.46991370872435,2.51817986430092,5.04091927045361));
#15938=CARTESIAN_POINT('Ctrl Pts',(-3.43667038151527,2.46490269000124,5.03721467410135));
#15939=CARTESIAN_POINT('Ctrl Pts',(-3.4334146300602,2.40985202293434,5.03351007774908));
#15940=CARTESIAN_POINT('Ctrl Pts',(-3.43015887860513,2.35480135586744,5.02980548139681));
#15941=CARTESIAN_POINT('Ctrl Pts',(-3.45689070290407,2.29797719603331,5.02610088504454));
#15942=CARTESIAN_POINT('Ctrl Pts',(-3.50137612997721,2.26538543995573,5.02239628869227));
#15943=CARTESIAN_POINT('Ctrl Pts',(-3.54586155705034,2.23279368387816,5.01869169234));
#15944=CARTESIAN_POINT('Ctrl Pts',(-3.60810058689768,2.22443433155712,5.01498709598773));
#15945=CARTESIAN_POINT('Ctrl Pts',(-3.65960917559394,2.24413308920132,5.01128249963547));
#15946=CARTESIAN_POINT('Ctrl Pts',(-3.7111177642902,2.26383184684551,5.0075779032832));
#15947=CARTESIAN_POINT('Ctrl Pts',(-3.75189591183539,2.31158871445493,5.00387330693093));
#15948=CARTESIAN_POINT('Ctrl Pts',(-3.76328126727638,2.36554749015986,5.00016871057866));
#15949=CARTESIAN_POINT('Ctrl Pts',(-3.76565462410273,2.37679557365843,4.9993964616061));
#15950=CARTESIAN_POINT('Ctrl Pts',(-3.76675073733939,2.38831315681292,4.99862421263354));
#15951=CARTESIAN_POINT('Ctrl Pts',(-3.76664425875303,2.39985083704439,4.99785196366098));
#15952=CARTESIAN_POINT('Ctrl Pts',(-3.76634000089015,2.39995738785102,5.01714803633902));
#15953=CARTESIAN_POINT('Ctrl Pts',(-3.76639762849214,2.37478458425737,5.01882514925639));
#15954=CARTESIAN_POINT('Ctrl Pts',(-3.76104161363815,2.34963505698934,5.02050226217376));
#15955=CARTESIAN_POINT('Ctrl Pts',(-3.75014621226255,2.32717238066401,5.02217937509113));
#15956=CARTESIAN_POINT('Ctrl Pts',(-3.72607921965016,2.27755428523638,5.0258839714434));
#15957=CARTESIAN_POINT('Ctrl Pts',(-3.67498391951647,2.2410461313627,5.02958856779567));
#15958=CARTESIAN_POINT('Ctrl Pts',(-3.62024436463387,2.23435607004762,5.03329316414794));
#15959=CARTESIAN_POINT('Ctrl Pts',(-3.56550480975127,2.22766600873255,5.03699776050021));
#15960=CARTESIAN_POINT('Ctrl Pts',(-3.50712100011975,2.25079403997609,5.04070235685247));
#15961=CARTESIAN_POINT('Ctrl Pts',(-3.47181261940603,2.29315551442515,5.04440695320474));
#15962=CARTESIAN_POINT('Ctrl Pts',(-3.43650423869231,2.33551698887421,5.04811154955701));
#15963=CARTESIAN_POINT('Ctrl Pts',(-3.42427128689639,2.39711190652879,5.05181614590928));
#15964=CARTESIAN_POINT('Ctrl Pts',(-3.44071223950815,2.44975095341954,5.05552074226154));
#15965=CARTESIAN_POINT('Ctrl Pts',(-3.45715319211991,2.50239000031029,5.05922533861381));
#15966=CARTESIAN_POINT('Ctrl Pts',(-3.50226804913935,2.54607317643722,5.06292993496608));
#15967=CARTESIAN_POINT('Ctrl Pts',(-3.55540974897266,2.56080872993518,5.06663453131835));
#15968=CARTESIAN_POINT('Ctrl Pts',(-3.60855144880598,2.57554428343315,5.07033912767062));
#15969=CARTESIAN_POINT('Ctrl Pts',(-3.66971999145316,2.56133221430215,5.07404372402289));
#15970=CARTESIAN_POINT('Ctrl Pts',(-3.71092122942369,2.52467655355957,5.07774832037516));
#15971=CARTESIAN_POINT('Ctrl Pts',(-3.74576802490479,2.49367427362722,5.08088155902978));
#15972=CARTESIAN_POINT('Ctrl Pts',(-3.76633165033452,2.44661746651941,5.0840147976844));
#15973=CARTESIAN_POINT('Ctrl Pts',(-3.76673280722786,2.39986996770474,5.08714803633902));
#15974=CARTESIAN_POINT('Origin',(-3.6,2.4,4.7));
#15975=CARTESIAN_POINT('',(-3.76674783252531,2.40012156540224,5.15714803633902));
#15976=CARTESIAN_POINT('',(-3.76638442018051,2.4000942147675,5.13785196366098));
#15977=CARTESIAN_POINT('',(-3.7666,2.4,4.7));
#15978=CARTESIAN_POINT('',(-3.47309291201476,2.50793586530485,5.2));
#15979=CARTESIAN_POINT('Ctrl Pts',(-3.76674783252531,2.40012156540224,5.15714803633902));
#15980=CARTESIAN_POINT('Ctrl Pts',(-3.76635429688688,2.35284438834095,5.16031823516921));
#15981=CARTESIAN_POINT('Ctrl Pts',(-3.74524547308137,2.30526839815283,5.1634884339994));
#15982=CARTESIAN_POINT('Ctrl Pts',(-3.70967617106781,2.27424023606977,5.16665863282959));
#15983=CARTESIAN_POINT('Ctrl Pts',(-3.66811098429235,2.23798168503636,5.17036322918186));
#15984=CARTESIAN_POINT('Ctrl Pts',(-3.60679923783928,2.22432008207827,5.17406782553412));
#15985=CARTESIAN_POINT('Ctrl Pts',(-3.55380863333633,2.23961508023379,5.17777242188639));
#15986=CARTESIAN_POINT('Ctrl Pts',(-3.50081802883339,2.2549100783893,5.18147701823866));
#15987=CARTESIAN_POINT('Ctrl Pts',(-3.45614856628056,2.29916167765842,5.18518161459093));
#15988=CARTESIAN_POINT('Ctrl Pts',(-3.44024447629705,2.35186821788708,5.1888862109432));
#15989=CARTESIAN_POINT('Ctrl Pts',(-3.42434038631354,2.40457475811575,5.19259080729547));
#15990=CARTESIAN_POINT('Ctrl Pts',(-3.43720166889934,2.46573623930395,5.19629540364773));
#15991=CARTESIAN_POINT('Ctrl Pts',(-3.47309291201476,2.50793586530485,5.2));
#15992=CARTESIAN_POINT('',(-3.72714753727462,2.50812032359617,5.2));
#15993=CARTESIAN_POINT('Origin',(-3.6,2.4,5.2));
#15994=CARTESIAN_POINT('Ctrl Pts',(-3.72714768981588,2.50812044061668,5.2));
#15995=CARTESIAN_POINT('Ctrl Pts',(-3.69206189497277,2.54927257104909,5.19636770818145));
#15996=CARTESIAN_POINT('Ctrl Pts',(-3.63506413165932,2.57187758396405,5.19273541636289));
#15997=CARTESIAN_POINT('Ctrl Pts',(-3.58132375091077,2.56581791151438,5.18910312454434));
#15998=CARTESIAN_POINT('Ctrl Pts',(-3.52651361217864,2.55963761500343,5.18539852819207));
#15999=CARTESIAN_POINT('Ctrl Pts',(-3.475091829903,2.5236400741886,5.1816939318398));
#16000=CARTESIAN_POINT('Ctrl Pts',(-3.45055836676857,2.47425895866487,5.17798933548753));
#16001=CARTESIAN_POINT('Ctrl Pts',(-3.42602490363414,2.42487784314114,5.17428473913526));
#16002=CARTESIAN_POINT('Ctrl Pts',(-3.42837975964092,2.3621131529085,5.17058014278299));
#16003=CARTESIAN_POINT('Ctrl Pts',(-3.4565619363393,2.31470980183002,5.16687554643073));
#16004=CARTESIAN_POINT('Ctrl Pts',(-3.48474411303769,2.26730645075154,5.16317095007846));
#16005=CARTESIAN_POINT('Ctrl Pts',(-3.53875361042767,2.23526443882722,5.15946635372619));
#16006=CARTESIAN_POINT('Ctrl Pts',(-3.59386432951576,2.23323784347702,5.15576175737392));
#16007=CARTESIAN_POINT('Ctrl Pts',(-3.64897504860385,2.23121124812682,5.15205716102166));
#16008=CARTESIAN_POINT('Ctrl Pts',(-3.70518698939006,2.25920006935074,5.14835256466939));
#16009=CARTESIAN_POINT('Ctrl Pts',(-3.73677860664843,2.30440012364175,5.14464796831712));
#16010=CARTESIAN_POINT('Ctrl Pts',(-3.75609666072391,2.3320396422478,5.14238263343174));
#16011=CARTESIAN_POINT('Ctrl Pts',(-3.76620859139621,2.36611484945711,5.14011729854636));
#16012=CARTESIAN_POINT('Ctrl Pts',(-3.76638442018051,2.4000942147675,5.13785196366098));
#16013=CARTESIAN_POINT('Origin',(-3.6,2.4,5.35459252805377));
#16014=CARTESIAN_POINT('',(-3.80572269346025,2.40011955618633,4.34540747194623));
#16015=CARTESIAN_POINT('',(-3.8051611014991,2.39991986595833,4.33959252805377));
#16016=CARTESIAN_POINT('',(-3.805475,2.40000000000001,5.35459252805377));
#16017=CARTESIAN_POINT('',(-3.41173724903364,2.31767678198965,4.3));
#16018=CARTESIAN_POINT('Ctrl Pts',(-3.8051611014991,2.39991986595833,4.33959252805377));
#16019=CARTESIAN_POINT('Ctrl Pts',(-3.80504328807488,2.43847991504582,4.33750880775932));
#16020=CARTESIAN_POINT('Ctrl Pts',(-3.77605831390311,2.54576383181508,4.33172049111259));
#16021=CARTESIAN_POINT('Ctrl Pts',(-3.60297477126067,2.64299057240655,4.32222757811361));
#16022=CARTESIAN_POINT('Ctrl Pts',(-3.39749753058122,2.53388381093044,4.3111137890568));
#16023=CARTESIAN_POINT('Ctrl Pts',(-3.38436282049399,2.380278625644,4.30370459635227));
#16024=CARTESIAN_POINT('Ctrl Pts',(-3.41173724903364,2.31767678198965,4.3));
#16025=CARTESIAN_POINT('',(-3.47764162137361,2.23446466486417,4.3));
#16026=CARTESIAN_POINT('Origin',(-3.6,2.4,4.3));
#16027=CARTESIAN_POINT('Ctrl Pts',(-3.80572269346025,2.40011955618633,4.34540747194623));
#16028=CARTESIAN_POINT('Ctrl Pts',(-3.80577296183019,2.40728359294699,4.34501772883951));
#16029=CARTESIAN_POINT('Ctrl Pts',(-3.80218372831243,2.48249299452007,4.34092338938053));
#16030=CARTESIAN_POINT('Ctrl Pts',(-3.70962996035205,2.61673302206395,4.33312445356927));
#16031=CARTESIAN_POINT('Ctrl Pts',(-3.47734458963256,2.60960762555316,4.32201066451247));
#16032=CARTESIAN_POINT('Ctrl Pts',(-3.35820165688085,2.41200908723629,4.31096917998938));
#16033=CARTESIAN_POINT('Ctrl Pts',(-3.42405717417692,2.27417969332383,4.30363229181855));
#16034=CARTESIAN_POINT('Ctrl Pts',(-3.477641490197,2.23446446733471,4.3));
#16035=CARTESIAN_POINT('Origin',(-3.6,2.4,5.35459252805377));
#16036=CARTESIAN_POINT('',(-3.8051926580795,2.40010265427736,4.41540747194623));
#16037=CARTESIAN_POINT('',(-3.80566724099481,2.39985021907517,4.40959252805377));
#16038=CARTESIAN_POINT('',(-3.805475,2.40000000000001,5.35459252805377));
#16039=CARTESIAN_POINT('Ctrl Pts',(-3.80566724099481,2.39985021907517,4.40959252805377));
#16040=CARTESIAN_POINT('Ctrl Pts',(-3.80518613776288,2.45851948579172,4.40640305253959));
#16041=CARTESIAN_POINT('Ctrl Pts',(-3.74813828696622,2.58615032985374,4.39950898067314));
#16042=CARTESIAN_POINT('Ctrl Pts',(-3.53156902199863,2.63302754596983,4.38891031245443));
#16043=CARTESIAN_POINT('Ctrl Pts',(-3.36710794775451,2.46888245639993,4.37779652339763));
#16044=CARTESIAN_POINT('Ctrl Pts',(-3.41581895566904,2.24170428297288,4.36668273434082));
#16045=CARTESIAN_POINT('Ctrl Pts',(-3.63310626324856,2.15938431915927,4.35556894528402));
#16046=CARTESIAN_POINT('Ctrl Pts',(-3.78504422722635,2.27149586782626,4.34653887652167));
#16047=CARTESIAN_POINT('Ctrl Pts',(-3.80525274573711,2.36992492828818,4.34121340411158));
#16048=CARTESIAN_POINT('Ctrl Pts',(-3.8051611014991,2.39991986595833,4.33959252805377));
#16049=CARTESIAN_POINT('Ctrl Pts',(-3.8051926580795,2.40010265427736,4.41540747194623));
#16050=CARTESIAN_POINT('Ctrl Pts',(-3.80531782228225,2.42777437777342,4.41391197361979));
#16051=CARTESIAN_POINT('Ctrl Pts',(-3.78721617252902,2.52383659362796,4.40871187894108));
#16052=CARTESIAN_POINT('Ctrl Pts',(-3.64121277856108,2.63934345799643,4.3998071879101));
#16053=CARTESIAN_POINT('Ctrl Pts',(-3.4212652433475,2.56443108225311,4.38869339885329));
#16054=CARTESIAN_POINT('Ctrl Pts',(-3.36491712045917,2.33901445477475,4.3775796097965));
#16055=CARTESIAN_POINT('Ctrl Pts',(-3.52374009472539,2.16941582002738,4.36646582073968));
#16056=CARTESIAN_POINT('Ctrl Pts',(-3.7443527804805,2.20942499341216,4.3557417747896));
#16057=CARTESIAN_POINT('Ctrl Pts',(-3.80529514960796,2.33918780371163,4.34872232519178));
#16058=CARTESIAN_POINT('Ctrl Pts',(-3.80572269346025,2.40011955618633,4.34540747194623));
#16059=CARTESIAN_POINT('Origin',(-3.6,2.4,5.35459252805377));
#16060=CARTESIAN_POINT('',(-3.80534990670044,2.39982347234431,4.48540747194623));
#16061=CARTESIAN_POINT('',(-3.80562878067403,2.40016339023914,4.47959252805377));
#16062=CARTESIAN_POINT('',(-3.805475,2.40000000000001,5.35459252805377));
#16063=CARTESIAN_POINT('Ctrl Pts',(-3.80562878067403,2.40016339023914,4.47959252805377));
#16064=CARTESIAN_POINT('Ctrl Pts',(-3.80572325245773,2.41103322160878,4.47900189367213));
#16065=CARTESIAN_POINT('Ctrl Pts',(-3.79999615010417,2.4899814340984,4.47470666293823));
#16066=CARTESIAN_POINT('Ctrl Pts',(-3.69773850528383,2.62233049702197,4.46670683585206));
#16067=CARTESIAN_POINT('Ctrl Pts',(-3.46621554861493,2.60269535293104,4.45559304679526));
#16068=CARTESIAN_POINT('Ctrl Pts',(-3.35714699158608,2.39753073103871,4.44447925773845));
#16069=CARTESIAN_POINT('Ctrl Pts',(-3.47036459922058,2.19462650439043,4.43336546868165));
#16070=CARTESIAN_POINT('Ctrl Pts',(-3.70223885539349,2.17970247609322,4.42225167962484));
#16071=CARTESIAN_POINT('Ctrl Pts',(-3.80084479883202,2.31283530811152,4.41432736608222));
#16072=CARTESIAN_POINT('Ctrl Pts',(-3.80574494226542,2.39037475462753,4.41010764889186));
#16073=CARTESIAN_POINT('Ctrl Pts',(-3.80566724099481,2.39985021907517,4.40959252805377));
#16074=CARTESIAN_POINT('Ctrl Pts',(-3.80534990670044,2.39982347234431,4.48540747194623));
#16075=CARTESIAN_POINT('Ctrl Pts',(-3.804956326745,2.4478627067473,4.48280621840006));
#16076=CARTESIAN_POINT('Ctrl Pts',(-3.76418777279803,2.56491922132028,4.47650036850163));
#16077=CARTESIAN_POINT('Ctrl Pts',(-3.56918135753979,2.64090223654315,4.46648992225092));
#16078=CARTESIAN_POINT('Ctrl Pts',(-3.38089014394226,2.50475947474088,4.45537613319412));
#16079=CARTESIAN_POINT('Ctrl Pts',(-3.3931526891646,2.27272919910994,4.44426234413731));
#16080=CARTESIAN_POINT('Ctrl Pts',(-3.59474487835949,2.15719128792351,4.43314855508051));
#16081=CARTESIAN_POINT('Ctrl Pts',(-3.77337323137102,2.2495401787091,4.42353026435015));
#16082=CARTESIAN_POINT('Ctrl Pts',(-3.80500776987982,2.35922694839029,4.41761656997206));
#16083=CARTESIAN_POINT('Ctrl Pts',(-3.8051926580795,2.40010265427736,4.41540747194623));
#16084=CARTESIAN_POINT('Origin',(-3.6,2.4,5.35459252805377));
#16085=CARTESIAN_POINT('',(-3.80581594817644,2.40000082772184,4.55540747194624));
#16086=CARTESIAN_POINT('',(-3.80515175559583,2.40004689761323,4.54959252805377));
#16087=CARTESIAN_POINT('',(-3.805475,2.40000000000001,5.35459252805377));
#16088=CARTESIAN_POINT('Ctrl Pts',(-3.80515175559583,2.40004689761323,4.54959252805377));
#16089=CARTESIAN_POINT('Ctrl Pts',(-3.80521586484871,2.43145144073697,4.54789613845241));
#16090=CARTESIAN_POINT('Ctrl Pts',(-3.78367650680796,2.53135422698056,4.54249515249878));
#16091=CARTESIAN_POINT('Ctrl Pts',(-3.62821111800771,2.64122148806661,4.53338957019289));
#16092=CARTESIAN_POINT('Ctrl Pts',(-3.41263638408026,2.55452685581013,4.52227578113608));
#16093=CARTESIAN_POINT('Ctrl Pts',(-3.36855769224962,2.32639203807509,4.51116199207928));
#16094=CARTESIAN_POINT('Ctrl Pts',(-3.536320770243,2.1656314264689,4.50004820302247));
#16095=CARTESIAN_POINT('Ctrl Pts',(-3.75035693400944,2.21653400528296,4.48952504834731));
#16096=CARTESIAN_POINT('Ctrl Pts',(-3.80513070343558,2.34285510855967,4.4827064900244));
#16097=CARTESIAN_POINT('Ctrl Pts',(-3.80562878067403,2.40016339023914,4.47959252805377));
#16098=CARTESIAN_POINT('Ctrl Pts',(-3.80581594649383,2.40000082771776,4.55540747194623));
#16099=CARTESIAN_POINT('Ctrl Pts',(-3.80581594913922,2.4000451187351,4.55540505953261));
#16100=CARTESIAN_POINT('Ctrl Pts',(-3.80579587912807,2.46810441912583,4.55169805076672));
#16101=CARTESIAN_POINT('Ctrl Pts',(-3.73158417538336,2.60413054603043,4.54428644564855));
#16102=CARTESIAN_POINT('Ctrl Pts',(-3.49986236476522,2.62126031969194,4.53317265659175));
#16103=CARTESIAN_POINT('Ctrl Pts',(-3.35979766713961,2.43586801331045,4.52205886753494));
#16104=CARTESIAN_POINT('Ctrl Pts',(-3.43959288921302,2.2176453079079,4.51094507847814));
#16105=CARTESIAN_POINT('Ctrl Pts',(-3.66621055822496,2.16633391955349,4.49983128942134));
#16106=CARTESIAN_POINT('Ctrl Pts',(-3.79336822071197,2.29085017253336,4.4913187539107));
#16107=CARTESIAN_POINT('Ctrl Pts',(-3.80551684683325,2.37944724113564,4.48651081475233));
#16108=CARTESIAN_POINT('Ctrl Pts',(-3.80534990670044,2.39982347234431,4.48540747194623));
#16109=CARTESIAN_POINT('Origin',(-3.6,2.4,5.35459252805377));
#16110=CARTESIAN_POINT('',(-3.80534749188876,2.40017600730441,4.62540747194623));
#16111=CARTESIAN_POINT('',(-3.80545679372687,2.39981210841117,4.61959252805377));
#16112=CARTESIAN_POINT('',(-3.805475,2.40000000000001,5.35459252805377));
#16113=CARTESIAN_POINT('Ctrl Pts',(-3.80545679372687,2.39981210841117,4.61959252805377));
#16114=CARTESIAN_POINT('Ctrl Pts',(-3.80498629190864,2.45149295693423,4.61679038323268));
#16115=CARTESIAN_POINT('Ctrl Pts',(-3.75902063818539,2.5722445101987,4.61028364205933));
#16116=CARTESIAN_POINT('Ctrl Pts',(-3.55620097488638,2.63888348417682,4.60007230453371));
#16117=CARTESIAN_POINT('Ctrl Pts',(-3.3755463800872,2.4927590756963,4.58895851547691));
#16118=CARTESIAN_POINT('Ctrl Pts',(-3.40033672906513,2.26173123324197,4.5778447264201));
#16119=CARTESIAN_POINT('Ctrl Pts',(-3.60788113427776,2.15726236113484,4.5667309373633));
#16120=CARTESIAN_POINT('Ctrl Pts',(-3.77763371313004,2.25700670057819,4.55731353790785));
#16121=CARTESIAN_POINT('Ctrl Pts',(-3.80507586227844,2.36286981549731,4.55160073480468));
#16122=CARTESIAN_POINT('Ctrl Pts',(-3.80515175559583,2.40004689761323,4.54959252805377));
#16123=CARTESIAN_POINT('Ctrl Pts',(-3.80534749188876,2.40017600730441,4.62540747194623));
#16124=CARTESIAN_POINT('Ctrl Pts',(-3.80551452420589,2.42064195120264,4.62429930431288));
#16125=CARTESIAN_POINT('Ctrl Pts',(-3.79329841012664,2.50933048388748,4.61948654032726));
#16126=CARTESIAN_POINT('Ctrl Pts',(-3.66590691767206,2.63375190534549,4.61096917998937));
#16127=CARTESIAN_POINT('Ctrl Pts',(-3.43935610442817,2.58214613327058,4.59985539093257));
#16128=CARTESIAN_POINT('Ctrl Pts',(-3.35984447062414,2.36381993973287,4.58874160187577));
#16129=CARTESIAN_POINT('Ctrl Pts',(-3.50014991641224,2.17860976567263,4.57762781281897));
#16130=CARTESIAN_POINT('Ctrl Pts',(-3.73179898227351,2.19603680019893,4.56651643617579));
#16131=CARTESIAN_POINT('Ctrl Pts',(-3.80581188677276,2.33203010689162,4.55910965588488));
#16132=CARTESIAN_POINT('Ctrl Pts',(-3.80581594649383,2.40000082771776,4.55540747194623));
#16133=CARTESIAN_POINT('Origin',(-3.6,2.4,5.35459252805377));
#16134=CARTESIAN_POINT('',(-3.80519403776112,2.3998960891277,4.69540747194623));
#16135=CARTESIAN_POINT('',(-3.80578859626649,2.40006787741036,4.68959252805377));
#16136=CARTESIAN_POINT('',(-3.805475,2.40000000000001,5.35459252805377));
#16137=CARTESIAN_POINT('Ctrl Pts',(-3.80578859626649,2.40006787741036,4.68959252805377));
#16138=CARTESIAN_POINT('Ctrl Pts',(-3.80580466836371,2.40380178606869,4.68938922436523));
#16139=CARTESIAN_POINT('Ctrl Pts',(-3.8040203778982,2.4755592442775,4.68548132432442));
#16140=CARTESIAN_POINT('Ctrl Pts',(-3.7203544535977,2.61094662622203,4.67786882793133));
#16141=CARTESIAN_POINT('Ctrl Pts',(-3.48804541599454,2.61552226041731,4.66675503887454));
#16142=CARTESIAN_POINT('Ctrl Pts',(-3.35820967878295,2.42282792546417,4.65564124981773));
#16143=CARTESIAN_POINT('Ctrl Pts',(-3.44968736466998,2.20923893144694,4.64452746076093));
#16144=CARTESIAN_POINT('Ctrl Pts',(-3.67874791033599,2.17025570685489,4.63341367170413));
#16145=CARTESIAN_POINT('Ctrl Pts',(-3.79614945128685,2.2983686897146,4.62510202746841));
#16146=CARTESIAN_POINT('Ctrl Pts',(-3.80560832232849,2.38316790767908,4.62049497958495));
#16147=CARTESIAN_POINT('Ctrl Pts',(-3.80545679372687,2.39981210841117,4.61959252805377));
#16148=CARTESIAN_POINT('Ctrl Pts',(-3.80519403776112,2.3998960891277,4.69540747194623));
#16149=CARTESIAN_POINT('Ctrl Pts',(-3.80500643965891,2.44086040425288,4.69319354909316));
#16150=CARTESIAN_POINT('Ctrl Pts',(-3.77326722861529,2.55063877508332,4.68727502988781));
#16151=CARTESIAN_POINT('Ctrl Pts',(-3.59442944478611,2.64280165560495,4.6776519143302));
#16152=CARTESIAN_POINT('Ctrl Pts',(-3.39298749751263,2.52700196401557,4.6665381252734));
#16153=CARTESIAN_POINT('Ctrl Pts',(-3.38102644144724,2.29495593446246,4.65542433621659));
#16154=CARTESIAN_POINT('Ctrl Pts',(-3.56949436685434,2.15905792937668,4.64431054715979));
#16155=CARTESIAN_POINT('Ctrl Pts',(-3.76430796130134,2.23525748954489,4.63430492573634));
#16156=CARTESIAN_POINT('Ctrl Pts',(-3.80495613638248,2.352224449347,4.62800390066515));
#16157=CARTESIAN_POINT('Ctrl Pts',(-3.80534749188876,2.40017600730441,4.62540747194623));
#16158=CARTESIAN_POINT('Origin',(-3.6,2.4,5.35459252805377));
#16159=CARTESIAN_POINT('',(-3.80572670757095,2.39987978133106,4.76540747194623));
#16160=CARTESIAN_POINT('',(-3.8052563985153,2.4001450986671,4.75959252805377));
#16161=CARTESIAN_POINT('',(-3.805475,2.40000000000001,5.35459252805377));
#16162=CARTESIAN_POINT('Ctrl Pts',(-3.8052563985153,2.4001450986671,4.75959252805377));
#16163=CARTESIAN_POINT('Ctrl Pts',(-3.80541421064946,2.4243482217442,4.7582834691455));
#16164=CARTESIAN_POINT('Ctrl Pts',(-3.79026314769432,2.51685423684082,4.75326981388497));
#16165=CARTESIAN_POINT('Ctrl Pts',(-3.65317165905879,2.6369735181158,4.74455156227217));
#16166=CARTESIAN_POINT('Ctrl Pts',(-3.42974255082951,2.57319374878213,4.73343777321536));
#16167=CARTESIAN_POINT('Ctrl Pts',(-3.36215201667677,2.35088777703746,4.72232398415856));
#16168=CARTESIAN_POINT('Ctrl Pts',(-3.51226643903938,2.1735347799409,4.71121019510176));
#16169=CARTESIAN_POINT('Ctrl Pts',(-3.73846936695489,2.20292040156477,4.70029970973349));
#16170=CARTESIAN_POINT('Ctrl Pts',(-3.80551180288158,2.33576256604952,4.6930938207175));
#16171=CARTESIAN_POINT('Ctrl Pts',(-3.80578859626649,2.40006787741036,4.68959252805377));
#16172=CARTESIAN_POINT('Ctrl Pts',(-3.80572670757095,2.39987978133106,4.76540747194623));
#16173=CARTESIAN_POINT('Ctrl Pts',(-3.80530256520545,2.46089806692785,4.76208779387343));
#16174=CARTESIAN_POINT('Ctrl Pts',(-3.74420122965308,2.59074745124221,4.75506351944836));
#16175=CARTESIAN_POINT('Ctrl Pts',(-3.52344221510783,2.63048336300545,4.74433464867103));
#16176=CARTESIAN_POINT('Ctrl Pts',(-3.36483726729874,2.46068083880743,4.73322085961422));
#16177=CARTESIAN_POINT('Ctrl Pts',(-3.42147943565789,2.23533645468145,4.72210707055742));
#16178=CARTESIAN_POINT('Ctrl Pts',(-3.64152350112028,2.16071048099716,4.71099328150062));
#16179=CARTESIAN_POINT('Ctrl Pts',(-3.7872979195691,2.27634402063526,4.70209341529689));
#16180=CARTESIAN_POINT('Ctrl Pts',(-3.80532035088855,2.37231408965339,4.69689814544543));
#16181=CARTESIAN_POINT('Ctrl Pts',(-3.80519403776112,2.3998960891277,4.69540747194623));
#16182=CARTESIAN_POINT('Origin',(-3.6,2.4,5.35459252805377));
#16183=CARTESIAN_POINT('',(-3.80555825533459,2.40017991403412,4.83540747194623));
#16184=CARTESIAN_POINT('',(-3.80526423105652,2.39985120339831,4.82959252805377));
#16185=CARTESIAN_POINT('',(-3.805475,2.40000000000001,5.35459252805377));
#16186=CARTESIAN_POINT('Ctrl Pts',(-3.80526423105652,2.39985120339831,4.82959252805377));
#16187=CARTESIAN_POINT('Ctrl Pts',(-3.80496496310342,2.44449429497159,4.82717771392578));
#16188=CARTESIAN_POINT('Ctrl Pts',(-3.76870077292898,2.55806758042747,4.82105830344552));
#16189=CARTESIAN_POINT('Ctrl Pts',(-3.58130943065524,2.64214527918755,4.81123429661299));
#16190=CARTESIAN_POINT('Ctrl Pts',(-3.38642339103422,2.51562311930547,4.80012050755619));
#16191=CARTESIAN_POINT('Ctrl Pts',(-3.38702644372307,2.28326980706774,4.78900671849939));
#16192=CARTESIAN_POINT('Ctrl Pts',(-3.58256660775658,2.15776096423133,4.77789292944257));
#16193=CARTESIAN_POINT('Ctrl Pts',(-3.76915215745557,2.24264335554317,4.76808819929404));
#16194=CARTESIAN_POINT('Ctrl Pts',(-3.80496760717513,2.35585412961529,4.76198806549777));
#16195=CARTESIAN_POINT('Ctrl Pts',(-3.8052563985153,2.4001450986671,4.75959252805377));
#16196=CARTESIAN_POINT('Ctrl Pts',(-3.80555825533459,2.40017991403412,4.83540747194623));
#16197=CARTESIAN_POINT('Ctrl Pts',(-3.80567994271202,2.41345772088563,4.83468663500598));
#16198=CARTESIAN_POINT('Ctrl Pts',(-3.79845785744155,2.49484232907173,4.83026120171345));
#16199=CARTESIAN_POINT('Ctrl Pts',(-3.68988494016744,2.62561997380774,4.82213117206865));
#16200=CARTESIAN_POINT('Ctrl Pts',(-3.45919254257122,2.59788111325323,4.81101738301186));
#16201=CARTESIAN_POINT('Ctrl Pts',(-3.35738280762477,2.38901942561361,4.79990359395505));
#16202=CARTESIAN_POINT('Ctrl Pts',(-3.47764334032546,2.19020838223802,4.78878980489825));
#16203=CARTESIAN_POINT('Ctrl Pts',(-3.70989831124516,2.18342198579874,4.77767601584144));
#16204=CARTESIAN_POINT('Ctrl Pts',(-3.8022342613798,2.31768599661427,4.76988190485744));
#16205=CARTESIAN_POINT('Ctrl Pts',(-3.80577588708354,2.39280468157954,4.7657923902257));
#16206=CARTESIAN_POINT('Ctrl Pts',(-3.80572670757095,2.39987978133106,4.76540747194623));
#16207=CARTESIAN_POINT('Origin',(-3.6,2.4,5.35459252805377));
#16208=CARTESIAN_POINT('',(-3.80514216591097,2.40000781019071,4.90540747194623));
#16209=CARTESIAN_POINT('',(-3.8057933217542,2.39993826202139,4.89959252805377));
#16210=CARTESIAN_POINT('',(-3.805475,2.40000000000001,5.35459252805377));
#16211=CARTESIAN_POINT('Ctrl Pts',(-3.8057933217542,2.39993826202139,4.89959252805377));
#16212=CARTESIAN_POINT('Ctrl Pts',(-3.80553738483576,2.46459365390411,4.89607195870605));
#16213=CARTESIAN_POINT('Ctrl Pts',(-3.73784442289473,2.59774586534896,4.88884679300607));
#16214=CARTESIAN_POINT('Ctrl Pts',(-3.51109208760397,2.62600676257303,4.87791703095382));
#16215=CARTESIAN_POINT('Ctrl Pts',(-3.36190028978558,2.44787694237367,4.86680324189701));
#16216=CARTESIAN_POINT('Ctrl Pts',(-3.43064385696086,2.2259248138587,4.85568945284022));
#16217=CARTESIAN_POINT('Ctrl Pts',(-3.65440102248913,2.16330567736551,4.8445756637834));
#16218=CARTESIAN_POINT('Ctrl Pts',(-3.7905654137645,2.28386779123864,4.83587668885459));
#16219=CARTESIAN_POINT('Ctrl Pts',(-3.80542407378798,2.37600677360117,4.83088231027805));
#16220=CARTESIAN_POINT('Ctrl Pts',(-3.80526423105652,2.39985120339831,4.82959252805377));
#16221=CARTESIAN_POINT('Ctrl Pts',(-3.80514216591096,2.40000781019071,4.90540747194623));
#16222=CARTESIAN_POINT('Ctrl Pts',(-3.80515363190124,2.43382668369574,4.90358087978625));
#16223=CARTESIAN_POINT('Ctrl Pts',(-3.78123591260341,2.53621991664107,4.898049691274));
#16224=CARTESIAN_POINT('Ctrl Pts',(-3.6197380796992,2.64206214751696,4.88881390640948));
#16225=CARTESIAN_POINT('Ctrl Pts',(-3.40733479453568,2.54786410535795,4.87770011735268));
#16226=CARTESIAN_POINT('Ctrl Pts',(-3.37128015690807,2.3183243706747,4.86658632829587));
#16227=CARTESIAN_POINT('Ctrl Pts',(-3.54457538552076,2.16354326577609,4.85547253923908));
#16228=CARTESIAN_POINT('Ctrl Pts',(-3.75407113442107,2.22119506367479,4.84507958712252));
#16229=CARTESIAN_POINT('Ctrl Pts',(-3.80505455493103,2.34521910535256,4.83839123135824));
#16230=CARTESIAN_POINT('Ctrl Pts',(-3.80555825533459,2.40017991403412,4.83540747194623));
#16231=CARTESIAN_POINT('Origin',(-3.6,2.4,5.35459252805377));
#16232=CARTESIAN_POINT('',(-3.80552958623817,2.39981603086253,4.97540747194623));
#16233=CARTESIAN_POINT('',(-3.8054461347863,2.4001877030526,4.96959252805377));
#16234=CARTESIAN_POINT('',(-3.805475,2.40000000000001,5.35459252805377));
#16235=CARTESIAN_POINT('Ctrl Pts',(-3.80544613478631,2.4001877030526,4.96959252805377));
#16236=CARTESIAN_POINT('Ctrl Pts',(-3.8056000456266,2.41718968004276,4.9686707998386));
#16237=CARTESIAN_POINT('Ctrl Pts',(-3.79589308272504,2.50235240455911,4.96404447527116));
#16238=CARTESIAN_POINT('Ctrl Pts',(-3.67755429503925,2.63014996180817,4.95571355435145));
#16239=CARTESIAN_POINT('Ctrl Pts',(-3.44869918906956,2.58997825726379,4.94459976529464));
#16240=CARTESIAN_POINT('Ctrl Pts',(-3.35833143120733,2.37591729928569,4.93348597623784));
#16241=CARTESIAN_POINT('Ctrl Pts',(-3.48916565507154,2.18389951041786,4.92237218718103));
#16242=CARTESIAN_POINT('Ctrl Pts',(-3.72144781179447,2.18968095039579,4.91125839812423));
#16243=CARTESIAN_POINT('Ctrl Pts',(-3.80419976151153,2.32515687187029,4.90366517841514));
#16244=CARTESIAN_POINT('Ctrl Pts',(-3.80580670007452,2.39655859898363,4.89977655505832));
#16245=CARTESIAN_POINT('Ctrl Pts',(-3.8057933217542,2.39993826202139,4.89959252805377));
#16246=CARTESIAN_POINT('Ctrl Pts',(-3.80552958623817,2.39981603086253,4.97540747194623));
#16247=CARTESIAN_POINT('Ctrl Pts',(-3.80503092645118,2.45384921596595,4.97247512456653));
#16248=CARTESIAN_POINT('Ctrl Pts',(-3.75549941221135,2.57695439031686,4.96583818083456));
#16249=CARTESIAN_POINT('Ctrl Pts',(-3.54785414659174,2.63720135974049,4.9554966407503));
#16250=CARTESIAN_POINT('Ctrl Pts',(-3.37243277255298,2.48483414437987,4.94438285169351));
#16251=CARTESIAN_POINT('Ctrl Pts',(-3.40530626273826,2.25481727477052,4.9332690626367));
#16252=CARTESIAN_POINT('Ctrl Pts',(-3.61638513853951,2.15768779995451,4.9221552735799));
#16253=CARTESIAN_POINT('Ctrl Pts',(-3.78023981554385,2.2618608319249,4.91286807668307));
#16254=CARTESIAN_POINT('Ctrl Pts',(-3.80513037719409,2.36523705642733,4.90728547613852));
#16255=CARTESIAN_POINT('Ctrl Pts',(-3.80514216591096,2.40000781019071,4.90540747194623));
#16256=CARTESIAN_POINT('Origin',(-3.6,2.4,5.35459252805377));
#16257=CARTESIAN_POINT('',(-3.8057470998819,2.40010656251728,5.04540747194623));
#16258=CARTESIAN_POINT('',(-3.80515433183015,2.39994744458997,5.03959252805377));
#16259=CARTESIAN_POINT('',(-3.805475,2.40000000000001,5.35459252805377));
#16260=CARTESIAN_POINT('Ctrl Pts',(-3.80515433183015,2.39994744458997,5.03959252805377));
#16261=CARTESIAN_POINT('Ctrl Pts',(-3.80506840880667,2.4374802122161,5.03756504461887));
#16262=CARTESIAN_POINT('Ctrl Pts',(-3.77723759754696,2.54371107308321,5.03183296483171));
#16263=CARTESIAN_POINT('Ctrl Pts',(-3.60662102779949,2.64277527582587,5.02239628869227));
#16264=CARTESIAN_POINT('Ctrl Pts',(-3.39962169493761,2.53723049491962,5.01128249963547));
#16265=CARTESIAN_POINT('Ctrl Pts',(-3.3760308968172,2.30607708183528,5.00016871057867));
#16266=CARTESIAN_POINT('Ctrl Pts',(-3.55744155898554,2.16089238284251,4.98905492152186));
#16267=CARTESIAN_POINT('Ctrl Pts',(-3.75953036163254,2.22845546798632,4.97886286068023));
#16268=CARTESIAN_POINT('Ctrl Pts',(-3.80498144946327,2.34885558664921,4.97237539619086));
#16269=CARTESIAN_POINT('Ctrl Pts',(-3.80544613478631,2.4001877030526,4.96959252805377));
#16270=CARTESIAN_POINT('Ctrl Pts',(-3.8057470998819,2.40010656251728,5.04540747194623));
#16271=CARTESIAN_POINT('Ctrl Pts',(-3.80578578291066,2.40623506936011,5.04507396569907));
#16272=CARTESIAN_POINT('Ctrl Pts',(-3.80275767503742,2.48040043607423,5.04103586309964));
#16273=CARTESIAN_POINT('Ctrl Pts',(-3.71288602216703,2.61503584063672,5.03329316414794));
#16274=CARTESIAN_POINT('Ctrl Pts',(-3.48055937550073,2.61146539619723,5.02217937509113));
#16275=CARTESIAN_POINT('Ctrl Pts',(-3.35755806712823,2.4143382523336,5.01106558603433));
#16276=CARTESIAN_POINT('Ctrl Pts',(-3.45646661930996,2.20408715554039,4.99995179697752));
#16277=CARTESIAN_POINT('Ctrl Pts',(-3.68675289766315,2.17315730107164,4.98883800792072));
#16278=CARTESIAN_POINT('Ctrl Pts',(-3.79782383296962,2.3032367743191,4.98065656624362));
#16279=CARTESIAN_POINT('Ctrl Pts',(-3.80566091089323,2.38558610982074,4.97617972091879));
#16280=CARTESIAN_POINT('Ctrl Pts',(-3.80552958623817,2.39981603086253,4.97540747194623));
#16281=CARTESIAN_POINT('Origin',(-3.6,2.4,5.35459252805377));
#16282=CARTESIAN_POINT('',(-3.80520911606596,2.40011619915578,5.11540747194623));
#16283=CARTESIAN_POINT('',(-3.80563879690963,2.399839625535,5.10959252805377));
#16284=CARTESIAN_POINT('',(-3.805475,2.40000000000001,5.35459252805377));
#16285=CARTESIAN_POINT('Ctrl Pts',(-3.80563879690963,2.399839625535,5.10959252805377));
#16286=CARTESIAN_POINT('Ctrl Pts',(-3.805144032728,2.45749534173516,5.10645928939914));
#16287=CARTESIAN_POINT('Ctrl Pts',(-3.74979515516761,2.58415303951777,5.09962145439226));
#16288=CARTESIAN_POINT('Ctrl Pts',(-3.53510505788101,2.63403473315196,5.0890790230331));
#16289=CARTESIAN_POINT('Ctrl Pts',(-3.36817873292179,2.47240567046266,5.07796523397629));
#16290=CARTESIAN_POINT('Ctrl Pts',(-3.41344102170209,2.24450262655374,5.06685144491949));
#16291=CARTESIAN_POINT('Ctrl Pts',(-3.6294628695539,2.15892821683407,5.05573765586269));
#16292=CARTESIAN_POINT('Ctrl Pts',(-3.78402795283848,2.2693666686934,5.04665135024078));
#16293=CARTESIAN_POINT('Ctrl Pts',(-3.80522540644911,2.36890073499569,5.04126964097114));
#16294=CARTESIAN_POINT('Ctrl Pts',(-3.80515433183015,2.39994744458997,5.03959252805377));
#16295=CARTESIAN_POINT('Ctrl Pts',(-3.80520911606596,2.40011619915578,5.11540747194623));
#16296=CARTESIAN_POINT('Ctrl Pts',(-3.80534689450199,2.42674223668704,5.11396821047934));
#16297=CARTESIAN_POINT('Ctrl Pts',(-3.7881600578547,2.52173200460476,5.10882435266019));
#16298=CARTESIAN_POINT('Ctrl Pts',(-3.64483147349944,2.63869087951471,5.09997589848877));
#16299=CARTESIAN_POINT('Ctrl Pts',(-3.42377646220466,2.56711959422357,5.08886210943196));
#16300=CARTESIAN_POINT('Ctrl Pts',(-3.36401957377094,2.34258029572384,5.07774832037515));
#16301=CARTESIAN_POINT('Ctrl Pts',(-3.52025888482579,2.17059867951396,5.06663453131835));
#16302=CARTESIAN_POINT('Ctrl Pts',(-3.7426071061349,2.20745024082863,5.05585424850871));
#16303=CARTESIAN_POINT('Ctrl Pts',(-3.80535609078813,2.33815945072363,5.04877856205134));
#16304=CARTESIAN_POINT('Ctrl Pts',(-3.8057470998819,2.40010656251728,5.04540747194623));
#16305=CARTESIAN_POINT('Origin',(-3.6,2.4,5.35459252805377));
#16306=CARTESIAN_POINT('',(-3.80526708520764,2.39977040928181,5.18540747194623));
#16307=CARTESIAN_POINT('',(-3.80565732826014,2.40014993187889,5.17959252805377));
#16308=CARTESIAN_POINT('',(-3.805475,2.40000000000001,5.35459252805377));
#16309=CARTESIAN_POINT('',(-3.65301702171886,2.20148256743283,5.2));
#16310=CARTESIAN_POINT('Ctrl Pts',(-3.65301702171886,2.20148256743283,5.2));
#16311=CARTESIAN_POINT('Ctrl Pts',(-3.71902879097456,2.21911198848201,5.19629540364773));
#16312=CARTESIAN_POINT('Ctrl Pts',(-3.79249439061758,2.28872811842027,5.19143122762981));
#16313=CARTESIAN_POINT('Ctrl Pts',(-3.80542873353734,2.378346888084,5.18656705161189));
#16314=CARTESIAN_POINT('Ctrl Pts',(-3.80526708520764,2.39977040928181,5.18540747194623));
#16315=CARTESIAN_POINT('',(-3.54686846753247,2.20112677390461,5.2));
#16316=CARTESIAN_POINT('Origin',(-3.6,2.4,5.2));
#16317=CARTESIAN_POINT('Ctrl Pts',(-3.54686839490754,2.2011265482535,5.2));
#16318=CARTESIAN_POINT('Ctrl Pts',(-3.61132828593009,2.18399467910883,5.19636770818144));
#16319=CARTESIAN_POINT('Ctrl Pts',(-3.74930829171963,2.21593295369214,5.1895652175327));
#16320=CARTESIAN_POINT('Ctrl Pts',(-3.80517196370246,2.34184094054235,5.18276272688396));
#16321=CARTESIAN_POINT('Ctrl Pts',(-3.80565732826014,2.40014993187889,5.17959252805377));
#16322=CARTESIAN_POINT('Origin',(-3.,1.8,5.2));
#16323=CARTESIAN_POINT('',(-3.,2.,0.8));
#16324=CARTESIAN_POINT('',(-3.2,1.8,0.8));
#16325=CARTESIAN_POINT('Origin',(-3.,1.8,0.8));
#16326=CARTESIAN_POINT('',(-3.,2.,5.2));
#16327=CARTESIAN_POINT('',(-3.,2.,5.2));
#16328=CARTESIAN_POINT('',(-3.2,1.8,5.2));
#16329=CARTESIAN_POINT('Origin',(-3.,1.8,5.2));
#16330=CARTESIAN_POINT('',(-3.2,1.8,5.2));
#16331=CARTESIAN_POINT('Origin',(-3.2,2.,5.2));
#16332=CARTESIAN_POINT('',(3.,2.,0.8));
#16333=CARTESIAN_POINT('',(3.2,2.,0.8));
#16334=CARTESIAN_POINT('',(3.,2.,5.2));
#16335=CARTESIAN_POINT('',(3.,2.,5.2));
#16336=CARTESIAN_POINT('',(-1.6,2.,5.2));
#16337=CARTESIAN_POINT('Origin',(3.,1.8,5.2));
#16338=CARTESIAN_POINT('',(3.2,1.8,0.8));
#16339=CARTESIAN_POINT('Origin',(3.,1.8,0.8));
#16340=CARTESIAN_POINT('',(3.2,1.8,5.2));
#16341=CARTESIAN_POINT('',(3.2,1.8,5.2));
#16342=CARTESIAN_POINT('Origin',(3.,1.8,5.2));
#16343=CARTESIAN_POINT('Origin',(3.2,2.,5.2));
#16344=CARTESIAN_POINT('',(3.2,-1.8,0.8));
#16345=CARTESIAN_POINT('',(3.2,-2.,0.8));
#16346=CARTESIAN_POINT('',(3.2,-1.8,5.2));
#16347=CARTESIAN_POINT('',(3.2,-1.8,5.2));
#16348=CARTESIAN_POINT('',(3.2,1.,5.2));
#16349=CARTESIAN_POINT('Origin',(-3.,-1.8,5.2));
#16350=CARTESIAN_POINT('',(-3.2,-1.8,0.8));
#16351=CARTESIAN_POINT('',(-3.,-2.,0.8));
#16352=CARTESIAN_POINT('Origin',(-3.,-1.8,0.8));
#16353=CARTESIAN_POINT('',(-3.2,-1.8,5.2));
#16354=CARTESIAN_POINT('',(-3.2,-1.8,5.2));
#16355=CARTESIAN_POINT('',(-3.,-2.,5.2));
#16356=CARTESIAN_POINT('Origin',(-3.,-1.8,5.2));
#16357=CARTESIAN_POINT('',(-3.,-2.,5.2));
#16358=CARTESIAN_POINT('Origin',(0.,0.,0.8));
#16359=CARTESIAN_POINT('',(-3.2,2.,0.8));
#16360=CARTESIAN_POINT('',(3.,-2.,0.8));
#16361=CARTESIAN_POINT('',(-3.2,-2.,0.8));
#16362=CARTESIAN_POINT('Origin',(3.,-1.8,0.8));
#16363=CARTESIAN_POINT('',(-0.8,-9.79717439317883E-17,0.8));
#16364=CARTESIAN_POINT('Origin',(0.,0.,0.8));
#16365=CARTESIAN_POINT('',(2.65,1.,0.8));
#16366=CARTESIAN_POINT('Origin',(2.4,1.,0.8));
#16367=CARTESIAN_POINT('',(-2.15,1.,0.8));
#16368=CARTESIAN_POINT('Origin',(-2.4,1.,0.8));
#16369=CARTESIAN_POINT('Origin',(3.2,-2.,5.2));
#16370=CARTESIAN_POINT('',(3.,-2.,5.2));
#16371=CARTESIAN_POINT('',(1.6,-2.,5.2));
#16372=CARTESIAN_POINT('',(3.,-2.,5.2));
#16373=CARTESIAN_POINT('',(7.34788079488412E-17,-2.,2.8));
#16374=CARTESIAN_POINT('Origin',(0.,-2.,2.2));
#16375=CARTESIAN_POINT('Origin',(3.,-1.8,5.2));
#16376=CARTESIAN_POINT('Origin',(3.,-1.8,5.2));
#16377=CARTESIAN_POINT('Origin',(0.,-2.4,2.2));
#16378=CARTESIAN_POINT('',(7.34788079488412E-17,-2.8,2.8));
#16379=CARTESIAN_POINT('Origin',(0.,-2.8,2.2));
#16380=CARTESIAN_POINT('',(7.34788079488412E-17,-2.4,2.8));
#16381=CARTESIAN_POINT('Origin',(-2.4,1.,0.4));
#16382=CARTESIAN_POINT('',(-2.,1.,0.4));
#16383=CARTESIAN_POINT('Origin',(-2.4,1.,0.4));
#16384=CARTESIAN_POINT('',(-2.15,1.,0.4));
#16385=CARTESIAN_POINT('Origin',(-2.4,1.,0.4));
#16386=CARTESIAN_POINT('Origin',(-2.4,1.,0.2));
#16387=CARTESIAN_POINT('',(-2.,1.,0.));
#16388=CARTESIAN_POINT('Origin',(-2.4,1.,0.));
#16389=CARTESIAN_POINT('',(-2.,1.,0.2));
#16390=CARTESIAN_POINT('Origin',(-2.4,1.,0.4));
#16391=CARTESIAN_POINT('',(-2.15,1.,0.4));
#16392=CARTESIAN_POINT('Origin',(2.4,1.,0.4));
#16393=CARTESIAN_POINT('',(2.8,1.,0.4));
#16394=CARTESIAN_POINT('Origin',(2.4,1.,0.4));
#16395=CARTESIAN_POINT('',(2.65,1.,0.4));
#16396=CARTESIAN_POINT('Origin',(2.4,1.,0.4));
#16397=CARTESIAN_POINT('Origin',(2.4,1.,0.2));
#16398=CARTESIAN_POINT('',(2.8,1.,0.));
#16399=CARTESIAN_POINT('Origin',(2.4,1.,0.));
#16400=CARTESIAN_POINT('',(2.8,1.,0.2));
#16401=CARTESIAN_POINT('Origin',(2.4,1.,0.4));
#16402=CARTESIAN_POINT('',(2.65,1.,0.4));
#16403=CARTESIAN_POINT('Origin',(-3.6,2.4,4.3));
#16404=CARTESIAN_POINT('Ctrl Pts',(-3.76351293272515,2.3680769545372,4.3));
#16405=CARTESIAN_POINT('Ctrl Pts',(-3.76286871316717,2.35978063266222,4.3));
#16406=CARTESIAN_POINT('Ctrl Pts',(-3.76155560899202,2.35157023575845,4.3));
#16407=CARTESIAN_POINT('Ctrl Pts',(-3.75963220387653,2.34349709858594,4.3));
#16408=CARTESIAN_POINT('Ctrl Pts',(-3.75857027766629,2.33903985975814,4.3));
#16409=CARTESIAN_POINT('Ctrl Pts',(-3.75732203034493,2.33462439532847,4.3));
#16410=CARTESIAN_POINT('Ctrl Pts',(-3.75589532649161,2.33025917511629,4.3));
#16411=CARTESIAN_POINT('Ctrl Pts',(-3.75435560971578,2.32554817445892,4.3));
#16412=CARTESIAN_POINT('Ctrl Pts',(-3.75261043848503,2.32090359735875,4.3));
#16413=CARTESIAN_POINT('Ctrl Pts',(-3.75067344213558,2.31634215529567,4.3));
#16414=CARTESIAN_POINT('Ctrl Pts',(-3.74745267041618,2.30875754441053,4.3));
#16415=CARTESIAN_POINT('Ctrl Pts',(-3.74370039609997,2.30139711771457,4.3));
#16416=CARTESIAN_POINT('Ctrl Pts',(-3.73945961576596,2.29430909563144,4.3));
#16417=CARTESIAN_POINT('Ctrl Pts',(-3.73760645031824,2.29121172284092,4.3));
#16418=CARTESIAN_POINT('Ctrl Pts',(-3.73566013813008,2.28816728583911,4.3));
#16419=CARTESIAN_POINT('Ctrl Pts',(-3.73363014813367,2.28518827452246,4.3));
#16420=CARTESIAN_POINT('Ctrl Pts',(-3.72675415090804,2.27509774521709,4.3));
#16421=CARTESIAN_POINT('Ctrl Pts',(-3.71890632139719,2.26572975853371,4.3));
#16422=CARTESIAN_POINT('Ctrl Pts',(-3.71022045861654,2.25723279915054,4.3));
#16423=CARTESIAN_POINT('Ctrl Pts',(-3.7059906475113,2.25309497956169,4.3));
#16424=CARTESIAN_POINT('Ctrl Pts',(-3.70156132140551,2.2491639079058,4.3));
#16425=CARTESIAN_POINT('Ctrl Pts',(-3.6969439956845,2.24545878490313,4.3));
#16426=CARTESIAN_POINT('Ctrl Pts',(-3.69303802929494,2.24232448448942,4.3));
#16427=CARTESIAN_POINT('Ctrl Pts',(-3.68899297342194,2.23934940616711,4.3));
#16428=CARTESIAN_POINT('Ctrl Pts',(-3.68484121061819,2.23656266363051,4.3));
#16429=CARTESIAN_POINT('Ctrl Pts',(-3.67976592507208,2.23315603498015,4.3));
#16430=CARTESIAN_POINT('Ctrl Pts',(-3.6745257104219,2.23002554470273,4.3));
#16431=CARTESIAN_POINT('Ctrl Pts',(-3.66913582629221,2.22718930926681,4.3));
#16432=CARTESIAN_POINT('Ctrl Pts',(-3.6615627323528,2.22320423706977,4.3));
#16433=CARTESIAN_POINT('Ctrl Pts',(-3.65369447955584,2.21979946771843,4.3));
#16434=CARTESIAN_POINT('Ctrl Pts',(-3.64559786041243,2.21695927257373,4.3));
#16435=CARTESIAN_POINT('Ctrl Pts',(-3.6396877011334,2.21488606085518,4.3));
#16436=CARTESIAN_POINT('Ctrl Pts',(-3.63365563048822,2.21311388420288,4.3));
#16437=CARTESIAN_POINT('Ctrl Pts',(-3.62752539225901,2.21164027047228,4.3));
#16438=CARTESIAN_POINT('Ctrl Pts',(-3.62399744472375,2.21079220686783,4.3));
#16439=CARTESIAN_POINT('Ctrl Pts',(-3.62044147481098,2.2100443281221,4.3));
#16440=CARTESIAN_POINT('Ctrl Pts',(-3.61687028704666,2.20939689951074,4.3));
#16441=CARTESIAN_POINT('Ctrl Pts',(-3.605353381675,2.20730897399576,4.3));
#16442=CARTESIAN_POINT('Ctrl Pts',(-3.59365536798806,2.20625732317521,4.3));
#16443=CARTESIAN_POINT('Ctrl Pts',(-3.58193303067035,2.20620865478203,4.3));
#16444=CARTESIAN_POINT('Ctrl Pts',(-3.57526869322992,2.20618098601718,4.3));
#16445=CARTESIAN_POINT('Ctrl Pts',(-3.56859610554753,2.20647808326505,4.3));
#16446=CARTESIAN_POINT('Ctrl Pts',(-3.5619424077193,2.20709864598645,4.3));
#16447=CARTESIAN_POINT('Ctrl Pts',(-3.55784552037318,2.20748074562885,4.3));
#16448=CARTESIAN_POINT('Ctrl Pts',(-3.55375372321261,2.20798587206127,4.3));
#16449=CARTESIAN_POINT('Ctrl Pts',(-3.54967985340644,2.20861337807665,4.3));
#16450=CARTESIAN_POINT('Ctrl Pts',(-3.53642392777045,2.21065521384261,4.3));
#16451=CARTESIAN_POINT('Ctrl Pts',(-3.52344437883893,2.21397442298982,4.3));
#16452=CARTESIAN_POINT('Ctrl Pts',(-3.51095539964347,2.2185383760968,4.3));
#16453=CARTESIAN_POINT('Ctrl Pts',(-3.50062245090115,2.22231443279277,4.3));
#16454=CARTESIAN_POINT('Ctrl Pts',(-3.49062431451358,2.22694342333832,4.3));
#16455=CARTESIAN_POINT('Ctrl Pts',(-3.48108410337466,2.23243384161104,4.3));
#16456=CARTESIAN_POINT('Ctrl Pts',(-3.47992982403391,2.23309813260964,4.3));
#16457=CARTESIAN_POINT('Ctrl Pts',(-3.47878225959784,2.23377506397182,4.3));
#16458=CARTESIAN_POINT('Ctrl Pts',(-3.47764149019701,2.2344644673347,4.3));
#16459=CARTESIAN_POINT('Ctrl Pts',(-3.41173724903364,2.31767678198965,4.3));
#16460=CARTESIAN_POINT('Ctrl Pts',(-3.40908132667977,2.32572936887695,4.3));
#16461=CARTESIAN_POINT('Ctrl Pts',(-3.40697195743913,2.3339396046188,4.3));
#16462=CARTESIAN_POINT('Ctrl Pts',(-3.40539675516275,2.34225613248928,4.3));
#16463=CARTESIAN_POINT('Ctrl Pts',(-3.40421042715,2.34851953759571,4.3));
#16464=CARTESIAN_POINT('Ctrl Pts',(-3.40332726918042,2.35484328996956,4.3));
#16465=CARTESIAN_POINT('Ctrl Pts',(-3.40274510142185,2.36120518228067,4.3));
#16466=CARTESIAN_POINT('Ctrl Pts',(-3.40230911384944,2.36596962679656,4.3));
#16467=CARTESIAN_POINT('Ctrl Pts',(-3.40204239822336,2.37075409356134,4.3));
#16468=CARTESIAN_POINT('Ctrl Pts',(-3.40194406709946,2.37553699140669,4.3));
#16469=CARTESIAN_POINT('Ctrl Pts',(-3.40173837831389,2.38554184450123,4.3));
#16470=CARTESIAN_POINT('Ctrl Pts',(-3.40226689742789,2.39555478383888,4.3));
#16471=CARTESIAN_POINT('Ctrl Pts',(-3.40352192589958,2.40548747856692,4.3));
#16472=CARTESIAN_POINT('Ctrl Pts',(-3.40417748512669,2.41067578291694,4.3));
#16473=CARTESIAN_POINT('Ctrl Pts',(-3.40503255607762,2.41584510393915,4.3));
#16474=CARTESIAN_POINT('Ctrl Pts',(-3.40608151604784,2.42095776789691,4.3));
#16475=CARTESIAN_POINT('Ctrl Pts',(-3.40864845689543,2.4334691184973,4.3));
#16476=CARTESIAN_POINT('Ctrl Pts',(-3.41237570095201,2.44567367466126,4.3));
#16477=CARTESIAN_POINT('Ctrl Pts',(-3.41724958122609,2.45738288213971,4.3));
#16478=CARTESIAN_POINT('Ctrl Pts',(-3.41948715125122,2.46275851104282,4.3));
#16479=CARTESIAN_POINT('Ctrl Pts',(-3.42196701213329,2.46802938689262,4.3));
#16480=CARTESIAN_POINT('Ctrl Pts',(-3.4246907645117,2.47317480637784,4.3));
#16481=CARTESIAN_POINT('Ctrl Pts',(-3.42647139059006,2.47653857328711,4.3));
#16482=CARTESIAN_POINT('Ctrl Pts',(-3.42835735887431,2.47985042338477,4.3));
#16483=CARTESIAN_POINT('Ctrl Pts',(-3.43034607421528,2.48309853180527,4.3));
#16484=CARTESIAN_POINT('Ctrl Pts',(-3.4346184872232,2.49007653432835,4.3));
#16485=CARTESIAN_POINT('Ctrl Pts',(-3.43934735204432,2.49673388406761,4.3));
#16486=CARTESIAN_POINT('Ctrl Pts',(-3.44453054699271,2.50301823813816,4.3));
#16487=CARTESIAN_POINT('Ctrl Pts',(-3.45023589251222,2.50993567259632,4.3));
#16488=CARTESIAN_POINT('Ctrl Pts',(-3.45649190823175,2.51640147868906,4.3));
#16489=CARTESIAN_POINT('Ctrl Pts',(-3.46322632730094,2.52238265672963,4.3));
#16490=CARTESIAN_POINT('Ctrl Pts',(-3.46747028515846,2.52615193026038,4.3));
#16491=CARTESIAN_POINT('Ctrl Pts',(-3.47190440586361,2.52972849539073,4.3));
#16492=CARTESIAN_POINT('Ctrl Pts',(-3.4765114687556,2.53310132051434,4.3));
#16493=CARTESIAN_POINT('Ctrl Pts',(-3.47932494356125,2.53516106198772,4.3));
#16494=CARTESIAN_POINT('Ctrl Pts',(-3.48219950761294,2.53714209816472,4.3));
#16495=CARTESIAN_POINT('Ctrl Pts',(-3.48512412807744,2.53903826687632,4.3));
#16496=CARTESIAN_POINT('Ctrl Pts',(-3.49373597317477,2.5446217302422,4.3));
#16497=CARTESIAN_POINT('Ctrl Pts',(-3.50279826970664,2.54948377957132,4.3));
#16498=CARTESIAN_POINT('Ctrl Pts',(-3.51220207894208,2.55357333967367,4.3));
#16499=CARTESIAN_POINT('Ctrl Pts',(-3.5210279439966,2.5574115614721,4.3));
#16500=CARTESIAN_POINT('Ctrl Pts',(-3.53015530415702,2.56056927246177,4.3));
#16501=CARTESIAN_POINT('Ctrl Pts',(-3.53949459164804,2.56298239916129,4.3));
#16502=CARTESIAN_POINT('Ctrl Pts',(-3.54298202528158,2.5638834977967,4.3));
#16503=CARTESIAN_POINT('Ctrl Pts',(-3.54649047145145,2.5646782882288,4.3));
#16504=CARTESIAN_POINT('Ctrl Pts',(-3.55001192980026,2.5653638227639,4.3));
#16505=CARTESIAN_POINT('Ctrl Pts',(-3.56109314401874,2.567521041247,4.3));
#16506=CARTESIAN_POINT('Ctrl Pts',(-3.57231422450356,2.56860269457927,4.3));
#16507=CARTESIAN_POINT('Ctrl Pts',(-3.58352456323646,2.56851224856759,4.3));
#16508=CARTESIAN_POINT('Ctrl Pts',(-3.58970650036672,2.56846237214805,4.3));
#16509=CARTESIAN_POINT('Ctrl Pts',(-3.59588506606642,2.56805522595141,4.3));
#16510=CARTESIAN_POINT('Ctrl Pts',(-3.60203269728429,2.56726809931874,4.3));
#16511=CARTESIAN_POINT('Ctrl Pts',(-3.60310836212971,2.56713037400346,4.3));
#16512=CARTESIAN_POINT('Ctrl Pts',(-3.60418307356748,2.56698100334876,4.3));
#16513=CARTESIAN_POINT('Ctrl Pts',(-3.60525667864057,2.56682005840211,4.3));
#16514=CARTESIAN_POINT('Origin',(-3.6,2.4,5.35459252805377));
#16515=CARTESIAN_POINT('Ctrl Pts',(-3.80565732826014,2.40014993187889,5.17959252805377));
#16516=CARTESIAN_POINT('Ctrl Pts',(-3.80573914572043,2.40997902530624,5.17905813053169));
#16517=CARTESIAN_POINT('Ctrl Pts',(-3.80062938236564,2.48786313470717,5.17481913665734));
#16518=CARTESIAN_POINT('Ctrl Pts',(-3.70109553522054,2.62084298334156,5.16687554643073));
#16519=CARTESIAN_POINT('Ctrl Pts',(-3.46929950811782,2.60468896536386,5.15576175737392));
#16520=CARTESIAN_POINT('Ctrl Pts',(-3.35713783891219,2.401213058351,5.14464796831712));
#16521=CARTESIAN_POINT('Ctrl Pts',(-3.46726930372222,2.19661072251331,5.13353417926031));
#16522=CARTESIAN_POINT('Ctrl Pts',(-3.69889135748228,2.17818094124235,5.12242039020352));
#16523=CARTESIAN_POINT('Ctrl Pts',(-3.80021577778504,2.31073764355723,5.11443983980133));
#16524=CARTESIAN_POINT('Ctrl Pts',(-3.80572901899447,2.38932589169745,5.11016388575141));
#16525=CARTESIAN_POINT('Ctrl Pts',(-3.80563879690963,2.399839625535,5.10959252805377));
#16526=CARTESIAN_POINT('Ctrl Pts',(-3.80526708520764,2.39977040928181,5.18540747194623));
#16527=CARTESIAN_POINT('Ctrl Pts',(-3.80491230346332,2.4467902221928,5.18286245525962));
#16528=CARTESIAN_POINT('Ctrl Pts',(-3.76565540874154,2.56295294620881,5.17661284222074));
#16529=CARTESIAN_POINT('Ctrl Pts',(-3.57278676575927,2.64128531597693,5.16665863282959));
#16530=CARTESIAN_POINT('Ctrl Pts',(-3.38252462806861,2.5080933346037,5.15554484377278));
#16531=CARTESIAN_POINT('Ctrl Pts',(-3.39123766596766,2.27586209704876,5.14443105471597));
#16532=CARTESIAN_POINT('Ctrl Pts',(-3.59107442724388,2.15730569128375,5.13331726565918));
#16533=CARTESIAN_POINT('Ctrl Pts',(-3.77212564275939,2.247453977085,5.12364273806926));
#16534=CARTESIAN_POINT('Ctrl Pts',(-3.80499225880634,2.35820797534334,5.11767280683161));
#16535=CARTESIAN_POINT('Ctrl Pts',(-3.80520911606596,2.40011619915578,5.11540747194623));
#16536=CARTESIAN_POINT('Ctrl Pts',(-3.47309291201476,2.50793586530485,5.2));
#16537=CARTESIAN_POINT('Ctrl Pts',(-3.43720166889934,2.46573623930395,5.19629540364773));
#16538=CARTESIAN_POINT('Ctrl Pts',(-3.41147910372774,2.34341327692754,5.1888862109432));
#16539=CARTESIAN_POINT('Ctrl Pts',(-3.54548749138621,2.21065847912018,5.17777242188639));
#16540=CARTESIAN_POINT('Ctrl Pts',(-3.72942273074541,2.25164328799446,5.16665863282959));
#16541=CARTESIAN_POINT('Ctrl Pts',(-3.79487861203899,2.42820978532064,5.15554484377278));
#16542=CARTESIAN_POINT('Ctrl Pts',(-3.68196868800459,2.57906042596279,5.14443105471598));
#16543=CARTESIAN_POINT('Ctrl Pts',(-3.49402748778406,2.56596267978888,5.13331726565918));
#16544=CARTESIAN_POINT('Ctrl Pts',(-3.40308633148933,2.40098355284719,5.12220347660236));
#16545=CARTESIAN_POINT('Ctrl Pts',(-3.49238138946403,2.23509111264493,5.11108968754557));
#16546=CARTESIAN_POINT('Ctrl Pts',(-3.68018153136171,2.22014816795705,5.09997589848877));
#16547=CARTESIAN_POINT('Ctrl Pts',(-3.79459033398193,2.36982238810866,5.08886210943195));
#16548=CARTESIAN_POINT('Ctrl Pts',(-3.73088853410035,2.54712014517116,5.07774832037516));
#16549=CARTESIAN_POINT('Ctrl Pts',(-3.54738290615879,2.58975635256414,5.06663453131835));
#16550=CARTESIAN_POINT('Ctrl Pts',(-3.41203833510047,2.45870682418337,5.05552074226154));
#16551=CARTESIAN_POINT('Ctrl Pts',(-3.44873719048823,2.27392207121964,5.04440695320474));
#16552=CARTESIAN_POINT('Ctrl Pts',(-3.62388861938279,2.20453797748901,5.03329316414794));
#16553=CARTESIAN_POINT('Ctrl Pts',(-3.77717451978384,2.31406243911007,5.02217937509113));
#16554=CARTESIAN_POINT('Ctrl Pts',(-3.76829057505717,2.5022465500548,5.01106558603433));
#16555=CARTESIAN_POINT('Ctrl Pts',(-3.60536835737386,2.5968432215724,4.99995179697752));
#16556=CARTESIAN_POINT('Ctrl Pts',(-3.43753242183529,2.51126706632734,4.98883800792072));
#16557=CARTESIAN_POINT('Ctrl Pts',(-3.41840490283366,2.32384690027379,4.97772421886392));
#16558=CARTESIAN_POINT('Ctrl Pts',(-3.56549343582914,2.20613053160512,4.96661042980711));
#16559=CARTESIAN_POINT('Ctrl Pts',(-3.74416621827519,2.26586508520319,4.95549664075031));
#16560=CARTESIAN_POINT('Ctrl Pts',(-3.79088202621085,2.44837484789993,4.9443828516935));
#16561=CARTESIAN_POINT('Ctrl Pts',(-3.66288135078982,2.58660656351012,4.9332690626367));
#16562=CARTESIAN_POINT('Ctrl Pts',(-3.47732466187608,2.55403517537485,4.9221552735799));
#16563=CARTESIAN_POINT('Ctrl Pts',(-3.40405410117601,2.38047364429248,4.91104148452309));
#16564=CARTESIAN_POINT('Ctrl Pts',(-3.51013504384922,2.2247848080575,4.89992769546628));
#16565=CARTESIAN_POINT('Ctrl Pts',(-3.69847040002413,2.22947242407076,4.88881390640949));
#16566=CARTESIAN_POINT('Ctrl Pts',(-3.79667468232717,2.39024586425236,4.87770011735267));
#16567=CARTESIAN_POINT('Ctrl Pts',(-3.7148603974533,2.55994737550017,4.86658632829588));
#16568=CARTESIAN_POINT('Ctrl Pts',(-3.52791308818505,2.58324724002758,4.85547253923907));
#16569=CARTESIAN_POINT('Ctrl Pts',(-3.40694774682213,2.43881882759193,4.84435875018226));
#16570=CARTESIAN_POINT('Ctrl Pts',(-3.46268532215442,2.25885910202633,4.83324496112546));
#16571=CARTESIAN_POINT('Ctrl Pts',(-3.64410857937311,2.20808724102248,4.82213117206866));
#16572=CARTESIAN_POINT('Ctrl Pts',(-3.78515875366629,2.33297530474957,4.81101738301185));
#16573=CARTESIAN_POINT('Ctrl Pts',(-3.75673102088563,2.51921183215107,4.79990359395505));
#16574=CARTESIAN_POINT('Ctrl Pts',(-3.58484560723768,2.59633241763059,4.78878980489824));
#16575=CARTESIAN_POINT('Ctrl Pts',(-3.42683118114759,2.49374771469177,4.77767601584145));
#16576=CARTESIAN_POINT('Ctrl Pts',(-3.42732013882109,2.30535466532418,4.76656222678463));
#16577=CARTESIAN_POINT('Ctrl Pts',(-3.58586493175446,2.20359156413646,4.75544843772784));
#16578=CARTESIAN_POINT('Ctrl Pts',(-3.75734771295555,2.28160333171781,4.74433464867102));
#16579=CARTESIAN_POINT('Ctrl Pts',(-3.784808348044,2.46798491248738,4.73322085961423));
#16580=CARTESIAN_POINT('Ctrl Pts',(-3.64311180629855,2.59213913185591,4.72210707055742));
#16581=CARTESIAN_POINT('Ctrl Pts',(-3.46195453932691,2.54042622483077,4.71099328150062));
#16582=CARTESIAN_POINT('Ctrl Pts',(-3.40715184805135,2.36017960167632,4.69987949244381));
#16583=CARTESIAN_POINT('Ctrl Pts',(-3.52886525730118,2.21638104070156,4.688765703387));
#16584=CARTESIAN_POINT('Ctrl Pts',(-3.7156891032661,2.24065099555331,4.67765191433021));
#16585=CARTESIAN_POINT('Ctrl Pts',(-3.79662140100789,2.41077490131571,4.6665381252734));
#16586=CARTESIAN_POINT('Ctrl Pts',(-3.69758390056881,2.57103641770819,4.65542433621659));
#16587=CARTESIAN_POINT('Ctrl Pts',(-3.50922674926239,2.57474636128738,4.64431054715979));
#16588=CARTESIAN_POINT('Ctrl Pts',(-3.40395538379481,2.41850897862188,4.63319675810298));
#16589=CARTESIAN_POINT('Ctrl Pts',(-3.47812587883694,2.24533011791732,4.62208296904618));
#16590=CARTESIAN_POINT('Ctrl Pts',(-3.6638491391263,2.21372235435953,4.61096917998938));
#16591=CARTESIAN_POINT('Ctrl Pts',(-3.79113055827457,2.35261663238717,4.59985539093257));
#16592=CARTESIAN_POINT('Ctrl Pts',(-3.74346800986679,2.53488144415775,4.58874160187577));
#16593=CARTESIAN_POINT('Ctrl Pts',(-3.56448756498879,2.59368774042515,4.57762781281897));
#16594=CARTESIAN_POINT('Ctrl Pts',(-3.41801205461748,2.475209451325,4.56651402376216));
#16595=CARTESIAN_POINT('Ctrl Pts',(-3.4381121745334,2.28789109846994,4.55540023470536));
#16596=CARTESIAN_POINT('Ctrl Pts',(-3.60639005704185,2.20318729463469,4.54428644564855));
#16597=CARTESIAN_POINT('Ctrl Pts',(-3.76881904785141,2.29862839193225,4.53317265659175));
#16598=CARTESIAN_POINT('Ctrl Pts',(-3.77672604966501,2.48685607191854,4.52205886753494));
#16599=CARTESIAN_POINT('Ctrl Pts',(-3.62287369392911,2.59558340387831,4.51094507847814));
#16600=CARTESIAN_POINT('Ctrl Pts',(-3.44808478689753,2.52529102897173,4.49983128942133));
#16601=CARTESIAN_POINT('Ctrl Pts',(-3.41234559692803,2.34031835280842,4.48871750036453));
#16602=CARTESIAN_POINT('Ctrl Pts',(-3.54836861088932,2.20997296824294,4.47760371130773));
#16603=CARTESIAN_POINT('Ctrl Pts',(-3.73165041953522,2.2535614747159,4.46648992225092));
#16604=CARTESIAN_POINT('Ctrl Pts',(-3.79443110878254,2.431186836485,4.45537613319412));
#16605=CARTESIAN_POINT('Ctrl Pts',(-3.67924679391792,2.58026650835313,4.44426234413731));
#16606=CARTESIAN_POINT('Ctrl Pts',(-3.49152700036135,2.56434625038721,4.43314855508051));
#16607=CARTESIAN_POINT('Ctrl Pts',(-3.40309375251607,2.39799790627107,4.4220347660237));
#16608=CARTESIAN_POINT('Ctrl Pts',(-3.49489106815987,2.23348230018954,4.4109209769669));
#16609=CARTESIAN_POINT('Ctrl Pts',(-3.68289569684173,2.22138183485646,4.3998071879101));
#16610=CARTESIAN_POINT('Ctrl Pts',(-3.79502512287648,2.37277339930001,4.38869339885329));
#16611=CARTESIAN_POINT('Ctrl Pts',(-3.72864550427982,2.54908418322982,4.37757960979649));
#16612=CARTESIAN_POINT('Ctrl Pts',(-3.54451587329345,2.58893972093235,4.36646582073968));
#16613=CARTESIAN_POINT('Ctrl Pts',(-3.41117013795305,2.4558501873037,4.35535203168288));
#16614=CARTESIAN_POINT('Ctrl Pts',(-3.45066522941702,2.27165316239582,4.34423824262608));
#16615=CARTESIAN_POINT('Ctrl Pts',(-3.62684269841689,2.20490778718547,4.33312445356927));
#16616=CARTESIAN_POINT('Ctrl Pts',(-3.77846161969435,2.31678392154068,4.32201066451247));
#16617=CARTESIAN_POINT('Ctrl Pts',(-3.76671077264337,2.50472571563538,4.31089687545566));
#16618=CARTESIAN_POINT('Ctrl Pts',(-3.6024119571336,2.59701778495161,4.29978308639886));
#16619=CARTESIAN_POINT('Ctrl Pts',(-3.43581014038123,2.50855356077874,4.28866929734205));
#16620=CARTESIAN_POINT('Ctrl Pts',(-3.42516046182893,2.38400982617005,4.28126010463752));
#16621=CARTESIAN_POINT('Ctrl Pts',(-3.44735576439472,2.33325198627315,4.27755550828525));
#16622=CARTESIAN_POINT('Ctrl Pts',(-3.46322193753412,2.51633123698097,5.20748149723825));
#16623=CARTESIAN_POINT('Ctrl Pts',(-3.42453903360215,2.47084927712496,5.20377690088598));
#16624=CARTESIAN_POINT('Ctrl Pts',(-3.39681573869656,2.33901189865735,5.19636770818145));
#16625=CARTESIAN_POINT('Ctrl Pts',(-3.54124744782407,2.19593128499412,5.18525391912464));
#16626=CARTESIAN_POINT('Ctrl Pts',(-3.73948937471845,2.24010393789599,5.17414013006784));
#16627=CARTESIAN_POINT('Ctrl Pts',(-3.81003648727512,2.43040397380471,5.16302634101103));
#16628=CARTESIAN_POINT('Ctrl Pts',(-3.68834430374324,2.59298794508905,5.15191255195423));
#16629=CARTESIAN_POINT('Ctrl Pts',(-3.48578482789531,2.57887144164721,5.14079876289743));
#16630=CARTESIAN_POINT('Ctrl Pts',(-3.38777016729695,2.40106005468179,5.12968497384062));
#16631=CARTESIAN_POINT('Ctrl Pts',(-3.48401069421676,2.22226431593439,5.11857118478382));
#16632=CARTESIAN_POINT('Ctrl Pts',(-3.68641814006856,2.20615909238548,5.10745739572702));
#16633=CARTESIAN_POINT('Ctrl Pts',(-3.80972578663008,2.36747513988482,5.0963436066702));
#16634=CARTESIAN_POINT('Ctrl Pts',(-3.74106918988897,2.55856331372564,5.0852298176134));
#16635=CARTESIAN_POINT('Ctrl Pts',(-3.5432902900662,2.60451581276008,5.0741160285566));
#16636=CARTESIAN_POINT('Ctrl Pts',(-3.39741846770758,2.46327310627647,5.06300223949979));
#16637=CARTESIAN_POINT('Ctrl Pts',(-3.43697180089285,2.26411558966434,5.05188845044299));
#16638=CARTESIAN_POINT('Ctrl Pts',(-3.62574670277316,2.18933472393736,5.04077466138618));
#16639=CARTESIAN_POINT('Ctrl Pts',(-3.79095535102953,2.30737812002324,5.02966087232938));
#16640=CARTESIAN_POINT('Ctrl Pts',(-3.78138040319912,2.51019940046172,5.01854708327258));
#16641=CARTESIAN_POINT('Ctrl Pts',(-3.60578591418241,2.61215390632356,5.00743329421578));
#16642=CARTESIAN_POINT('Ctrl Pts',(-3.42489551286939,2.51992154252476,4.99631950515897));
#16643=CARTESIAN_POINT('Ctrl Pts',(-3.40428023416151,2.31792362746096,4.98520571610217));
#16644=CARTESIAN_POINT('Ctrl Pts',(-3.56280947688127,2.19105114868425,4.97409192704536));
#16645=CARTESIAN_POINT('Ctrl Pts',(-3.75537962710962,2.25543192231258,4.96297813798856));
#16646=CARTESIAN_POINT('Ctrl Pts',(-3.80572904255528,2.45213749738394,4.95186434893175));
#16647=CARTESIAN_POINT('Ctrl Pts',(-3.6677723322063,2.60112102960948,4.94075055987495));
#16648=CARTESIAN_POINT('Ctrl Pts',(-3.46778283760724,2.56601620267116,4.92963677081815));
#16649=CARTESIAN_POINT('Ctrl Pts',(-3.38881321118645,2.37895486262355,4.91852298176134));
#16650=CARTESIAN_POINT('Ctrl Pts',(-3.50314524759,2.21115637551095,4.90740919270453));
#16651=CARTESIAN_POINT('Ctrl Pts',(-3.70612953728091,2.21620859951243,4.89629540364773));
#16652=CARTESIAN_POINT('Ctrl Pts',(-3.81197225790835,2.38948717672297,4.88518161459093));
#16653=CARTESIAN_POINT('Ctrl Pts',(-3.72379436694309,2.57238826029923,4.87406782553412));
#16654=CARTESIAN_POINT('Ctrl Pts',(-3.52230608799136,2.5975004142094,4.86295403647732));
#16655=CARTESIAN_POINT('Ctrl Pts',(-3.39193192780995,2.44183819918584,4.85184024742051));
#16656=CARTESIAN_POINT('Ctrl Pts',(-3.45200483375657,2.24788100597045,4.84072645836371));
#16657=CARTESIAN_POINT('Ctrl Pts',(-3.64753939374511,2.19316005313682,4.8296126693069));
#16658=CARTESIAN_POINT('Ctrl Pts',(-3.79956060750538,2.3277620493917,4.81849888025011));
#16659=CARTESIAN_POINT('Ctrl Pts',(-3.76892173404475,2.52848426107239,4.80738509119329));
#16660=CARTESIAN_POINT('Ctrl Pts',(-3.5836668817102,2.61160337148291,4.7962713021365));
#16661=CARTESIAN_POINT('Ctrl Pts',(-3.41336191777647,2.50103951622967,4.78515751307969));
#16662=CARTESIAN_POINT('Ctrl Pts',(-3.41388890712174,2.29799304590536,4.77404372402289));
#16663=CARTESIAN_POINT('Ctrl Pts',(-3.58476549042184,2.18831469750142,4.76292993496608));
#16664=CARTESIAN_POINT('Ctrl Pts',(-3.76958639310991,2.27239430714904,4.75181614590928));
#16665=CARTESIAN_POINT('Ctrl Pts',(-3.79918294694398,2.47327285461012,4.74070235685247));
#16666=CARTESIAN_POINT('Ctrl Pts',(-3.64646509055197,2.60708392727588,4.72958856779567));
#16667=CARTESIAN_POINT('Ctrl Pts',(-3.45121720982778,2.55134873281456,4.71847477873886));
#16668=CARTESIAN_POINT('Ctrl Pts',(-3.39215190425982,2.3570823267967,4.70736098968206));
#16669=CARTESIAN_POINT('Ctrl Pts',(-3.52333231788058,2.20209895378134,4.69624720062526));
#16670=CARTESIAN_POINT('Ctrl Pts',(-3.7246875304159,2.22825665272044,4.68513341156845));
#16671=CARTESIAN_POINT('Ctrl Pts',(-3.81191483230877,2.41161298512653,4.67401962251165));
#16672=CARTESIAN_POINT('Ctrl Pts',(-3.70517408491178,2.58433982054614,4.66290583345484));
#16673=CARTESIAN_POINT('Ctrl Pts',(-3.50216630483977,2.58833832766402,4.65179204439804));
#16674=CARTESIAN_POINT('Ctrl Pts',(-3.38870681545753,2.41994862756931,4.64067825534123));
#16675=CARTESIAN_POINT('Ctrl Pts',(-3.46864637411461,2.23329972242719,4.62956446628443));
#16676=CARTESIAN_POINT('Ctrl Pts',(-3.6688153961962,2.19923347185799,4.61845067722763));
#16677=CARTESIAN_POINT('Ctrl Pts',(-3.80599690571939,2.34893110134286,4.60733688817082));
#16678=CARTESIAN_POINT('Ctrl Pts',(-3.7546271112745,2.54537267293252,4.59622309911402));
#16679=CARTESIAN_POINT('Ctrl Pts',(-3.56172536828799,2.60875298834237,4.58510931005721));
#16680=CARTESIAN_POINT('Ctrl Pts',(-3.40385682977405,2.48105932611543,4.57399552100042));
#16681=CARTESIAN_POINT('Ctrl Pts',(-3.42552035937731,2.27917114339395,4.5628817319436));
#16682=CARTESIAN_POINT('Ctrl Pts',(-3.60688708278715,2.18787898346807,4.5517679428868));
#16683=CARTESIAN_POINT('Ctrl Pts',(-3.7819499811952,2.2907435954864,4.54065415383));
#16684=CARTESIAN_POINT('Ctrl Pts',(-3.79047199840596,2.49361183381496,4.52954036477319));
#16685=CARTESIAN_POINT('Ctrl Pts',(-3.62465283528865,2.61079609860775,4.51842657571639));
#16686=CARTESIAN_POINT('Ctrl Pts',(-3.43626865262511,2.53503630458453,4.50731278665958));
#16687=CARTESIAN_POINT('Ctrl Pts',(-3.39774962870189,2.33567624789731,4.49619899760278));
#16688=CARTESIAN_POINT('Ctrl Pts',(-3.54435266400721,2.19519245431826,4.48508520854598));
#16689=CARTESIAN_POINT('Ctrl Pts',(-3.74189033562052,2.24217132331451,4.47397141948917));
#16690=CARTESIAN_POINT('Ctrl Pts',(-3.80955417671754,2.43361258332043,4.46285763043237));
#16691=CARTESIAN_POINT('Ctrl Pts',(-3.68541069770656,2.59428783790942,4.45174384137556));
#16692=CARTESIAN_POINT('Ctrl Pts',(-3.48308984977921,2.57712928456848,4.44063005231877));
#16693=CARTESIAN_POINT('Ctrl Pts',(-3.38777816553941,2.39784218119362,4.42951626326195));
#16694=CARTESIAN_POINT('Ctrl Pts',(-3.48671557851344,2.22053036825651,4.41840247420515));
#16695=CARTESIAN_POINT('Ctrl Pts',(-3.68934341635898,2.20748871526871,4.40728868514834));
#16696=CARTESIAN_POINT('Ctrl Pts',(-3.81019439388853,2.37065568400947,4.39617489609154));
#16697=CARTESIAN_POINT('Ctrl Pts',(-3.73865169471375,2.56068011684939,4.38506110703474));
#16698=CARTESIAN_POINT('Ctrl Pts',(-3.54020025619518,2.60363566261151,4.37394731797793));
#16699=CARTESIAN_POINT('Ctrl Pts',(-3.3964827412202,2.46019427700244,4.36283352892113));
#16700=CARTESIAN_POINT('Ctrl Pts',(-3.43904980483436,2.26167020258818,4.35171973986432));
#16701=CARTESIAN_POINT('Ctrl Pts',(-3.62893055336078,2.18973329784341,4.34060595080752));
#16702=CARTESIAN_POINT('Ctrl Pts',(-3.79234256300291,2.3103112823848,4.32949216175072));
#16703=CARTESIAN_POINT('Ctrl Pts',(-3.77967772199614,2.5128713982991,4.31837837269391));
#16704=CARTESIAN_POINT('Ctrl Pts',(-3.60259956184262,2.61234204743659,4.30726458363711));
#16705=CARTESIAN_POINT('Ctrl Pts',(-3.42303927044789,2.51699697749597,4.2961507945803));
#16706=CARTESIAN_POINT('Ctrl Pts',(-3.41156124805062,2.38276609266137,4.28874160187577));
#16707=CARTESIAN_POINT('Ctrl Pts',(-3.43548292594103,2.32806025151199,4.2850370055235));
#16708=CARTESIAN_POINT('Ctrl Pts',(-3.45335096305347,2.52472660865709,5.2149629944765));
#16709=CARTESIAN_POINT('Ctrl Pts',(-3.41187639830495,2.47596231494597,5.21125839812423));
#16710=CARTESIAN_POINT('Ctrl Pts',(-3.38215237366538,2.33461052038716,5.20384920541969));
#16711=CARTESIAN_POINT('Ctrl Pts',(-3.53700740426192,2.18120409086806,5.19273541636289));
#16712=CARTESIAN_POINT('Ctrl Pts',(-3.7495560186915,2.22856458779753,5.18162162730609));
#16713=CARTESIAN_POINT('Ctrl Pts',(-3.82519436251124,2.43259816228878,5.17050783824928));
#16714=CARTESIAN_POINT('Ctrl Pts',(-3.69471991948189,2.60691546421531,5.15939404919248));
#16715=CARTESIAN_POINT('Ctrl Pts',(-3.47754216800657,2.59178020350553,5.14828026013568));
#16716=CARTESIAN_POINT('Ctrl Pts',(-3.37245400310457,2.4011365565164,5.13716647107886));
#16717=CARTESIAN_POINT('Ctrl Pts',(-3.47563999896949,2.20943751922385,5.12605268202207));
#16718=CARTESIAN_POINT('Ctrl Pts',(-3.69265474877542,2.19217001681392,5.11493889296526));
#16719=CARTESIAN_POINT('Ctrl Pts',(-3.82486123927823,2.36512789166097,5.10382510390846));
#16720=CARTESIAN_POINT('Ctrl Pts',(-3.75124984567759,2.57000648228012,5.09271131485165));
#16721=CARTESIAN_POINT('Ctrl Pts',(-3.53919767397361,2.61927527295602,5.08159752579485));
#16722=CARTESIAN_POINT('Ctrl Pts',(-3.38279860031468,2.46783938836956,5.07048373673804));
#16723=CARTESIAN_POINT('Ctrl Pts',(-3.42520641129747,2.25430910810904,5.05936994768124));
#16724=CARTESIAN_POINT('Ctrl Pts',(-3.62760478616353,2.17413147038572,5.04825615862444));
#16725=CARTESIAN_POINT('Ctrl Pts',(-3.80473618227523,2.30069380093641,5.03714236956763));
#16726=CARTESIAN_POINT('Ctrl Pts',(-3.79447023134107,2.51815225086865,5.02602858051083));
#16727=CARTESIAN_POINT('Ctrl Pts',(-3.60620347099095,2.62746459107471,5.01491479145402));
#16728=CARTESIAN_POINT('Ctrl Pts',(-3.4122586039035,2.52857601872219,5.00380100239722));
#16729=CARTESIAN_POINT('Ctrl Pts',(-3.39015556548935,2.31200035464812,4.99268721334042));
#16730=CARTESIAN_POINT('Ctrl Pts',(-3.56012551793341,2.17597176576338,4.98157342428361));
#16731=CARTESIAN_POINT('Ctrl Pts',(-3.76659303594405,2.24499875942197,4.9704596352268));
#16732=CARTESIAN_POINT('Ctrl Pts',(-3.82057605889971,2.45590014686796,4.95934584617));
#16733=CARTESIAN_POINT('Ctrl Pts',(-3.67266331362277,2.61563549570883,4.94823205711319));
#16734=CARTESIAN_POINT('Ctrl Pts',(-3.4582410133384,2.57799722996748,4.93711826805639));
#16735=CARTESIAN_POINT('Ctrl Pts',(-3.37357232119689,2.37743608095462,4.92600447899959));
#16736=CARTESIAN_POINT('Ctrl Pts',(-3.49615545133077,2.19752794296441,4.91489068994278));
#16737=CARTESIAN_POINT('Ctrl Pts',(-3.71378867453769,2.20294477495411,4.90377690088598));
#16738=CARTESIAN_POINT('Ctrl Pts',(-3.82726983348952,2.38872848919359,4.89266311182918));
#16739=CARTESIAN_POINT('Ctrl Pts',(-3.73272833643288,2.58482914509829,4.88154932277237));
#16740=CARTESIAN_POINT('Ctrl Pts',(-3.51669908779767,2.61175358839122,4.87043553371557));
#16741=CARTESIAN_POINT('Ctrl Pts',(-3.37691610879776,2.44485757077975,4.85932174465876));
#16742=CARTESIAN_POINT('Ctrl Pts',(-3.44132434535872,2.23690290991458,4.84820795560196));
#16743=CARTESIAN_POINT('Ctrl Pts',(-3.65097020811712,2.17823286525116,4.83709416654515));
#16744=CARTESIAN_POINT('Ctrl Pts',(-3.81396246134447,2.32254879403384,4.82598037748835));
#16745=CARTESIAN_POINT('Ctrl Pts',(-3.78111244720387,2.5377566899937,4.81486658843155));
#16746=CARTESIAN_POINT('Ctrl Pts',(-3.58248815618272,2.62687432533523,4.80375279937474));
#16747=CARTESIAN_POINT('Ctrl Pts',(-3.39989265440535,2.50833131776757,4.79263901031794));
#16748=CARTESIAN_POINT('Ctrl Pts',(-3.4004576754224,2.29063142648655,4.78152522126113));
#16749=CARTESIAN_POINT('Ctrl Pts',(-3.58366604908921,2.17303783086637,4.77041143220433));
#16750=CARTESIAN_POINT('Ctrl Pts',(-3.78182507326426,2.26318528258027,4.75929764314753));
#16751=CARTESIAN_POINT('Ctrl Pts',(-3.81355754584396,2.47856079673287,4.74818385409072));
#16752=CARTESIAN_POINT('Ctrl Pts',(-3.64981837480538,2.62202872269584,4.73707006503392));
#16753=CARTESIAN_POINT('Ctrl Pts',(-3.44047988032865,2.56227124079834,4.72595627597711));
#16754=CARTESIAN_POINT('Ctrl Pts',(-3.3771519604683,2.35398505191708,4.71484248692031));
#16755=CARTESIAN_POINT('Ctrl Pts',(-3.51779937845998,2.18781686686112,4.7037286978635));
#16756=CARTESIAN_POINT('Ctrl Pts',(-3.73368595756569,2.21586230988758,4.6926149088067));
#16757=CARTESIAN_POINT('Ctrl Pts',(-3.82720826360965,2.41245106893735,4.6815011197499));
#16758=CARTESIAN_POINT('Ctrl Pts',(-3.71276426925474,2.59764322338409,4.67038733069309));
#16759=CARTESIAN_POINT('Ctrl Pts',(-3.49510586041716,2.60193029404067,4.65927354163629));
#16760=CARTESIAN_POINT('Ctrl Pts',(-3.37345824712023,2.42138827651674,4.64815975257948));
#16761=CARTESIAN_POINT('Ctrl Pts',(-3.4591668693923,2.22126932693707,4.63704596352268));
#16762=CARTESIAN_POINT('Ctrl Pts',(-3.67378165326609,2.18474458935644,4.62593217446588));
#16763=CARTESIAN_POINT('Ctrl Pts',(-3.82086325316422,2.34524557029854,4.61481838540907));
#16764=CARTESIAN_POINT('Ctrl Pts',(-3.7657862126822,2.55586390170729,4.60370459635227));
#16765=CARTESIAN_POINT('Ctrl Pts',(-3.55896317158719,2.6238182362596,4.59259080729546));
#16766=CARTESIAN_POINT('Ctrl Pts',(-3.38970160493063,2.48690920090586,4.58147701823866));
#16767=CARTESIAN_POINT('Ctrl Pts',(-3.41292854422122,2.27045118831796,4.57036322918185));
#16768=CARTESIAN_POINT('Ctrl Pts',(-3.60738410853246,2.17257067230145,4.55924944012505));
#16769=CARTESIAN_POINT('Ctrl Pts',(-3.79508091453898,2.28285879904056,4.54813565106825));
#16770=CARTESIAN_POINT('Ctrl Pts',(-3.80421794714692,2.50036759571139,4.53702186201144));
#16771=CARTESIAN_POINT('Ctrl Pts',(-3.62643197664818,2.62600879333718,4.52590807295464));
#16772=CARTESIAN_POINT('Ctrl Pts',(-3.42445251835268,2.54478158019733,4.51479428389783));
#16773=CARTESIAN_POINT('Ctrl Pts',(-3.38315366047576,2.3310341429862,4.50368049484103));
#16774=CARTESIAN_POINT('Ctrl Pts',(-3.54033671712511,2.18041194039358,4.49256670578422));
#16775=CARTESIAN_POINT('Ctrl Pts',(-3.75213025170582,2.23078117191311,4.48145291672742));
#16776=CARTESIAN_POINT('Ctrl Pts',(-3.82467724465257,2.43603833015588,4.47033912767062));
#16777=CARTESIAN_POINT('Ctrl Pts',(-3.69157460149519,2.60830916746569,4.45922533861381));
#16778=CARTESIAN_POINT('Ctrl Pts',(-3.47465269919707,2.58991231874976,4.44811154955701));
#16779=CARTESIAN_POINT('Ctrl Pts',(-3.37246257856274,2.39768645611616,4.4369977605002));
#16780=CARTESIAN_POINT('Ctrl Pts',(-3.47854008886701,2.20757843632347,4.4258839714434));
#16781=CARTESIAN_POINT('Ctrl Pts',(-3.69579113587624,2.19359559568096,4.41477018238659));
#16782=CARTESIAN_POINT('Ctrl Pts',(-3.82536366490058,2.36853796871893,4.4036563933298));
#16783=CARTESIAN_POINT('Ctrl Pts',(-3.74865788514769,2.57227605046896,4.39254260427298));
#16784=CARTESIAN_POINT('Ctrl Pts',(-3.5358846390969,2.61833160429067,4.38142881521619));
#16785=CARTESIAN_POINT('Ctrl Pts',(-3.38179534448736,2.46453836670119,4.37031502615938));
#16786=CARTESIAN_POINT('Ctrl Pts',(-3.4274343802517,2.25168724278053,4.35920123710257));
#16787=CARTESIAN_POINT('Ctrl Pts',(-3.63101840830467,2.17455880850134,4.34808744804577));
#16788=CARTESIAN_POINT('Ctrl Pts',(-3.80622350631146,2.30383864322893,4.33697365898897));
#16789=CARTESIAN_POINT('Ctrl Pts',(-3.79264467134891,2.52101708096281,4.32585986993216));
#16790=CARTESIAN_POINT('Ctrl Pts',(-3.60278716655164,2.62766630992157,4.31474608087536));
#16791=CARTESIAN_POINT('Ctrl Pts',(-3.41026840051456,2.5254403942132,4.30363229181855));
#16792=CARTESIAN_POINT('Ctrl Pts',(-3.3979620342723,2.38152235915268,4.29622309911402));
#16793=CARTESIAN_POINT('Ctrl Pts',(-3.42361008748734,2.32286851675082,4.29251850276175));
#16794=CARTESIAN_POINT('Ctrl Pts',(-3.44347998857283,2.53312198033322,5.22244449171475));
#16795=CARTESIAN_POINT('Ctrl Pts',(-3.39921376300775,2.48107535276698,5.21873989536248));
#16796=CARTESIAN_POINT('Ctrl Pts',(-3.36748900863419,2.33020914211697,5.21133070265795));
#16797=CARTESIAN_POINT('Ctrl Pts',(-3.53276736069978,2.16647689674201,5.20021691360114));
#16798=CARTESIAN_POINT('Ctrl Pts',(-3.75962266266454,2.21702523769905,5.18910312454434));
#16799=CARTESIAN_POINT('Ctrl Pts',(-3.84035223774737,2.43479235077285,5.17798933548753));
#16800=CARTESIAN_POINT('Ctrl Pts',(-3.70109553522054,2.62084298334156,5.16687554643073));
#16801=CARTESIAN_POINT('Ctrl Pts',(-3.46929950811782,2.60468896536386,5.15576175737392));
#16802=CARTESIAN_POINT('Ctrl Pts',(-3.35713783891219,2.401213058351,5.14464796831712));
#16803=CARTESIAN_POINT('Ctrl Pts',(-3.46726930372222,2.19661072251331,5.13353417926031));
#16804=CARTESIAN_POINT('Ctrl Pts',(-3.69889135748228,2.17818094124235,5.12242039020352));
#16805=CARTESIAN_POINT('Ctrl Pts',(-3.83999669192638,2.36278064343714,5.1113066011467));
#16806=CARTESIAN_POINT('Ctrl Pts',(-3.76143050146621,2.5814496508346,5.1001928120899));
#16807=CARTESIAN_POINT('Ctrl Pts',(-3.53510505788101,2.63403473315196,5.0890790230331));
#16808=CARTESIAN_POINT('Ctrl Pts',(-3.36817873292179,2.47240567046266,5.07796523397629));
#16809=CARTESIAN_POINT('Ctrl Pts',(-3.41344102170209,2.24450262655374,5.06685144491949));
#16810=CARTESIAN_POINT('Ctrl Pts',(-3.6294628695539,2.15892821683407,5.05573765586269));
#16811=CARTESIAN_POINT('Ctrl Pts',(-3.81851701352091,2.29400948184958,5.04462386680588));
#16812=CARTESIAN_POINT('Ctrl Pts',(-3.80756005948302,2.52610510127557,5.03351007774908));
#16813=CARTESIAN_POINT('Ctrl Pts',(-3.60662102779949,2.64277527582587,5.02239628869227));
#16814=CARTESIAN_POINT('Ctrl Pts',(-3.39962169493761,2.53723049491962,5.01128249963547));
#16815=CARTESIAN_POINT('Ctrl Pts',(-3.3760308968172,2.30607708183528,5.00016871057867));
#16816=CARTESIAN_POINT('Ctrl Pts',(-3.55744155898554,2.16089238284251,4.98905492152186));
#16817=CARTESIAN_POINT('Ctrl Pts',(-3.77780644477848,2.23456559653136,4.97794113246506));
#16818=CARTESIAN_POINT('Ctrl Pts',(-3.83542307524414,2.45966279635197,4.96682734340825));
#16819=CARTESIAN_POINT('Ctrl Pts',(-3.67755429503925,2.63014996180817,4.95571355435145));
#16820=CARTESIAN_POINT('Ctrl Pts',(-3.44869918906956,2.58997825726379,4.94459976529464));
#16821=CARTESIAN_POINT('Ctrl Pts',(-3.35833143120733,2.37591729928569,4.93348597623784));
#16822=CARTESIAN_POINT('Ctrl Pts',(-3.48916565507154,2.18389951041786,4.92237218718103));
#16823=CARTESIAN_POINT('Ctrl Pts',(-3.72144781179447,2.18968095039579,4.91125839812423));
#16824=CARTESIAN_POINT('Ctrl Pts',(-3.84256740907069,2.38796980166419,4.90014460906742));
#16825=CARTESIAN_POINT('Ctrl Pts',(-3.74166230592267,2.59727002989735,4.88903082001062));
#16826=CARTESIAN_POINT('Ctrl Pts',(-3.51109208760397,2.62600676257303,4.87791703095382));
#16827=CARTESIAN_POINT('Ctrl Pts',(-3.36190028978558,2.44787694237367,4.86680324189701));
#16828=CARTESIAN_POINT('Ctrl Pts',(-3.43064385696086,2.2259248138587,4.85568945284022));
#16829=CARTESIAN_POINT('Ctrl Pts',(-3.65440102248913,2.16330567736551,4.8445756637834));
#16830=CARTESIAN_POINT('Ctrl Pts',(-3.82836431518356,2.31733553867597,4.8334618747266));
#16831=CARTESIAN_POINT('Ctrl Pts',(-3.79330316036299,2.54702911891502,4.8223480856698));
#16832=CARTESIAN_POINT('Ctrl Pts',(-3.58130943065524,2.64214527918755,4.81123429661299));
#16833=CARTESIAN_POINT('Ctrl Pts',(-3.38642339103422,2.51562311930547,4.80012050755619));
#16834=CARTESIAN_POINT('Ctrl Pts',(-3.38702644372307,2.28326980706774,4.78900671849939));
#16835=CARTESIAN_POINT('Ctrl Pts',(-3.58256660775658,2.15776096423133,4.77789292944257));
#16836=CARTESIAN_POINT('Ctrl Pts',(-3.79406375341862,2.2539762580115,4.76677914038578));
#16837=CARTESIAN_POINT('Ctrl Pts',(-3.82793214474394,2.48384873885561,4.75566535132897));
#16838=CARTESIAN_POINT('Ctrl Pts',(-3.65317165905879,2.6369735181158,4.74455156227217));
#16839=CARTESIAN_POINT('Ctrl Pts',(-3.42974255082951,2.57319374878213,4.73343777321536));
#16840=CARTESIAN_POINT('Ctrl Pts',(-3.36215201667677,2.35088777703746,4.72232398415856));
#16841=CARTESIAN_POINT('Ctrl Pts',(-3.51226643903938,2.1735347799409,4.71121019510176));
#16842=CARTESIAN_POINT('Ctrl Pts',(-3.74268438471549,2.20346796705471,4.70009640604495));
#16843=CARTESIAN_POINT('Ctrl Pts',(-3.84250169491054,2.41328915274817,4.68898261698815));
#16844=CARTESIAN_POINT('Ctrl Pts',(-3.7203544535977,2.61094662622203,4.67786882793133));
#16845=CARTESIAN_POINT('Ctrl Pts',(-3.48804541599454,2.61552226041731,4.66675503887454));
#16846=CARTESIAN_POINT('Ctrl Pts',(-3.35820967878295,2.42282792546417,4.65564124981773));
#16847=CARTESIAN_POINT('Ctrl Pts',(-3.44968736466998,2.20923893144694,4.64452746076093));
#16848=CARTESIAN_POINT('Ctrl Pts',(-3.67874791033599,2.17025570685489,4.63341367170413));
#16849=CARTESIAN_POINT('Ctrl Pts',(-3.83572960060904,2.34156003925422,4.62229988264732));
#16850=CARTESIAN_POINT('Ctrl Pts',(-3.77694531408991,2.56635513048207,4.61118609359051));
#16851=CARTESIAN_POINT('Ctrl Pts',(-3.55620097488638,2.63888348417682,4.60007230453371));
#16852=CARTESIAN_POINT('Ctrl Pts',(-3.3755463800872,2.4927590756963,4.58895851547691));
#16853=CARTESIAN_POINT('Ctrl Pts',(-3.40033672906513,2.26173123324197,4.5778447264201));
#16854=CARTESIAN_POINT('Ctrl Pts',(-3.60788113427776,2.15726236113484,4.5667309373633));
#16855=CARTESIAN_POINT('Ctrl Pts',(-3.80821184788277,2.27497400259471,4.55561714830649));
#16856=CARTESIAN_POINT('Ctrl Pts',(-3.81796389588787,2.50712335760782,4.54450335924969));
#16857=CARTESIAN_POINT('Ctrl Pts',(-3.62821111800771,2.64122148806661,4.53338957019289));
#16858=CARTESIAN_POINT('Ctrl Pts',(-3.41263638408026,2.55452685581013,4.52227578113608));
#16859=CARTESIAN_POINT('Ctrl Pts',(-3.36855769224962,2.32639203807509,4.51116199207928));
#16860=CARTESIAN_POINT('Ctrl Pts',(-3.536320770243,2.1656314264689,4.50004820302247));
#16861=CARTESIAN_POINT('Ctrl Pts',(-3.76237016779111,2.21939102051171,4.48893441396567));
#16862=CARTESIAN_POINT('Ctrl Pts',(-3.83980031258758,2.43846407699132,4.47782062490887));
#16863=CARTESIAN_POINT('Ctrl Pts',(-3.69773850528383,2.62233049702197,4.46670683585206));
#16864=CARTESIAN_POINT('Ctrl Pts',(-3.46621554861493,2.60269535293104,4.45559304679526));
#16865=CARTESIAN_POINT('Ctrl Pts',(-3.35714699158608,2.39753073103871,4.44447925773845));
#16866=CARTESIAN_POINT('Ctrl Pts',(-3.47036459922058,2.19462650439043,4.43336546868165));
#16867=CARTESIAN_POINT('Ctrl Pts',(-3.70223885539349,2.17970247609322,4.42225167962484));
#16868=CARTESIAN_POINT('Ctrl Pts',(-3.84053293591263,2.36642025342839,4.41113789056805));
#16869=CARTESIAN_POINT('Ctrl Pts',(-3.75866407558161,2.58387198408852,4.40002410151123));
#16870=CARTESIAN_POINT('Ctrl Pts',(-3.53156902199863,2.63302754596983,4.38891031245443));
#16871=CARTESIAN_POINT('Ctrl Pts',(-3.36710794775451,2.46888245639993,4.37779652339763));
#16872=CARTESIAN_POINT('Ctrl Pts',(-3.41581895566904,2.24170428297288,4.36668273434082));
#16873=CARTESIAN_POINT('Ctrl Pts',(-3.63310626324856,2.15938431915927,4.35556894528402));
#16874=CARTESIAN_POINT('Ctrl Pts',(-3.82010444962002,2.29736600407305,4.34445515622722));
#16875=CARTESIAN_POINT('Ctrl Pts',(-3.80561162070166,2.52916276362653,4.33334136717041));
#16876=CARTESIAN_POINT('Ctrl Pts',(-3.60297477126067,2.64299057240655,4.32222757811361));
#16877=CARTESIAN_POINT('Ctrl Pts',(-3.39749753058122,2.53388381093044,4.3111137890568));
#16878=CARTESIAN_POINT('Ctrl Pts',(-3.38436282049399,2.380278625644,4.30370459635227));
#16879=CARTESIAN_POINT('Ctrl Pts',(-3.41173724903364,2.31767678198965,4.3));
#16880=CARTESIAN_POINT('Ctrl Pts',(-3.47309291201476,2.50793586530485,5.2));
#16881=CARTESIAN_POINT('Ctrl Pts',(-3.46488109712516,2.50027511355887,5.2));
#16882=CARTESIAN_POINT('Ctrl Pts',(-3.45756392397337,2.49177395403935,5.2));
#16883=CARTESIAN_POINT('Ctrl Pts',(-3.45114582175476,2.48262659215394,5.2));
#16884=CARTESIAN_POINT('Ctrl Pts',(-3.44637505636198,2.47582708724863,5.2));
#16885=CARTESIAN_POINT('Ctrl Pts',(-3.44210140258396,2.46866923691254,5.2));
#16886=CARTESIAN_POINT('Ctrl Pts',(-3.4383368615674,2.46121837901648,5.2));
#16887=CARTESIAN_POINT('Ctrl Pts',(-3.43611956164057,2.45682985287343,5.2));
#16888=CARTESIAN_POINT('Ctrl Pts',(-3.43407749071882,2.45233446363919,5.2));
#16889=CARTESIAN_POINT('Ctrl Pts',(-3.4322255599542,2.44777399682775,5.2));
#16890=CARTESIAN_POINT('Ctrl Pts',(-3.42766722424942,2.43654888026604,5.2));
#16891=CARTESIAN_POINT('Ctrl Pts',(-3.42424189960471,2.42490562017205,5.2));
#16892=CARTESIAN_POINT('Ctrl Pts',(-3.42197767565222,2.41304271238881,5.2));
#16893=CARTESIAN_POINT('Ctrl Pts',(-3.42053879301361,2.40550400048974,5.2));
#16894=CARTESIAN_POINT('Ctrl Pts',(-3.41956954249672,2.39787570455109,5.2));
#16895=CARTESIAN_POINT('Ctrl Pts',(-3.41908669765048,2.39020364672881,5.2));
#16896=CARTESIAN_POINT('Ctrl Pts',(-3.4188613702662,2.3866233564252,5.2));
#16897=CARTESIAN_POINT('Ctrl Pts',(-3.4187425132976,2.38303698501937,5.2));
#16898=CARTESIAN_POINT('Ctrl Pts',(-3.4187312729093,2.37945933257344,5.2));
#16899=CARTESIAN_POINT('Ctrl Pts',(-3.41869622423253,2.36830384747272,5.2));
#16900=CARTESIAN_POINT('Ctrl Pts',(-3.4197031160267,2.35720597826242,5.2));
#16901=CARTESIAN_POINT('Ctrl Pts',(-3.42178566785009,2.34630687436894,5.2));
#16902=CARTESIAN_POINT('Ctrl Pts',(-3.42294604955552,2.3402339783087,5.2));
#16903=CARTESIAN_POINT('Ctrl Pts',(-3.42444092603953,2.33422255306027,5.2));
#16904=CARTESIAN_POINT('Ctrl Pts',(-3.42625156753842,2.32828873958556,5.2));
#16905=CARTESIAN_POINT('Ctrl Pts',(-3.42738421175614,2.32457685099508,5.2));
#16906=CARTESIAN_POINT('Ctrl Pts',(-3.42864107094821,2.32089381471682,5.2));
#16907=CARTESIAN_POINT('Ctrl Pts',(-3.4300164442918,2.31724844575858,5.2));
#16908=CARTESIAN_POINT('Ctrl Pts',(-3.43439823178552,2.30563470307137,5.2));
#16909=CARTESIAN_POINT('Ctrl Pts',(-3.43994733372525,2.29448387749046,5.2));
#16910=CARTESIAN_POINT('Ctrl Pts',(-3.44649833143843,2.28391851131164,5.2));
#16911=CARTESIAN_POINT('Ctrl Pts',(-3.45083930540137,2.27691744345919,5.2));
#16912=CARTESIAN_POINT('Ctrl Pts',(-3.45562139981211,2.27017330264703,5.2));
#16913=CARTESIAN_POINT('Ctrl Pts',(-3.46080803162185,2.26372396193311,5.2));
#16914=CARTESIAN_POINT('Ctrl Pts',(-3.46351816065219,2.2603540397685,5.2));
#16915=CARTESIAN_POINT('Ctrl Pts',(-3.46634013864158,2.25706328802701,5.2));
#16916=CARTESIAN_POINT('Ctrl Pts',(-3.46926558695491,2.25386191331523,5.2));
#16917=CARTESIAN_POINT('Ctrl Pts',(-3.47553201369268,2.24700444124844,5.2));
#16918=CARTESIAN_POINT('Ctrl Pts',(-3.48224798017073,2.24058272300471,5.2));
#16919=CARTESIAN_POINT('Ctrl Pts',(-3.48935940275436,2.23464751188384,5.2));
#16920=CARTESIAN_POINT('Ctrl Pts',(-3.49388585721574,2.23086972163985,5.2));
#16921=CARTESIAN_POINT('Ctrl Pts',(-3.49857277644925,2.2272891074735,5.2));
#16922=CARTESIAN_POINT('Ctrl Pts',(-3.50340840926684,2.2239201748241,5.2));
#16923=CARTESIAN_POINT('Ctrl Pts',(-3.50748096973522,2.22108286635877,5.2));
#16924=CARTESIAN_POINT('Ctrl Pts',(-3.51165201299164,2.21840074277452,5.2));
#16925=CARTESIAN_POINT('Ctrl Pts',(-3.51591072169151,2.21588342574414,5.2));
#16926=CARTESIAN_POINT('Ctrl Pts',(-3.52463381704441,2.21072721571968,5.2));
#16927=CARTESIAN_POINT('Ctrl Pts',(-3.53372795060187,2.20625881994954,5.2));
#16928=CARTESIAN_POINT('Ctrl Pts',(-3.54313435341931,2.20255201733462,5.2));
#16929=CARTESIAN_POINT('Ctrl Pts',(-3.5443736619696,2.20206364018726,5.2));
#16930=CARTESIAN_POINT('Ctrl Pts',(-3.54561840623672,2.20158850319392,5.2));
#16931=CARTESIAN_POINT('Ctrl Pts',(-3.54686839490754,2.2011265482535,5.2));
#16932=CARTESIAN_POINT('Ctrl Pts',(-3.76673280722786,2.39986996770474,5.08714803633902));
#16933=CARTESIAN_POINT('Ctrl Pts',(-3.76680595967625,2.39134538779314,5.08771939403666));
#16934=CARTESIAN_POINT('Ctrl Pts',(-3.76620865205667,2.38283109327188,5.08829075173431));
#16935=CARTESIAN_POINT('Ctrl Pts',(-3.76490523356496,2.37442631092714,5.08886210943196));
#16936=CARTESIAN_POINT('Ctrl Pts',(-3.75645406644185,2.31993098139145,5.09256670578422));
#16937=CARTESIAN_POINT('Ctrl Pts',(-3.71831779890178,2.27003957467425,5.0962713021365));
#16938=CARTESIAN_POINT('Ctrl Pts',(-3.66794964148213,2.24758436209697,5.09997589848877));
#16939=CARTESIAN_POINT('Ctrl Pts',(-3.61758148406248,2.22512914951968,5.10368049484103));
#16940=CARTESIAN_POINT('Ctrl Pts',(-3.55498143676326,2.2301101310823,5.1073850911933));
#16941=CARTESIAN_POINT('Ctrl Pts',(-3.50879890345119,2.26024936189732,5.11108968754557));
#16942=CARTESIAN_POINT('Ctrl Pts',(-3.46261637013913,2.29038859271235,5.11479428389783));
#16943=CARTESIAN_POINT('Ctrl Pts',(-3.43285135081423,2.34568607277977,5.1184988802501));
#16944=CARTESIAN_POINT('Ctrl Pts',(-3.43312570053424,2.40083133397043,5.12220347660237));
#16945=CARTESIAN_POINT('Ctrl Pts',(-3.43340005025424,2.45597659516109,5.12590807295464));
#16946=CARTESIAN_POINT('Ctrl Pts',(-3.46371376901915,2.51096963747498,5.12961266930691));
#16947=CARTESIAN_POINT('Ctrl Pts',(-3.51019416177169,2.54064911632758,5.13331726565918));
#16948=CARTESIAN_POINT('Ctrl Pts',(-3.55667455452423,2.57032859518018,5.13702186201145));
#16949=CARTESIAN_POINT('Ctrl Pts',(-3.61932162126441,2.57469451057149,5.14072645836371));
#16950=CARTESIAN_POINT('Ctrl Pts',(-3.6694634753069,2.55173569482678,5.14443105471598));
#16951=CARTESIAN_POINT('Ctrl Pts',(-3.71960532934939,2.52877687908207,5.14813565106825));
#16952=CARTESIAN_POINT('Ctrl Pts',(-3.75724197069419,2.47849333220135,5.15184024742052));
#16953=CARTESIAN_POINT('Ctrl Pts',(-3.76515097781766,2.42392380920663,5.15554484377278));
#16954=CARTESIAN_POINT('Ctrl Pts',(-3.76629187237323,2.41605201560311,5.15607924129486));
#16955=CARTESIAN_POINT('Ctrl Pts',(-3.76681417046854,2.40809103597041,5.15661363881694));
#16956=CARTESIAN_POINT('Ctrl Pts',(-3.76674783252531,2.40012156540224,5.15714803633902));
#16957=CARTESIAN_POINT('Ctrl Pts',(-3.65301702171886,2.20148256743283,5.2));
#16958=CARTESIAN_POINT('Ctrl Pts',(-3.71902879097456,2.21911198848201,5.19629540364773));
#16959=CARTESIAN_POINT('Ctrl Pts',(-3.83093279751213,2.32515241961692,5.1888862109432));
#16960=CARTESIAN_POINT('Ctrl Pts',(-3.78812294461068,2.55382789975093,5.17777242188639));
#16961=CARTESIAN_POINT('Ctrl Pts',(-3.57278676575927,2.64128531597693,5.16665863282959));
#16962=CARTESIAN_POINT('Ctrl Pts',(-3.38252462806861,2.5080933346037,5.15554484377278));
#16963=CARTESIAN_POINT('Ctrl Pts',(-3.39123766596766,2.27586209704876,5.14443105471597));
#16964=CARTESIAN_POINT('Ctrl Pts',(-3.59107442724388,2.15730569128375,5.13331726565918));
#16965=CARTESIAN_POINT('Ctrl Pts',(-3.79906029518588,2.2608651698129,5.12220347660237));
#16966=CARTESIAN_POINT('Ctrl Pts',(-3.82485429121136,2.49178880612566,5.11108968754556));
#16967=CARTESIAN_POINT('Ctrl Pts',(-3.64483147349944,2.63869087951471,5.09997589848877));
#16968=CARTESIAN_POINT('Ctrl Pts',(-3.42377646220466,2.56711959422357,5.08886210943196));
#16969=CARTESIAN_POINT('Ctrl Pts',(-3.36401957377094,2.34258029572384,5.07774832037515));
#16970=CARTESIAN_POINT('Ctrl Pts',(-3.52025888482579,2.17059867951396,5.06663453131835));
#16971=CARTESIAN_POINT('Ctrl Pts',(-3.74948582371233,2.20859030608788,5.05552074226155));
#16972=CARTESIAN_POINT('Ctrl Pts',(-3.8418868522934,2.42178158973285,5.04440695320474));
#16973=CARTESIAN_POINT('Ctrl Pts',(-3.71288602216703,2.61503584063672,5.03329316414794));
#16974=CARTESIAN_POINT('Ctrl Pts',(-3.48055937550073,2.61146539619723,5.02217937509113));
#16975=CARTESIAN_POINT('Ctrl Pts',(-3.35755806712823,2.4143382523336,5.01106558603433));
#16976=CARTESIAN_POINT('Ctrl Pts',(-3.45646661930996,2.20408715554039,4.99995179697752));
#16977=CARTESIAN_POINT('Ctrl Pts',(-3.68675289766315,2.17315730107164,4.98883800792072));
#16978=CARTESIAN_POINT('Ctrl Pts',(-3.83763326741432,2.34985914450584,4.97772421886391));
#16979=CARTESIAN_POINT('Ctrl Pts',(-3.77100521132112,2.57245548011022,4.96661042980712));
#16980=CARTESIAN_POINT('Ctrl Pts',(-3.54785414659174,2.63720135974049,4.9554966407503));
#16981=CARTESIAN_POINT('Ctrl Pts',(-3.37243277255298,2.48483414437987,4.94438285169351));
#16982=CARTESIAN_POINT('Ctrl Pts',(-3.40530626273826,2.25481727477052,4.9332690626367));
#16983=CARTESIAN_POINT('Ctrl Pts',(-3.61638513853951,2.15768779995451,4.9221552735799));
#16984=CARTESIAN_POINT('Ctrl Pts',(-3.81246651125382,2.28234942989398,4.91104148452309));
#16985=CARTESIAN_POINT('Ctrl Pts',(-3.81407487666422,2.51469796087643,4.89992769546629));
#16986=CARTESIAN_POINT('Ctrl Pts',(-3.6197380796992,2.64206214751696,4.88881390640948));
#16987=CARTESIAN_POINT('Ctrl Pts',(-3.40733479453568,2.54786410535795,4.87770011735268));
#16988=CARTESIAN_POINT('Ctrl Pts',(-3.37128015690807,2.3183243706747,4.86658632829587));
#16989=CARTESIAN_POINT('Ctrl Pts',(-3.54457538552076,2.16354326577609,4.85547253923908));
#16990=CARTESIAN_POINT('Ctrl Pts',(-3.76860139232476,2.2251936913151,4.84435875018226));
#16991=CARTESIAN_POINT('Ctrl Pts',(-3.83830463266378,2.44684631363142,4.83324496112547));
#16992=CARTESIAN_POINT('Ctrl Pts',(-3.68988494016744,2.62561997380774,4.82213117206865));
#16993=CARTESIAN_POINT('Ctrl Pts',(-3.45919254257122,2.59788111325323,4.81101738301186));
#16994=CARTESIAN_POINT('Ctrl Pts',(-3.35738280762477,2.38901942561361,4.79990359395505));
#16995=CARTESIAN_POINT('Ctrl Pts',(-3.47764334032546,2.19020838223802,4.78878980489825));
#16996=CARTESIAN_POINT('Ctrl Pts',(-3.70989831124516,2.18342198579874,4.77767601584144));
#16997=CARTESIAN_POINT('Ctrl Pts',(-3.84156211155055,2.3748719019196,4.76656222678464));
#16998=CARTESIAN_POINT('Ctrl Pts',(-3.75212137165305,2.58932185118547,4.75544843772783));
#16999=CARTESIAN_POINT('Ctrl Pts',(-3.52344221510783,2.63048336300545,4.74433464867103));
#17000=CARTESIAN_POINT('Ctrl Pts',(-3.36483726729874,2.46068083880743,4.73322085961422));
#17001=CARTESIAN_POINT('Ctrl Pts',(-3.42147943565789,2.23533645468145,4.72210707055742));
#17002=CARTESIAN_POINT('Ctrl Pts',(-3.64152350112028,2.16071048099716,4.71099328150062));
#17003=CARTESIAN_POINT('Ctrl Pts',(-3.82356063509873,2.30510891778388,4.69987949244381));
#17004=CARTESIAN_POINT('Ctrl Pts',(-3.80097018442129,2.53636223826109,4.68876570338701));
#17005=CARTESIAN_POINT('Ctrl Pts',(-3.59442944478611,2.64280165560495,4.6776519143302));
#17006=CARTESIAN_POINT('Ctrl Pts',(-3.39298749751263,2.52700196401557,4.6665381252734));
#17007=CARTESIAN_POINT('Ctrl Pts',(-3.38102644144724,2.29495593446246,4.65542433621659));
#17008=CARTESIAN_POINT('Ctrl Pts',(-3.56949436685434,2.15905792937668,4.64431054715979));
#17009=CARTESIAN_POINT('Ctrl Pts',(-3.7858844442369,2.24369693400118,4.63319675810299));
#17010=CARTESIAN_POINT('Ctrl Pts',(-3.83213238173679,2.47140190753206,4.62208296904618));
#17011=CARTESIAN_POINT('Ctrl Pts',(-3.66590691767206,2.63375190534549,4.61096917998937));
#17012=CARTESIAN_POINT('Ctrl Pts',(-3.43935610442817,2.58214613327058,4.59985539093257));
#17013=CARTESIAN_POINT('Ctrl Pts',(-3.35984447062414,2.36381993973287,4.58874160187577));
#17014=CARTESIAN_POINT('Ctrl Pts',(-3.50014991641224,2.17860976567263,4.57762781281897));
#17015=CARTESIAN_POINT('Ctrl Pts',(-3.73184927607424,2.1960405838179,4.56651402376216));
#17016=CARTESIAN_POINT('Ctrl Pts',(-3.84286549809491,2.40015776867247,4.55540023470536));
#17017=CARTESIAN_POINT('Ctrl Pts',(-3.73158417538336,2.60413054603043,4.54428644564855));
#17018=CARTESIAN_POINT('Ctrl Pts',(-3.49986236476522,2.62126031969194,4.53317265659175));
#17019=CARTESIAN_POINT('Ctrl Pts',(-3.35979766713961,2.43586801331045,4.52205886753494));
#17020=CARTESIAN_POINT('Ctrl Pts',(-3.43959288921302,2.2176453079079,4.51094507847814));
#17021=CARTESIAN_POINT('Ctrl Pts',(-3.66621055822496,2.16633391955349,4.49983128942134));
#17022=CARTESIAN_POINT('Ctrl Pts',(-3.83222495382674,2.32889974592014,4.48871750036453));
#17023=CARTESIAN_POINT('Ctrl Pts',(-3.78568121275365,2.55654443850517,4.47760371130773));
#17024=CARTESIAN_POINT('Ctrl Pts',(-3.56918135753979,2.64090223654315,4.46648992225092));
#17025=CARTESIAN_POINT('Ctrl Pts',(-3.38089014394226,2.50475947474088,4.45537613319412));
#17026=CARTESIAN_POINT('Ctrl Pts',(-3.3931526891646,2.27272919910994,4.44426234413731));
#17027=CARTESIAN_POINT('Ctrl Pts',(-3.59474487835949,2.15719128792351,4.43314855508051));
#17028=CARTESIAN_POINT('Ctrl Pts',(-3.80114723098,2.26389903055612,4.4220347660237));
#17029=CARTESIAN_POINT('Ctrl Pts',(-3.82343705972838,2.49518136177793,4.4109209769669));
#17030=CARTESIAN_POINT('Ctrl Pts',(-3.64121277856108,2.63934345799643,4.3998071879101));
#17031=CARTESIAN_POINT('Ctrl Pts',(-3.4212652433475,2.56443108225311,4.38869339885329));
#17032=CARTESIAN_POINT('Ctrl Pts',(-3.36491712045917,2.33901445477475,4.3775796097965));
#17033=CARTESIAN_POINT('Ctrl Pts',(-3.52374009472539,2.16941582002738,4.36646582073968));
#17034=CARTESIAN_POINT('Ctrl Pts',(-3.75237048890211,2.21087904346051,4.35535203168288));
#17035=CARTESIAN_POINT('Ctrl Pts',(-3.84152270551859,2.42543572391857,4.34423824262608));
#17036=CARTESIAN_POINT('Ctrl Pts',(-3.70962996035205,2.61673302206395,4.33312445356927));
#17037=CARTESIAN_POINT('Ctrl Pts',(-3.47734458963256,2.60960762555316,4.32201066451247));
#17038=CARTESIAN_POINT('Ctrl Pts',(-3.35742145615876,2.41071512444121,4.31089687545567));
#17039=CARTESIAN_POINT('Ctrl Pts',(-3.45934316515028,2.20183612882053,4.29978308639885));
#17040=CARTESIAN_POINT('Ctrl Pts',(-3.69040350703126,2.17470170179864,4.28866929734206));
#17041=CARTESIAN_POINT('Ctrl Pts',(-3.7885754343637,2.29356865430552,4.28126010463752));
#17042=CARTESIAN_POINT('Ctrl Pts',(-3.80166758614466,2.36062792457102,4.27755550828525));
#17043=CARTESIAN_POINT('Ctrl Pts',(-3.64967348970877,2.21400211999972,5.20748149723825));
#17044=CARTESIAN_POINT('Ctrl Pts',(-3.71152220988337,2.2305197371096,5.20377690088598));
#17045=CARTESIAN_POINT('Ctrl Pts',(-3.81636896167925,2.32987270138258,5.19636770818145));
#17046=CARTESIAN_POINT('Ctrl Pts',(-3.7762589230805,2.54412670398045,5.18525391912464));
#17047=CARTESIAN_POINT('Ctrl Pts',(-3.57450297532427,2.62606859592404,5.17414013006784));
#17048=CARTESIAN_POINT('Ctrl Pts',(-3.39623976792153,2.50127640086039,5.16302634101103));
#17049=CARTESIAN_POINT('Ctrl Pts',(-3.404403315861,2.28369088559113,5.15191255195423));
#17050=CARTESIAN_POINT('Ctrl Pts',(-3.59163732076848,2.17261126982347,5.14079876289742));
#17051=CARTESIAN_POINT('Ctrl Pts',(-3.78650650684933,2.26963974340016,5.12968497384063));
#17052=CARTESIAN_POINT('Ctrl Pts',(-3.8106737979302,2.48600012163341,5.11857118478381));
#17053=CARTESIAN_POINT('Ctrl Pts',(-3.64200416517759,2.62363777825967,5.10745739572702));
#17054=CARTESIAN_POINT('Ctrl Pts',(-3.43489004460608,2.55658015434777,5.0963436066702));
#17055=CARTESIAN_POINT('Ctrl Pts',(-3.37890173959752,2.34620148403342,5.0852298176134));
#17056=CARTESIAN_POINT('Ctrl Pts',(-3.52528777861237,2.18506593235721,5.0741160285566));
#17057=CARTESIAN_POINT('Ctrl Pts',(-3.74005846207577,2.22066160730187,5.06300223949979));
#17058=CARTESIAN_POINT('Ctrl Pts',(-3.82663219619914,2.42040792821545,5.05188845044299));
#17059=CARTESIAN_POINT('Ctrl Pts',(-3.70576683635895,2.60147455044772,5.04077466138619));
#17060=CARTESIAN_POINT('Ctrl Pts',(-3.4880919289783,2.59812927699836,5.02966087232938));
#17061=CARTESIAN_POINT('Ctrl Pts',(-3.37284772952088,2.41343400678959,5.01854708327258));
#17062=CARTESIAN_POINT('Ctrl Pts',(-3.46551858860765,2.21644244909332,5.00743329421577));
#17063=CARTESIAN_POINT('Ctrl Pts',(-3.68128180402377,2.18746319379313,4.99631950515897));
#17064=CARTESIAN_POINT('Ctrl Pts',(-3.82264686473641,2.35302129035867,4.98520571610216));
#17065=CARTESIAN_POINT('Ctrl Pts',(-3.76022072401106,2.56157953122871,4.97409192704537));
#17066=CARTESIAN_POINT('Ctrl Pts',(-3.55114273814991,2.6222421954303,4.96297813798855));
#17067=CARTESIAN_POINT('Ctrl Pts',(-3.38678435785046,2.47948405740616,4.95186434893176));
#17068=CARTESIAN_POINT('Ctrl Pts',(-3.41758467298453,2.26397326040267,4.94075055987495));
#17069=CARTESIAN_POINT('Ctrl Pts',(-3.61535180559434,2.17296928071335,4.92963677081814));
#17070=CARTESIAN_POINT('Ctrl Pts',(-3.79906725647832,2.28976909313423,4.91852298176134));
#17071=CARTESIAN_POINT('Ctrl Pts',(-3.80057418991348,2.50746450469106,4.90740919270453));
#17072=CARTESIAN_POINT('Ctrl Pts',(-3.61849329266379,2.62679643638467,4.89629540364773));
#17073=CARTESIAN_POINT('Ctrl Pts',(-3.41948527490624,2.53853901780343,4.88518161459093));
#17074=CARTESIAN_POINT('Ctrl Pts',(-3.38570443220547,2.32347526509011,4.87406782553412));
#17075=CARTESIAN_POINT('Ctrl Pts',(-3.54807075298295,2.17845547008797,4.86295403647732));
#17076=CARTESIAN_POINT('Ctrl Pts',(-3.7579685024734,2.23621789580084,4.85184024742051));
#17077=CARTESIAN_POINT('Ctrl Pts',(-3.82327589016501,2.44389193890226,4.84072645836371));
#17078=CARTESIAN_POINT('Ctrl Pts',(-3.6842163234679,2.61139119255816,4.8296126693069));
#17079=CARTESIAN_POINT('Ctrl Pts',(-3.4680726008225,2.58540169032632,4.8184988802501));
#17080=CARTESIAN_POINT('Ctrl Pts',(-3.37268352280275,2.38971191834066,4.8073850911933));
#17081=CARTESIAN_POINT('Ctrl Pts',(-3.48535979430583,2.20343894417256,4.79627130213649));
#17082=CARTESIAN_POINT('Ctrl Pts',(-3.70296754618914,2.19708053355731,4.78515751307969));
#17083=CARTESIAN_POINT('Ctrl Pts',(-3.82632793531414,2.37645661184032,4.77404372402288));
#17084=CARTESIAN_POINT('Ctrl Pts',(-3.74252779851275,2.57738222030606,4.76292993496608));
#17085=CARTESIAN_POINT('Ctrl Pts',(-3.52827035135747,2.61594787087447,4.75181614590928));
#17086=CARTESIAN_POINT('Ctrl Pts',(-3.37966786507423,2.45685398621605,4.74070235685247));
#17087=CARTESIAN_POINT('Ctrl Pts',(-3.43273788062492,2.24572100320602,4.72958856779567));
#17088=CARTESIAN_POINT('Ctrl Pts',(-3.63890481092106,2.17580133560435,4.71847477873887));
#17089=CARTESIAN_POINT('Ctrl Pts',(-3.80946172657059,2.31109324810979,4.70736098968206));
#17090=CARTESIAN_POINT('Ctrl Pts',(-3.78829594843252,2.5277625188915,4.69624720062526));
#17091=CARTESIAN_POINT('Ctrl Pts',(-3.59478075327286,2.62748930720629,4.68513341156845));
#17092=CARTESIAN_POINT('Ctrl Pts',(-3.40604279383286,2.51899255273097,4.67401962251165));
#17093=CARTESIAN_POINT('Ctrl Pts',(-3.39483606482192,2.30158056527362,4.66290583345485));
#17094=CARTESIAN_POINT('Ctrl Pts',(-3.57141821239684,2.17425300257371,4.65179204439804));
#17095=CARTESIAN_POINT('Ctrl Pts',(-3.77416159430429,2.253554226763,4.64067825534124));
#17096=CARTESIAN_POINT('Ctrl Pts',(-3.81749289381852,2.46689892800445,4.62956446628442));
#17097=CARTESIAN_POINT('Ctrl Pts',(-3.66175048108285,2.61901028175737,4.61845067722763));
#17098=CARTESIAN_POINT('Ctrl Pts',(-3.44948715271524,2.57065904087346,4.60733688817082));
#17099=CARTESIAN_POINT('Ctrl Pts',(-3.37498994039659,2.36610164447049,4.59622309911403));
#17100=CARTESIAN_POINT('Ctrl Pts',(-3.50644698742571,2.19257179732202,4.58510931005721));
#17101=CARTESIAN_POINT('Ctrl Pts',(-3.72353416781713,2.20890333647083,4.57399552100042));
#17102=CARTESIAN_POINT('Ctrl Pts',(-3.82754912345333,2.40014781895086,4.5628817319436));
#17103=CARTESIAN_POINT('Ctrl Pts',(-3.723285785769,2.59125700102993,4.55176794288681));
#17104=CARTESIAN_POINT('Ctrl Pts',(-3.50617757029671,2.60730648114219,4.54065415382999));
#17105=CARTESIAN_POINT('Ctrl Pts',(-3.37494608858577,2.43360598789383,4.52954036477319));
#17106=CARTESIAN_POINT('Ctrl Pts',(-3.44970900460718,2.22914555312034,4.51842657571639));
#17107=CARTESIAN_POINT('Ctrl Pts',(-3.66203497246676,2.18107013057245,4.50731278665959));
#17108=CARTESIAN_POINT('Ctrl Pts',(-3.81757962782599,2.33338370159577,4.49619899760278));
#17109=CARTESIAN_POINT('Ctrl Pts',(-3.77397117966642,2.54667192352462,4.48508520854598));
#17110=CARTESIAN_POINT('Ctrl Pts',(-3.57112494309463,2.62570967549255,4.47397141948917));
#17111=CARTESIAN_POINT('Ctrl Pts',(-3.3947083629539,2.49815279172096,4.46285763043237));
#17112=CARTESIAN_POINT('Ctrl Pts',(-3.40619756763113,2.28075556466066,4.45174384137556));
#17113=CARTESIAN_POINT('Ctrl Pts',(-3.59507629394739,2.17250408134035,4.44063005231876));
#17114=CARTESIAN_POINT('Ctrl Pts',(-3.78846182950481,2.27248227294105,4.42951626326195));
#17115=CARTESIAN_POINT('Ctrl Pts',(-3.80934594451251,2.48917872489734,4.41840247420516));
#17116=CARTESIAN_POINT('Ctrl Pts',(-3.63861368415939,2.62424920171285,4.40728868514834));
#17117=CARTESIAN_POINT('Ctrl Pts',(-3.43253719640727,2.55406119407111,4.39617489609155));
#17118=CARTESIAN_POINT('Ctrl Pts',(-3.37974268227471,2.34286052375416,4.38506110703474));
#17119=CARTESIAN_POINT('Ctrl Pts',(-3.5285494451209,2.18395767020613,4.37394731797793));
#17120=CARTESIAN_POINT('Ctrl Pts',(-3.74276120511889,2.22280600486777,4.36283352892113));
#17121=CARTESIAN_POINT('Ctrl Pts',(-3.82629101443365,2.42383161349583,4.35171973986432));
#17122=CARTESIAN_POINT('Ctrl Pts',(-3.70271611891361,2.60306469869495,4.34060595080752));
#17123=CARTESIAN_POINT('Ctrl Pts',(-3.48507988440164,2.59638866713425,4.32949216175072));
#17124=CARTESIAN_POINT('Ctrl Pts',(-3.37271973395708,2.41003937238272,4.31837837269391));
#17125=CARTESIAN_POINT('Ctrl Pts',(-3.46821372435015,2.21433338394825,4.30726458363711));
#17126=CARTESIAN_POINT('Ctrl Pts',(-3.68470218678007,2.18891019649399,4.2961507945803));
#17127=CARTESIAN_POINT('Ctrl Pts',(-3.77668287645173,2.30028077429396,4.28874160187577));
#17128=CARTESIAN_POINT('Ctrl Pts',(-3.78894936833816,2.36311093455975,4.2850370055235));
#17129=CARTESIAN_POINT('Ctrl Pts',(-3.64632995769868,2.22652167256662,5.2149629944765));
#17130=CARTESIAN_POINT('Ctrl Pts',(-3.70401562879218,2.24192748573719,5.21125839812423));
#17131=CARTESIAN_POINT('Ctrl Pts',(-3.80180512584637,2.33459298314823,5.2038492054197));
#17132=CARTESIAN_POINT('Ctrl Pts',(-3.76439490155032,2.53442550820997,5.19273541636289));
#17133=CARTESIAN_POINT('Ctrl Pts',(-3.57621918488928,2.61085187587115,5.18162162730609));
#17134=CARTESIAN_POINT('Ctrl Pts',(-3.40995490777444,2.49445946711708,5.17050783824928));
#17135=CARTESIAN_POINT('Ctrl Pts',(-3.41756896575436,2.2915196741335,5.15939404919248));
#17136=CARTESIAN_POINT('Ctrl Pts',(-3.59220021429306,2.18791684836318,5.14828026013568));
#17137=CARTESIAN_POINT('Ctrl Pts',(-3.7739527185128,2.27841431698741,5.13716647107887));
#17138=CARTESIAN_POINT('Ctrl Pts',(-3.79649330464903,2.48021143714115,5.12605268202206));
#17139=CARTESIAN_POINT('Ctrl Pts',(-3.63917685685576,2.60858467700464,5.11493889296527));
#17140=CARTESIAN_POINT('Ctrl Pts',(-3.44600362700749,2.54604071447196,5.10382510390845));
#17141=CARTESIAN_POINT('Ctrl Pts',(-3.39378390542411,2.349822672343,5.09271131485166));
#17142=CARTESIAN_POINT('Ctrl Pts',(-3.53031667239896,2.19953318520045,5.08159752579485));
#17143=CARTESIAN_POINT('Ctrl Pts',(-3.73063110043921,2.23273290851586,5.07048373673805));
#17144=CARTESIAN_POINT('Ctrl Pts',(-3.81137754010487,2.41903426669804,5.05936994768123));
#17145=CARTESIAN_POINT('Ctrl Pts',(-3.69864765055087,2.58791326025872,5.04825615862444));
#17146=CARTESIAN_POINT('Ctrl Pts',(-3.49562448245587,2.58479315779948,5.03714236956762));
#17147=CARTESIAN_POINT('Ctrl Pts',(-3.38813739191354,2.41252976124558,5.02602858051083));
#17148=CARTESIAN_POINT('Ctrl Pts',(-3.47457055790533,2.22879774264625,5.01491479145402));
#17149=CARTESIAN_POINT('Ctrl Pts',(-3.67581071038439,2.20176908651461,5.00380100239723));
#17150=CARTESIAN_POINT('Ctrl Pts',(-3.8076604620585,2.35618343621151,4.99268721334041));
#17151=CARTESIAN_POINT('Ctrl Pts',(-3.74943623670099,2.5507035823472,4.98157342428361));
#17152=CARTESIAN_POINT('Ctrl Pts',(-3.55443132970808,2.6072830311201,4.97045963522681));
#17153=CARTESIAN_POINT('Ctrl Pts',(-3.40113594314794,2.47413397043246,4.95934584617));
#17154=CARTESIAN_POINT('Ctrl Pts',(-3.42986308323079,2.27312924603482,4.9482320571132));
#17155=CARTESIAN_POINT('Ctrl Pts',(-3.61431847264918,2.18825076147219,4.93711826805639));
#17156=CARTESIAN_POINT('Ctrl Pts',(-3.78566800170281,2.29718875637448,4.92600447899959));
#17157=CARTESIAN_POINT('Ctrl Pts',(-3.78707350316275,2.50023104850568,4.91489068994278));
#17158=CARTESIAN_POINT('Ctrl Pts',(-3.61724850562837,2.61153072525238,4.90377690088598));
#17159=CARTESIAN_POINT('Ctrl Pts',(-3.43163575527681,2.52921393024892,4.89266311182917));
#17160=CARTESIAN_POINT('Ctrl Pts',(-3.40012870750287,2.32862615950552,4.88154932277238));
#17161=CARTESIAN_POINT('Ctrl Pts',(-3.55156612044514,2.19336767439986,4.87043553371556));
#17162=CARTESIAN_POINT('Ctrl Pts',(-3.74733561262204,2.24724210028659,4.85932174465877));
#17163=CARTESIAN_POINT('Ctrl Pts',(-3.80824714766624,2.4409375641731,4.84820795560196));
#17164=CARTESIAN_POINT('Ctrl Pts',(-3.67854770676838,2.59716241130857,4.83709416654516));
#17165=CARTESIAN_POINT('Ctrl Pts',(-3.47695265907377,2.57292226739941,4.82598037748835));
#17166=CARTESIAN_POINT('Ctrl Pts',(-3.38798423798073,2.39040441106771,4.81486658843155));
#17167=CARTESIAN_POINT('Ctrl Pts',(-3.49307624828619,2.2166695061071,4.80375279937474));
#17168=CARTESIAN_POINT('Ctrl Pts',(-3.69603678113312,2.21073908131588,4.79263901031794));
#17169=CARTESIAN_POINT('Ctrl Pts',(-3.81109375907773,2.37804132176103,4.78152522126113));
#17170=CARTESIAN_POINT('Ctrl Pts',(-3.73293422537244,2.56544258942666,4.77041143220433));
#17171=CARTESIAN_POINT('Ctrl Pts',(-3.5330984876071,2.6014123787435,4.75929764314753));
#17172=CARTESIAN_POINT('Ctrl Pts',(-3.39449846284973,2.45302713362467,4.74818385409072));
#17173=CARTESIAN_POINT('Ctrl Pts',(-3.44399632559195,2.2561055517306,4.73707006503392));
#17174=CARTESIAN_POINT('Ctrl Pts',(-3.63628612072185,2.19089219021153,4.72595627597712));
#17175=CARTESIAN_POINT('Ctrl Pts',(-3.79536281804244,2.31707757843571,4.7148424869203));
#17176=CARTESIAN_POINT('Ctrl Pts',(-3.77562171244375,2.5191627995219,4.70372869786351));
#17177=CARTESIAN_POINT('Ctrl Pts',(-3.5951320617596,2.61217695880763,4.6926149088067));
#17178=CARTESIAN_POINT('Ctrl Pts',(-3.41909809015308,2.51098314144638,4.6815011197499));
#17179=CARTESIAN_POINT('Ctrl Pts',(-3.40864568819661,2.30820519608479,4.67038733069309));
#17180=CARTESIAN_POINT('Ctrl Pts',(-3.57334205793934,2.18944807577074,4.65927354163629));
#17181=CARTESIAN_POINT('Ctrl Pts',(-3.76243874437168,2.26341151952482,4.64815975257949));
#17182=CARTESIAN_POINT('Ctrl Pts',(-3.80285340590026,2.46239594847684,4.63704596352267));
#17183=CARTESIAN_POINT('Ctrl Pts',(-3.65759404449364,2.60426865816925,4.62593217446588));
#17184=CARTESIAN_POINT('Ctrl Pts',(-3.45961820100231,2.55917194847634,4.61481838540907));
#17185=CARTESIAN_POINT('Ctrl Pts',(-3.39013541016905,2.3683833492081,4.60370459635227));
#17186=CARTESIAN_POINT('Ctrl Pts',(-3.51274405843916,2.20653382897141,4.59259080729546));
#17187=CARTESIAN_POINT('Ctrl Pts',(-3.71521905956003,2.22176608912375,4.58147701823867));
#17188=CARTESIAN_POINT('Ctrl Pts',(-3.81223274881174,2.40013786922925,4.57036322918185));
#17189=CARTESIAN_POINT('Ctrl Pts',(-3.71498739615465,2.57838345602943,4.55924944012506));
#17190=CARTESIAN_POINT('Ctrl Pts',(-3.51249277582821,2.59335264259245,4.54813565106824));
#17191=CARTESIAN_POINT('Ctrl Pts',(-3.39009451003192,2.4313439624772,4.53702186201144));
#17192=CARTESIAN_POINT('Ctrl Pts',(-3.45982512000134,2.24064579833279,4.52590807295464));
#17193=CARTESIAN_POINT('Ctrl Pts',(-3.65785938670857,2.1958063415914,4.51479428389783));
#17194=CARTESIAN_POINT('Ctrl Pts',(-3.80293430182523,2.33786765727141,4.50368049484103));
#17195=CARTESIAN_POINT('Ctrl Pts',(-3.76226114657918,2.53679940854407,4.49256670578423));
#17196=CARTESIAN_POINT('Ctrl Pts',(-3.57306852864947,2.61051711444195,4.48145291672742));
#17197=CARTESIAN_POINT('Ctrl Pts',(-3.40852658196552,2.49154610870105,4.47033912767061));
#17198=CARTESIAN_POINT('Ctrl Pts',(-3.41924244609765,2.28878193021138,4.45922533861382));
#17199=CARTESIAN_POINT('Ctrl Pts',(-3.5954077095353,2.18781687475719,4.44811154955701));
#17200=CARTESIAN_POINT('Ctrl Pts',(-3.77577642802961,2.28106551532598,4.43699776050021));
#17201=CARTESIAN_POINT('Ctrl Pts',(-3.79525482929664,2.48317608801675,4.4258839714434));
#17202=CARTESIAN_POINT('Ctrl Pts',(-3.6360145897577,2.60915494542926,4.4147701823866));
#17203=CARTESIAN_POINT('Ctrl Pts',(-3.44380914946703,2.54369130588911,4.40365639332979));
#17204=CARTESIAN_POINT('Ctrl Pts',(-3.39456824409026,2.34670659273357,4.39254260427299));
#17205=CARTESIAN_POINT('Ctrl Pts',(-3.53335879551641,2.19849952038487,4.38142881521618));
#17206=CARTESIAN_POINT('Ctrl Pts',(-3.73315192133567,2.23473296627504,4.37031502615938));
#17207=CARTESIAN_POINT('Ctrl Pts',(-3.81105932334871,2.4222275030731,4.35920123710257));
#17208=CARTESIAN_POINT('Ctrl Pts',(-3.69580227747518,2.58939637532595,4.34808744804577));
#17209=CARTESIAN_POINT('Ctrl Pts',(-3.49281517917073,2.58316970871533,4.33697365898897));
#17210=CARTESIAN_POINT('Ctrl Pts',(-3.38801801175539,2.40936362032424,4.32585986993216));
#17211=CARTESIAN_POINT('Ctrl Pts',(-3.47708428355003,2.22683063907596,4.31474608087536));
#17212=CARTESIAN_POINT('Ctrl Pts',(-3.67900086652888,2.20311869118934,4.30363229181856));
#17213=CARTESIAN_POINT('Ctrl Pts',(-3.76479031853975,2.3069928942824,4.29622309911402));
#17214=CARTESIAN_POINT('Ctrl Pts',(-3.77623115053166,2.36559394454847,4.29251850276175));
#17215=CARTESIAN_POINT('Ctrl Pts',(-3.64298642568859,2.23904122513352,5.22244449171475));
#17216=CARTESIAN_POINT('Ctrl Pts',(-3.69650904770099,2.25333523436478,5.21873989536248));
#17217=CARTESIAN_POINT('Ctrl Pts',(-3.78724129001348,2.33931326491388,5.21133070265794));
#17218=CARTESIAN_POINT('Ctrl Pts',(-3.75253088002014,2.52472431243949,5.20021691360114));
#17219=CARTESIAN_POINT('Ctrl Pts',(-3.57793539445428,2.59563515581826,5.18910312454433));
#17220=CARTESIAN_POINT('Ctrl Pts',(-3.42367004762736,2.48764253337377,5.17798933548753));
#17221=CARTESIAN_POINT('Ctrl Pts',(-3.4307346156477,2.29934846267587,5.16687554643072));
#17222=CARTESIAN_POINT('Ctrl Pts',(-3.59276310781765,2.2032224269029,5.15576175737392));
#17223=CARTESIAN_POINT('Ctrl Pts',(-3.76139893017626,2.28718889057467,5.14464796831712));
#17224=CARTESIAN_POINT('Ctrl Pts',(-3.78231281136787,2.47442275264891,5.13353417926031));
#17225=CARTESIAN_POINT('Ctrl Pts',(-3.63634954853391,2.5935315757496,5.12242039020352));
#17226=CARTESIAN_POINT('Ctrl Pts',(-3.45711720940891,2.53550127459616,5.1113066011467));
#17227=CARTESIAN_POINT('Ctrl Pts',(-3.4086660712507,2.35344386065259,5.1001928120899));
#17228=CARTESIAN_POINT('Ctrl Pts',(-3.53534556618555,2.21400043804369,5.0890790230331));
#17229=CARTESIAN_POINT('Ctrl Pts',(-3.72120373880265,2.24480420972985,5.07796523397629));
#17230=CARTESIAN_POINT('Ctrl Pts',(-3.79612288401061,2.41766060518064,5.06685144491949));
#17231=CARTESIAN_POINT('Ctrl Pts',(-3.6915284647428,2.57435197006973,5.05573765586269));
#17232=CARTESIAN_POINT('Ctrl Pts',(-3.50315703593343,2.5714570386006,5.04462386680588));
#17233=CARTESIAN_POINT('Ctrl Pts',(-3.40342705430619,2.41162551570156,5.03351007774908));
#17234=CARTESIAN_POINT('Ctrl Pts',(-3.48362252720301,2.24115303619919,5.02239628869227));
#17235=CARTESIAN_POINT('Ctrl Pts',(-3.67033961674501,2.21607497923609,5.01128249963547));
#17236=CARTESIAN_POINT('Ctrl Pts',(-3.79267405938058,2.35934558206435,5.00016871057866));
#17237=CARTESIAN_POINT('Ctrl Pts',(-3.73865174939092,2.53982763346569,4.98905492152186));
#17238=CARTESIAN_POINT('Ctrl Pts',(-3.55771992126626,2.59232386680991,4.97794113246505));
#17239=CARTESIAN_POINT('Ctrl Pts',(-3.41548752844543,2.46878388345875,4.96682734340825));
#17240=CARTESIAN_POINT('Ctrl Pts',(-3.44214149347704,2.28228523166696,4.95571355435145));
#17241=CARTESIAN_POINT('Ctrl Pts',(-3.61328513970402,2.20353224223104,4.94459976529464));
#17242=CARTESIAN_POINT('Ctrl Pts',(-3.7722687469273,2.30460841961473,4.93348597623784));
#17243=CARTESIAN_POINT('Ctrl Pts',(-3.77357281641202,2.4929975923203,4.92237218718104));
#17244=CARTESIAN_POINT('Ctrl Pts',(-3.61600371859295,2.59626501412009,4.91125839812423));
#17245=CARTESIAN_POINT('Ctrl Pts',(-3.44378623564737,2.51988884269441,4.90014460906743));
#17246=CARTESIAN_POINT('Ctrl Pts',(-3.41455298280027,2.33377705392094,4.88903082001062));
#17247=CARTESIAN_POINT('Ctrl Pts',(-3.55506148790733,2.20827987871175,4.87791703095382));
#17248=CARTESIAN_POINT('Ctrl Pts',(-3.73670272277068,2.25826630477233,4.86680324189701));
#17249=CARTESIAN_POINT('Ctrl Pts',(-3.79321840516747,2.43798318944394,4.85568945284021));
#17250=CARTESIAN_POINT('Ctrl Pts',(-3.67287909006884,2.58293363005899,4.8445756637834));
#17251=CARTESIAN_POINT('Ctrl Pts',(-3.48583271732505,2.5604428444725,4.8334618747266));
#17252=CARTESIAN_POINT('Ctrl Pts',(-3.40328495315871,2.39109690379476,4.8223480856698));
#17253=CARTESIAN_POINT('Ctrl Pts',(-3.50079270226656,2.22990006804163,4.81123429661299));
#17254=CARTESIAN_POINT('Ctrl Pts',(-3.68910601607711,2.22439762907444,4.80012050755619));
#17255=CARTESIAN_POINT('Ctrl Pts',(-3.79585958284132,2.37962603168174,4.78900671849938));
#17256=CARTESIAN_POINT('Ctrl Pts',(-3.72334065223214,2.55350295854726,4.77789292944258));
#17257=CARTESIAN_POINT('Ctrl Pts',(-3.53792662385674,2.58687688661252,4.76677914038578));
#17258=CARTESIAN_POINT('Ctrl Pts',(-3.40932906062523,2.4492002810333,4.75566535132897));
#17259=CARTESIAN_POINT('Ctrl Pts',(-3.45525477055898,2.26649010025516,4.74455156227217));
#17260=CARTESIAN_POINT('Ctrl Pts',(-3.63366743052263,2.20598304481872,4.73343777321536));
#17261=CARTESIAN_POINT('Ctrl Pts',(-3.7812639095143,2.32306190876162,4.72232398415856));
#17262=CARTESIAN_POINT('Ctrl Pts',(-3.76294747645498,2.51056308015232,4.71121019510176));
#17263=CARTESIAN_POINT('Ctrl Pts',(-3.59548337024634,2.59686461040897,4.70009640604495));
#17264=CARTESIAN_POINT('Ctrl Pts',(-3.43215338647331,2.50297373016179,4.68898261698815));
#17265=CARTESIAN_POINT('Ctrl Pts',(-3.42245531157129,2.31482982689595,4.67786882793134));
#17266=CARTESIAN_POINT('Ctrl Pts',(-3.57526590348185,2.20464314896778,4.66675503887454));
#17267=CARTESIAN_POINT('Ctrl Pts',(-3.75071589443907,2.27326881228664,4.65564124981773));
#17268=CARTESIAN_POINT('Ctrl Pts',(-3.78821391798199,2.45789296894922,4.64452746076093));
#17269=CARTESIAN_POINT('Ctrl Pts',(-3.65343760790444,2.58952703458114,4.63341367170412));
#17270=CARTESIAN_POINT('Ctrl Pts',(-3.46974924928937,2.54768485607922,4.62229988264733));
#17271=CARTESIAN_POINT('Ctrl Pts',(-3.40528087994151,2.37066505394572,4.61118609359051));
#17272=CARTESIAN_POINT('Ctrl Pts',(-3.51904112945263,2.2204958606208,4.60007230453372));
#17273=CARTESIAN_POINT('Ctrl Pts',(-3.70690395130293,2.23462884177668,4.58895851547691));
#17274=CARTESIAN_POINT('Ctrl Pts',(-3.79691637417015,2.40012791950764,4.57784472642011));
#17275=CARTESIAN_POINT('Ctrl Pts',(-3.7066890065403,2.56550991102893,4.5667309373633));
#17276=CARTESIAN_POINT('Ctrl Pts',(-3.5188079813597,2.57939880404271,4.55561714830649));
#17277=CARTESIAN_POINT('Ctrl Pts',(-3.40524293147808,2.42908193706057,4.54450335924969));
#17278=CARTESIAN_POINT('Ctrl Pts',(-3.4699412353955,2.25214604354523,4.53338957019289));
#17279=CARTESIAN_POINT('Ctrl Pts',(-3.65368380095038,2.21054255261035,4.52227578113608));
#17280=CARTESIAN_POINT('Ctrl Pts',(-3.78828897582448,2.34235161294705,4.51116199207928));
#17281=CARTESIAN_POINT('Ctrl Pts',(-3.75055111349195,2.52692689356351,4.50004820302248));
#17282=CARTESIAN_POINT('Ctrl Pts',(-3.57501211420431,2.59532455339135,4.48893441396567));
#17283=CARTESIAN_POINT('Ctrl Pts',(-3.42234480097716,2.48493942568113,4.47782062490887));
#17284=CARTESIAN_POINT('Ctrl Pts',(-3.43228732456417,2.29680829576209,4.46670683585206));
#17285=CARTESIAN_POINT('Ctrl Pts',(-3.5957391251232,2.20312966817403,4.45559304679526));
#17286=CARTESIAN_POINT('Ctrl Pts',(-3.76309102655441,2.2896487577109,4.44447925773845));
#17287=CARTESIAN_POINT('Ctrl Pts',(-3.78116371408077,2.47717345113617,4.43336546868165));
#17288=CARTESIAN_POINT('Ctrl Pts',(-3.63341549535601,2.59406068914566,4.42225167962485));
#17289=CARTESIAN_POINT('Ctrl Pts',(-3.4550811025268,2.53332141770711,4.41113789056804));
#17290=CARTESIAN_POINT('Ctrl Pts',(-3.40939380590581,2.35055266171297,4.40002410151124));
#17291=CARTESIAN_POINT('Ctrl Pts',(-3.53816814591191,2.21304137056363,4.38891031245443));
#17292=CARTESIAN_POINT('Ctrl Pts',(-3.72354263755246,2.2466599276823,4.37779652339763));
#17293=CARTESIAN_POINT('Ctrl Pts',(-3.79582763226376,2.42062339265036,4.36668273434082));
#17294=CARTESIAN_POINT('Ctrl Pts',(-3.68888843603675,2.57572805195694,4.35556894528402));
#17295=CARTESIAN_POINT('Ctrl Pts',(-3.50055047393982,2.56995075029642,4.34445515622722));
#17296=CARTESIAN_POINT('Ctrl Pts',(-3.40331628955371,2.40868786826575,4.33334136717041));
#17297=CARTESIAN_POINT('Ctrl Pts',(-3.4859548427499,2.23932789420368,4.32222757811361));
#17298=CARTESIAN_POINT('Ctrl Pts',(-3.67329954627769,2.21732718588468,4.3111137890568));
#17299=CARTESIAN_POINT('Ctrl Pts',(-3.75289776062778,2.31370501427084,4.30370459635227));
#17300=CARTESIAN_POINT('Ctrl Pts',(-3.76351293272515,2.3680769545372,4.3));
#17301=CARTESIAN_POINT('Ctrl Pts',(-3.76638442018051,2.4000942147675,5.13785196366098));
#17302=CARTESIAN_POINT('Ctrl Pts',(-3.76649613151981,2.42168271873493,5.13641270219409));
#17303=CARTESIAN_POINT('Ctrl Pts',(-3.76259704654914,2.44323253526348,5.1349734407272));
#17304=CARTESIAN_POINT('Ctrl Pts',(-3.75449995403028,2.46306857948665,5.13353417926031));
#17305=CARTESIAN_POINT('Ctrl Pts',(-3.73365839042322,2.51412569368247,5.12982958290804));
#17306=CARTESIAN_POINT('Ctrl Pts',(-3.68500396947857,2.55382863471604,5.12612498655578));
#17307=CARTESIAN_POINT('Ctrl Pts',(-3.63080470248541,2.56400838837391,5.12242039020351));
#17308=CARTESIAN_POINT('Ctrl Pts',(-3.57660543549225,2.57418814203179,5.11871579385124));
#17309=CARTESIAN_POINT('Ctrl Pts',(-3.51686132245058,2.55484470831398,5.11501119749897));
#17310=CARTESIAN_POINT('Ctrl Pts',(-3.47891407623671,2.51483008913114,5.1113066011467));
#17311=CARTESIAN_POINT('Ctrl Pts',(-3.44096683002284,2.47481546994831,5.10760200479444));
#17312=CARTESIAN_POINT('Ctrl Pts',(-3.42481645063677,2.41412966530045,5.10389740844217));
#17313=CARTESIAN_POINT('Ctrl Pts',(-3.43785451009954,2.3605461925417,5.1001928120899));
#17314=CARTESIAN_POINT('Ctrl Pts',(-3.45089256956232,2.30696271978295,5.09648821573763));
#17315=CARTESIAN_POINT('Ctrl Pts',(-3.49311906787393,2.26048157891332,5.09278361938537));
#17316=CARTESIAN_POINT('Ctrl Pts',(-3.54520867913259,2.2423749704262,5.0890790230331));
#17317=CARTESIAN_POINT('Ctrl Pts',(-3.59729829039125,2.22426836193908,5.08537442668083));
#17318=CARTESIAN_POINT('Ctrl Pts',(-3.65925101459695,2.23453628583446,5.08166983032856));
#17319=CARTESIAN_POINT('Ctrl Pts',(-3.70271390090113,2.26847964702395,5.07796523397629));
#17320=CARTESIAN_POINT('Ctrl Pts',(-3.74226404132859,2.29936725748381,5.07459414387119));
#17321=CARTESIAN_POINT('Ctrl Pts',(-3.76650358790754,2.34985942080815,5.07122305376608));
#17322=CARTESIAN_POINT('Ctrl Pts',(-3.76682061973634,2.40008640134019,5.06785196366098));
#17323=CARTESIAN_POINT('Ctrl Pts',(-3.65301702171886,2.20148256743283,5.2));
#17324=CARTESIAN_POINT('Ctrl Pts',(-3.66542047547214,2.20607510650608,5.2));
#17325=CARTESIAN_POINT('Ctrl Pts',(-3.67726977303962,2.21193437262237,5.2));
#17326=CARTESIAN_POINT('Ctrl Pts',(-3.688447163997,2.21889712590693,5.2));
#17327=CARTESIAN_POINT('Ctrl Pts',(-3.69411334108481,2.22242676831449,5.2));
#17328=CARTESIAN_POINT('Ctrl Pts',(-3.69960641439008,2.22624073198774,5.2));
#17329=CARTESIAN_POINT('Ctrl Pts',(-3.70490760860864,2.23032132776193,5.2));
#17330=CARTESIAN_POINT('Ctrl Pts',(-3.70949455661916,2.2338521323121,5.2));
#17331=CARTESIAN_POINT('Ctrl Pts',(-3.71393782222619,2.23758261370384,5.2));
#17332=CARTESIAN_POINT('Ctrl Pts',(-3.71822343533123,2.24150219834368,5.2));
#17333=CARTESIAN_POINT('Ctrl Pts',(-3.72133392659836,2.24434702672511,5.2));
#17334=CARTESIAN_POINT('Ctrl Pts',(-3.72435518261367,2.24728605527231,5.2));
#17335=CARTESIAN_POINT('Ctrl Pts',(-3.72727779974184,2.25030906336475,5.2));
#17336=CARTESIAN_POINT('Ctrl Pts',(-3.73622279642463,2.25956131782473,5.2));
#17337=CARTESIAN_POINT('Ctrl Pts',(-3.74426351405243,2.26961342426582,5.2));
#17338=CARTESIAN_POINT('Ctrl Pts',(-3.75126091239845,2.28033434366482,5.2));
#17339=CARTESIAN_POINT('Ctrl Pts',(-3.75579176664188,2.28727619844431,5.2));
#17340=CARTESIAN_POINT('Ctrl Pts',(-3.75988435832116,2.29449904020269,5.2));
#17341=CARTESIAN_POINT('Ctrl Pts',(-3.76348920729151,2.30196994667654,5.2));
#17342=CARTESIAN_POINT('Ctrl Pts',(-3.76515597383801,2.30542425421759,5.2));
#17343=CARTESIAN_POINT('Ctrl Pts',(-3.76671433719502,2.30892350560647,5.2));
#17344=CARTESIAN_POINT('Ctrl Pts',(-3.76815916520543,2.31246074610162,5.2));
#17345=CARTESIAN_POINT('Ctrl Pts',(-3.77216128940432,2.32225878135629,5.2));
#17346=CARTESIAN_POINT('Ctrl Pts',(-3.77529844536059,2.33235630265294,5.2));
#17347=CARTESIAN_POINT('Ctrl Pts',(-3.77747651815115,2.34267992422407,5.2));
#17348=CARTESIAN_POINT('Ctrl Pts',(-3.77933030902448,2.35146651553144,5.2));
#17349=CARTESIAN_POINT('Ctrl Pts',(-3.78048860368035,2.36041737528633,5.2));
#17350=CARTESIAN_POINT('Ctrl Pts',(-3.78096403138949,2.36945420421056,5.2));
#17351=CARTESIAN_POINT('Ctrl Pts',(-3.781133173515,2.37266922180987,5.2));
#17352=CARTESIAN_POINT('Ctrl Pts',(-3.78121552286205,2.37589368165894,5.2));
#17353=CARTESIAN_POINT('Ctrl Pts',(-3.78121200959806,2.37911434872485,5.2));
#17354=CARTESIAN_POINT('Ctrl Pts',(-3.78119923720175,2.3908230151512,5.2));
#17355=CARTESIAN_POINT('Ctrl Pts',(-3.78005717470715,2.40251790081025,5.2));
#17356=CARTESIAN_POINT('Ctrl Pts',(-3.77783120806398,2.41402669258654,5.2));
#17357=CARTESIAN_POINT('Ctrl Pts',(-3.77668819949671,2.41993632633585,5.2));
#17358=CARTESIAN_POINT('Ctrl Pts',(-3.77525870411221,2.42579670928221,5.2));
#17359=CARTESIAN_POINT('Ctrl Pts',(-3.77354493887783,2.43158224657623,5.2));
#17360=CARTESIAN_POINT('Ctrl Pts',(-3.77185769889076,2.43727823671147,5.2));
#17361=CARTESIAN_POINT('Ctrl Pts',(-3.7698921652597,2.44290711736645,5.2));
#17362=CARTESIAN_POINT('Ctrl Pts',(-3.76766231085216,2.44841156899725,5.2));
#17363=CARTESIAN_POINT('Ctrl Pts',(-3.76420558690842,2.45694457890368,5.2));
#17364=CARTESIAN_POINT('Ctrl Pts',(-3.7601120066452,2.46519219654187,5.2));
#17365=CARTESIAN_POINT('Ctrl Pts',(-3.75539091261074,2.47305855746262,5.2));
#17366=CARTESIAN_POINT('Ctrl Pts',(-3.75297690030925,2.47708082261811,5.2));
#17367=CARTESIAN_POINT('Ctrl Pts',(-3.75039789825265,2.48100349927224,5.2));
#17368=CARTESIAN_POINT('Ctrl Pts',(-3.74766394598163,2.48480007876844,5.2));
#17369=CARTESIAN_POINT('Ctrl Pts',(-3.74222934299289,2.49234699262488,5.2));
#17370=CARTESIAN_POINT('Ctrl Pts',(-3.73617584476421,2.49941040205976,5.2));
#17371=CARTESIAN_POINT('Ctrl Pts',(-3.7295081017749,2.50587917960273,5.2));
#17372=CARTESIAN_POINT('Ctrl Pts',(-3.72872963243595,2.50663441941712,5.2));
#17373=CARTESIAN_POINT('Ctrl Pts',(-3.72794277607053,2.50738152833223,5.2));
#17374=CARTESIAN_POINT('Ctrl Pts',(-3.72714768981588,2.50812044061668,5.2));
#17375=CARTESIAN_POINT('Origin',(-3.6,2.4,4.7));
#17376=CARTESIAN_POINT('Origin',(-3.6,-2.4,4.3));
#17377=CARTESIAN_POINT('Ctrl Pts',(-3.76351293272515,-2.4319230454628,4.3));
#17378=CARTESIAN_POINT('Ctrl Pts',(-3.76286871316703,-2.44021936733959,
4.3));
#17379=CARTESIAN_POINT('Ctrl Pts',(-3.76155560816075,-2.4484297641735,4.3));
#17380=CARTESIAN_POINT('Ctrl Pts',(-3.75963220162413,-2.45650290122813,
4.3));
#17381=CARTESIAN_POINT('Ctrl Pts',(-3.75857027465495,-2.46096013988305,
4.3));
#17382=CARTESIAN_POINT('Ctrl Pts',(-3.75732202640333,-2.4653756041272,4.3));
#17383=CARTESIAN_POINT('Ctrl Pts',(-3.75589532148576,-2.46974082414556,
4.3));
#17384=CARTESIAN_POINT('Ctrl Pts',(-3.75435560354459,-2.47445182464518,
4.3));
#17385=CARTESIAN_POINT('Ctrl Pts',(-3.75261043098936,-2.47909640157799,
4.3));
#17386=CARTESIAN_POINT('Ctrl Pts',(-3.75067343320617,-2.48365784346818,
4.3));
#17387=CARTESIAN_POINT('Ctrl Pts',(-3.74745266086646,-2.49124244991258,
4.3));
#17388=CARTESIAN_POINT('Ctrl Pts',(-3.74370038620747,-2.49860287239871,
4.3));
#17389=CARTESIAN_POINT('Ctrl Pts',(-3.73945960595045,-2.50569089060563,
4.3));
#17390=CARTESIAN_POINT('Ctrl Pts',(-3.73760643937826,-2.50878826363795,
4.3));
#17391=CARTESIAN_POINT('Ctrl Pts',(-3.73566012601582,-2.511832700902,4.3));
#17392=CARTESIAN_POINT('Ctrl Pts',(-3.73363013483138,-2.51481171247594,
4.3));
#17393=CARTESIAN_POINT('Ctrl Pts',(-3.72675413466501,-2.52490224106299,
4.3));
#17394=CARTESIAN_POINT('Ctrl Pts',(-3.71890630233768,-2.53427022723708,
4.3));
#17395=CARTESIAN_POINT('Ctrl Pts',(-3.710220437496,-2.54276718643201,4.3));
#17396=CARTESIAN_POINT('Ctrl Pts',(-3.70599062580354,-2.54690500552178,
4.3));
#17397=CARTESIAN_POINT('Ctrl Pts',(-3.70156129932866,-2.55083607679561,
4.3));
#17398=CARTESIAN_POINT('Ctrl Pts',(-3.69694397352711,-2.55454119955382,
4.3));
#17399=CARTESIAN_POINT('Ctrl Pts',(-3.69303800092373,-2.55767550469228,
4.3));
#17400=CARTESIAN_POINT('Ctrl Pts',(-3.68899293859581,-2.56065058734466,
4.3));
#17401=CARTESIAN_POINT('Ctrl Pts',(-3.68484116924407,-2.56343733372212,
4.3));
#17402=CARTESIAN_POINT('Ctrl Pts',(-3.67976588279258,-2.56684396230261,
4.3));
#17403=CARTESIAN_POINT('Ctrl Pts',(-3.67452566755957,-2.56997445255576,
4.3));
#17404=CARTESIAN_POINT('Ctrl Pts',(-3.66913578324553,-2.57281068802155,
4.3));
#17405=CARTESIAN_POINT('Ctrl Pts',(-3.66156268589167,-2.57679576192101,
4.3));
#17406=CARTESIAN_POINT('Ctrl Pts',(-3.6536944302201,-2.58020053259861,4.3));
#17407=CARTESIAN_POINT('Ctrl Pts',(-3.64559780863821,-2.58304072868827,
4.3));
#17408=CARTESIAN_POINT('Ctrl Pts',(-3.63968764062526,-2.58511394353595,
4.3));
#17409=CARTESIAN_POINT('Ctrl Pts',(-3.633655561192,-2.58688612240617,4.3));
#17410=CARTESIAN_POINT('Ctrl Pts',(-3.6275253141649,-2.58835973744293,4.3));
#17411=CARTESIAN_POINT('Ctrl Pts',(-3.62399736219549,-2.58920780164787,
4.3));
#17412=CARTESIAN_POINT('Ctrl Pts',(-3.62044138799033,-2.58995568069818,
4.3));
#17413=CARTESIAN_POINT('Ctrl Pts',(-3.61687019594187,-2.59060310935882,
4.3));
#17414=CARTESIAN_POINT('Ctrl Pts',(-3.6053532973959,-2.59269103129053,4.3));
#17415=CARTESIAN_POINT('Ctrl Pts',(-3.5936552916365,-2.5937426794922,4.3));
#17416=CARTESIAN_POINT('Ctrl Pts',(-3.58193296271379,-2.5937913460953,4.3));
#17417=CARTESIAN_POINT('Ctrl Pts',(-3.57526861453522,-2.59381901390686,
4.3));
#17418=CARTESIAN_POINT('Ctrl Pts',(-3.56859601622939,-2.59352191446421,
4.3));
#17419=CARTESIAN_POINT('Ctrl Pts',(-3.56194230797419,-2.5929013482942,4.3));
#17420=CARTESIAN_POINT('Ctrl Pts',(-3.55784543918526,-2.59251924885793,
4.3));
#17421=CARTESIAN_POINT('Ctrl Pts',(-3.55375366053793,-2.59201412364595,
4.3));
#17422=CARTESIAN_POINT('Ctrl Pts',(-3.54967980921583,-2.59138661988454,
4.3));
#17423=CARTESIAN_POINT('Ctrl Pts',(-3.53642388866962,-2.5893447829725,4.3));
#17424=CARTESIAN_POINT('Ctrl Pts',(-3.52344434481125,-2.58602557270852,
4.3));
#17425=CARTESIAN_POINT('Ctrl Pts',(-3.51095537008143,-2.58146161840675,
4.3));
#17426=CARTESIAN_POINT('Ctrl Pts',(-3.50062243383895,-2.57768556394,4.3));
#17427=CARTESIAN_POINT('Ctrl Pts',(-3.49062430896861,-2.57305657702062,
4.3));
#17428=CARTESIAN_POINT('Ctrl Pts',(-3.48108410771908,-2.56756616374223,
4.3));
#17429=CARTESIAN_POINT('Ctrl Pts',(-3.47992982857924,-2.56690187277492,
4.3));
#17430=CARTESIAN_POINT('Ctrl Pts',(-3.47878226433178,-2.56622494144235,
4.3));
#17431=CARTESIAN_POINT('Ctrl Pts',(-3.47764149510761,-2.56553553810743,
4.3));
#17432=CARTESIAN_POINT('Ctrl Pts',(-3.41173724903364,-2.48232321801034,
4.3));
#17433=CARTESIAN_POINT('Ctrl Pts',(-3.40908132671273,-2.474270631223,4.3));
#17434=CARTESIAN_POINT('Ctrl Pts',(-3.40697195813618,-2.46606039521676,
4.3));
#17435=CARTESIAN_POINT('Ctrl Pts',(-3.40539675699364,-2.45774386680553,
4.3));
#17436=CARTESIAN_POINT('Ctrl Pts',(-3.40421043018009,-2.45148046311471,
4.3));
#17437=CARTESIAN_POINT('Ctrl Pts',(-3.40332727350005,-2.44515671203471,
4.3));
#17438=CARTESIAN_POINT('Ctrl Pts',(-3.40274510705531,-2.43879482091291,
4.3));
#17439=CARTESIAN_POINT('Ctrl Pts',(-3.40230912033401,-2.4340303758362,4.3));
#17440=CARTESIAN_POINT('Ctrl Pts',(-3.40204240567473,-2.42924590842869,
4.3));
#17441=CARTESIAN_POINT('Ctrl Pts',(-3.40194407560279,-2.42446300988855,
4.3));
#17442=CARTESIAN_POINT('Ctrl Pts',(-3.4017383892304,-2.41445816568562,4.3));
#17443=CARTESIAN_POINT('Ctrl Pts',(-3.40226690961593,-2.40444523502109,
4.3));
#17444=CARTESIAN_POINT('Ctrl Pts',(-3.40352193796024,-2.39451254861871,
4.3));
#17445=CARTESIAN_POINT('Ctrl Pts',(-3.40417749889618,-2.3893242345667,4.3));
#17446=CARTESIAN_POINT('Ctrl Pts',(-3.4050325722576,-2.38415490381948,4.3));
#17447=CARTESIAN_POINT('Ctrl Pts',(-3.40608153527603,-2.37904223030681,
4.3));
#17448=CARTESIAN_POINT('Ctrl Pts',(-3.40864847953637,-2.36653087604773,
4.3));
#17449=CARTESIAN_POINT('Ctrl Pts',(-3.41237572714265,-2.35432631626979,
4.3));
#17450=CARTESIAN_POINT('Ctrl Pts',(-3.41724961050618,-2.34261710559519,
4.3));
#17451=CARTESIAN_POINT('Ctrl Pts',(-3.41948718042203,-2.33724147889476,
4.3));
#17452=CARTESIAN_POINT('Ctrl Pts',(-3.42196704076708,-2.33197060519316,
4.3));
#17453=CARTESIAN_POINT('Ctrl Pts',(-3.42469079211682,-2.32682518779718,
4.3));
#17454=CARTESIAN_POINT('Ctrl Pts',(-3.42647141933207,-2.32346141883567,
4.3));
#17455=CARTESIAN_POINT('Ctrl Pts',(-3.42835738874669,-2.3201495667824,4.3));
#17456=CARTESIAN_POINT('Ctrl Pts',(-3.430346105223,-2.31690145647487,4.3));
#17457=CARTESIAN_POINT('Ctrl Pts',(-3.43461852095602,-2.30992344943073,
4.3));
#17458=CARTESIAN_POINT('Ctrl Pts',(-3.43934738846969,-2.3032660957291,4.3));
#17459=CARTESIAN_POINT('Ctrl Pts',(-3.44453058590951,-2.29698173842211,
4.3));
#17460=CARTESIAN_POINT('Ctrl Pts',(-3.4502359337428,-2.29006430092116,4.3));
#17461=CARTESIAN_POINT('Ctrl Pts',(-3.45649195144988,-2.28359849259699,
4.3));
#17462=CARTESIAN_POINT('Ctrl Pts',(-3.4632263722909,-2.27761731307503,4.3));
#17463=CARTESIAN_POINT('Ctrl Pts',(-3.46747035511976,-2.27384801742411,
4.3));
#17464=CARTESIAN_POINT('Ctrl Pts',(-3.47190450284819,-2.27027143263625,
4.3));
#17465=CARTESIAN_POINT('Ctrl Pts',(-3.47651159455371,-2.26689859050011,
4.3));
#17466=CARTESIAN_POINT('Ctrl Pts',(-3.4793251060266,-2.26483882467541,4.3));
#17467=CARTESIAN_POINT('Ctrl Pts',(-3.48219970787858,-2.26285776645565,
4.3));
#17468=CARTESIAN_POINT('Ctrl Pts',(-3.48512436737332,-2.26096157786103,
4.3));
#17469=CARTESIAN_POINT('Ctrl Pts',(-3.49373619954507,-2.25537813884111,
4.3));
#17470=CARTESIAN_POINT('Ctrl Pts',(-3.50279847994849,-2.25051611152294,
4.3));
#17471=CARTESIAN_POINT('Ctrl Pts',(-3.51220227087042,-2.24642657080492,
4.3));
#17472=CARTESIAN_POINT('Ctrl Pts',(-3.5210281717619,-2.24258834413989,4.3));
#17473=CARTESIAN_POINT('Ctrl Pts',(-3.53015556945347,-2.23943063412497,
4.3));
#17474=CARTESIAN_POINT('Ctrl Pts',(-3.53949489532435,-2.23701751505981,
4.3));
#17475=CARTESIAN_POINT('Ctrl Pts',(-3.54298225084135,-2.23611644316218,
4.3));
#17476=CARTESIAN_POINT('Ctrl Pts',(-3.54649061678302,-2.23532167500438,
4.3));
#17477=CARTESIAN_POINT('Ctrl Pts',(-3.5500119948057,-2.23463615769257,4.3));
#17478=CARTESIAN_POINT('Ctrl Pts',(-3.5610932074021,-2.23247894451586,4.3));
#17479=CARTESIAN_POINT('Ctrl Pts',(-3.57231428638466,-2.23139729676061,
4.3));
#17480=CARTESIAN_POINT('Ctrl Pts',(-3.58352462409827,-2.2314877485142,4.3));
#17481=CARTESIAN_POINT('Ctrl Pts',(-3.58970653876345,-2.23153762792339,
4.3));
#17482=CARTESIAN_POINT('Ctrl Pts',(-3.59588508216706,-2.23194477463139,
4.3));
#17483=CARTESIAN_POINT('Ctrl Pts',(-3.60203269161667,-2.23273189903069,
4.3));
#17484=CARTESIAN_POINT('Ctrl Pts',(-3.60310835631345,-2.23286962442383,
4.3));
#17485=CARTESIAN_POINT('Ctrl Pts',(-3.60418306761235,-2.23301899515145,
4.3));
#17486=CARTESIAN_POINT('Ctrl Pts',(-3.60525667255607,-2.23317994016621,
4.3));
#17487=CARTESIAN_POINT('Origin',(-3.6,-2.4,5.35459252805377));
#17488=CARTESIAN_POINT('Ctrl Pts',(-3.80565733457988,-2.39985006589818,
5.17959252805377));
#17489=CARTESIAN_POINT('Ctrl Pts',(-3.8057391516022,-2.39002097154438,5.17905813053169));
#17490=CARTESIAN_POINT('Ctrl Pts',(-3.80062938506941,-2.31213685567809,
5.17481913665734));
#17491=CARTESIAN_POINT('Ctrl Pts',(-3.70109554203788,-2.17915701647198,
5.16687554643073));
#17492=CARTESIAN_POINT('Ctrl Pts',(-3.46929950206046,-2.19531102353728,
5.15576175737392));
#17493=CARTESIAN_POINT('Ctrl Pts',(-3.35713783153282,-2.39878694399818,
5.14464796831711));
#17494=CARTESIAN_POINT('Ctrl Pts',(-3.46726929886284,-2.60338928299931,
5.13353417926032));
#17495=CARTESIAN_POINT('Ctrl Pts',(-3.69889136100131,-2.62181906697108,
5.12242039020351));
#17496=CARTESIAN_POINT('Ctrl Pts',(-3.80021578451737,-2.48926235936684,
5.11443983980133));
#17497=CARTESIAN_POINT('Ctrl Pts',(-3.80572902589707,-2.41067410853188,
5.11016388575141));
#17498=CARTESIAN_POINT('Ctrl Pts',(-3.8056388038084,-2.40016037433918,5.10959252805377));
#17499=CARTESIAN_POINT('Ctrl Pts',(-3.80526708169851,-2.40022955265959,
5.18540747194623));
#17500=CARTESIAN_POINT('Ctrl Pts',(-3.80491230300414,-2.3532097525552,5.18286245525962));
#17501=CARTESIAN_POINT('Ctrl Pts',(-3.76565541968849,-2.23704708335906,
5.17661284222073));
#17502=CARTESIAN_POINT('Ctrl Pts',(-3.5727867642971,-2.15871465280967,5.16665863282959));
#17503=CARTESIAN_POINT('Ctrl Pts',(-3.38252461999799,-2.29190667528476,
5.15554484377278));
#17504=CARTESIAN_POINT('Ctrl Pts',(-3.39123766053156,-2.52413789941101,
5.14443105471598));
#17505=CARTESIAN_POINT('Ctrl Pts',(-3.59107442597796,-2.64269432067786,
5.13331726565918));
#17506=CARTESIAN_POINT('Ctrl Pts',(-3.77212564872883,-2.55254602634109,
5.12364273806926));
#17507=CARTESIAN_POINT('Ctrl Pts',(-3.80499226553068,-2.44179202539712,
5.11767280683161));
#17508=CARTESIAN_POINT('Ctrl Pts',(-3.80520912268496,-2.39988380060309,
5.11540747194623));
#17509=CARTESIAN_POINT('Ctrl Pts',(-3.47309291201476,-2.29206413469515,
5.2));
#17510=CARTESIAN_POINT('Ctrl Pts',(-3.43720166889934,-2.33426376069605,
5.19629540364773));
#17511=CARTESIAN_POINT('Ctrl Pts',(-3.4114791580674,-2.45658678033172,5.1888862109432));
#17512=CARTESIAN_POINT('Ctrl Pts',(-3.54548746492724,-2.5893415011903,5.17777242188639));
#17513=CARTESIAN_POINT('Ctrl Pts',(-3.72942274690437,-2.54835673318009,
5.16665863282959));
#17514=CARTESIAN_POINT('Ctrl Pts',(-3.79487861290014,-2.37179020383286,
5.15554484377278));
#17515=CARTESIAN_POINT('Ctrl Pts',(-3.68196869353212,-2.22093957388603,
5.14443105471598));
#17516=CARTESIAN_POINT('Ctrl Pts',(-3.49402748287272,-2.23403731121212,
5.13331726565918));
#17517=CARTESIAN_POINT('Ctrl Pts',(-3.40308632550611,-2.39901644905753,
5.12220347660237));
#17518=CARTESIAN_POINT('Ctrl Pts',(-3.49238138552402,-2.56490889182472,
5.11108968754557));
#17519=CARTESIAN_POINT('Ctrl Pts',(-3.68018153421496,-2.57985183870243,
5.09997589848876));
#17520=CARTESIAN_POINT('Ctrl Pts',(-3.79459034046341,-2.43017761257843,
5.08886210943196));
#17521=CARTESIAN_POINT('Ctrl Pts',(-3.73088853854501,-2.25287985005212,
5.07774832037516));
#17522=CARTESIAN_POINT('Ctrl Pts',(-3.5473829043692,-2.21024364094684,5.06663453131835));
#17523=CARTESIAN_POINT('Ctrl Pts',(-3.41203832877697,-2.34129317389102,
5.05552074226154));
#17524=CARTESIAN_POINT('Ctrl Pts',(-3.44873718538878,-2.52607793299967,
5.04440695320475));
#17525=CARTESIAN_POINT('Ctrl Pts',(-3.62388862018941,-2.59546202911018,
5.03329316414794));
#17526=CARTESIAN_POINT('Ctrl Pts',(-3.77717452575129,-2.48593756377701,
5.02217937509113));
#17527=CARTESIAN_POINT('Ctrl Pts',(-3.76829058072669,-2.29775344650504,
5.01106558603433));
#17528=CARTESIAN_POINT('Ctrl Pts',(-3.6053683575545,-2.20315677179449,4.99995179697753));
#17529=CARTESIAN_POINT('Ctrl Pts',(-3.43753241636245,-2.28873292992563,
4.98883800792072));
#17530=CARTESIAN_POINT('Ctrl Pts',(-3.41840489671633,-2.47615310229093,
4.97772421886392));
#17531=CARTESIAN_POINT('Ctrl Pts',(-3.56549343466676,-2.59386947492594,
4.96661042980711));
#17532=CARTESIAN_POINT('Ctrl Pts',(-3.74416622313161,-2.53413491931517,
4.95549664075031));
#17533=CARTESIAN_POINT('Ctrl Pts',(-3.79088203264097,-2.35162515047058,
4.9443828516935));
#17534=CARTESIAN_POINT('Ctrl Pts',(-3.66288135290806,-2.21339343020375,
4.9332690626367));
#17535=CARTESIAN_POINT('Ctrl Pts',(-3.47732465774361,-2.24596481943629,
4.9221552735799));
#17536=CARTESIAN_POINT('Ctrl Pts',(-3.40405409457531,-2.41952635636528,
4.91104148452309));
#17537=CARTESIAN_POINT('Ctrl Pts',(-3.51013504082201,-2.57521519784486,
4.89992769546629));
#17538=CARTESIAN_POINT('Ctrl Pts',(-3.69847040334124,-2.57052758167369,
4.88881390640948));
#17539=CARTESIAN_POINT('Ctrl Pts',(-3.79667468895243,-2.40975413607622,
4.87770011735268));
#17540=CARTESIAN_POINT('Ctrl Pts',(-3.71486040132253,-2.24005261911178,
4.86658632829587));
#17541=CARTESIAN_POINT('Ctrl Pts',(-3.5279130857567,-2.2167527537995,4.85547253923907));
#17542=CARTESIAN_POINT('Ctrl Pts',(-3.40694774031892,-2.3611811711004,4.84435875018227));
#17543=CARTESIAN_POINT('Ctrl Pts',(-3.46268531752878,-2.5411409027282,4.83324496112546));
#17544=CARTESIAN_POINT('Ctrl Pts',(-3.64410858085897,-2.59191276544236,
4.82213117206866));
#17545=CARTESIAN_POINT('Ctrl Pts',(-3.7851587599036,-2.46702469750825,4.81101738301185));
#17546=CARTESIAN_POINT('Ctrl Pts',(-3.75673102616532,-2.28078816383312,
4.79990359395505));
#17547=CARTESIAN_POINT('Ctrl Pts',(-3.58484560672719,-2.20366757575568,
4.78878980489824));
#17548=CARTESIAN_POINT('Ctrl Pts',(-3.42683117531417,-2.30625228215021,
4.77767601584145));
#17549=CARTESIAN_POINT('Ctrl Pts',(-3.42732013300413,-2.49464533786407,
4.76656222678464));
#17550=CARTESIAN_POINT('Ctrl Pts',(-3.5858649312783,-2.59640844247982,4.75544843772783));
#17551=CARTESIAN_POINT('Ctrl Pts',(-3.75734771825602,-2.51839667227055,
4.74433464867103));
#17552=CARTESIAN_POINT('Ctrl Pts',(-3.78480835426951,-2.33201508522246,
4.73322085961423));
#17553=CARTESIAN_POINT('Ctrl Pts',(-3.64311180775084,-2.20786086167162,
4.72210707055742));
#17554=CARTESIAN_POINT('Ctrl Pts',(-3.46195453467666,-2.25957377043879,
4.71099328150062));
#17555=CARTESIAN_POINT('Ctrl Pts',(-3.407151841555,-2.43982039966509,4.69987949244381));
#17556=CARTESIAN_POINT('Ctrl Pts',(-3.52886525490491,-2.58361896548389,
4.68876570338701));
#17557=CARTESIAN_POINT('Ctrl Pts',(-3.71568910716324,-2.55934900981458,
4.6776519143302));
#17558=CARTESIAN_POINT('Ctrl Pts',(-3.79662140763134,-2.38922509832133,
4.6665381252734));
#17559=CARTESIAN_POINT('Ctrl Pts',(-3.69758390385606,-2.22896357653021,
4.65542433621659));
#17560=CARTESIAN_POINT('Ctrl Pts',(-3.50922674620458,-2.22525363282606,
4.64431054715979));
#17561=CARTESIAN_POINT('Ctrl Pts',(-3.40395537719079,-2.38149102075462,
4.63319675810299));
#17562=CARTESIAN_POINT('Ctrl Pts',(-3.47812587473144,-2.55466988729295,
4.62208296904618));
#17563=CARTESIAN_POINT('Ctrl Pts',(-3.66384914127714,-2.58627765191548,
4.61096917998938));
#17564=CARTESIAN_POINT('Ctrl Pts',(-3.79113056471305,-2.447383369209,4.59985539093257));
#17565=CARTESIAN_POINT('Ctrl Pts',(-3.74346801469971,-2.26511855129859,
4.58874160187577));
#17566=CARTESIAN_POINT('Ctrl Pts',(-3.56448756379251,-2.20631225305021,
4.57762781281896));
#17567=CARTESIAN_POINT('Ctrl Pts',(-3.41801204848697,-2.32479054614148,
4.56651402376216));
#17568=CARTESIAN_POINT('Ctrl Pts',(-3.43811216908,-2.51210890530657,4.55540023470536));
#17569=CARTESIAN_POINT('Ctrl Pts',(-3.60639005725709,-2.59681271199525,
4.54428644564855));
#17570=CARTESIAN_POINT('Ctrl Pts',(-3.76881905353834,-2.50137161148251,
4.53317265659175));
#17571=CARTESIAN_POINT('Ctrl Pts',(-3.77672605561821,-2.31314392515575,
4.52205886753495));
#17572=CARTESIAN_POINT('Ctrl Pts',(-3.62287369469976,-2.2044165895329,4.51094507847814));
#17573=CARTESIAN_POINT('Ctrl Pts',(-3.44808478177985,-2.27470896680823,
4.49983128942134));
#17574=CARTESIAN_POINT('Ctrl Pts',(-3.41234559060706,-2.45968164920097,
4.48871750036453));
#17575=CARTESIAN_POINT('Ctrl Pts',(-3.54836860914922,-2.5900270381604,4.47760371130773));
#17576=CARTESIAN_POINT('Ctrl Pts',(-3.73165042397165,-2.54643853021323,
4.46648992225092));
#17577=CARTESIAN_POINT('Ctrl Pts',(-3.79443111532907,-2.36881316247168,
4.45537613319412));
#17578=CARTESIAN_POINT('Ctrl Pts',(-3.67924679659355,-2.21973348556073,
4.44426234413731));
#17579=CARTESIAN_POINT('Ctrl Pts',(-3.49152699669547,-2.23565374410205,
4.43314855508051));
#17580=CARTESIAN_POINT('Ctrl Pts',(-3.40309374590592,-2.40200209374894,
4.4220347660237));
#17581=CARTESIAN_POINT('Ctrl Pts',(-3.49489106457482,-2.5665177055076,4.41092097696691));
#17582=CARTESIAN_POINT('Ctrl Pts',(-3.68289569971986,-2.57861817099917,
4.39980718791009));
#17583=CARTESIAN_POINT('Ctrl Pts',(-3.79502512928071,-2.42722660191142,
4.3886933988533));
#17584=CARTESIAN_POINT('Ctrl Pts',(-3.72864550893249,-2.25091581121659,
4.37757960979648));
#17585=CARTESIAN_POINT('Ctrl Pts',(-3.54451587080997,-2.21106027365159,
4.36646582073969));
#17586=CARTESIAN_POINT('Ctrl Pts',(-3.41117013277341,-2.34414980914689,
4.35535203168287));
#17587=CARTESIAN_POINT('Ctrl Pts',(-3.45066522211898,-2.5283468448043,4.34423824262609));
#17588=CARTESIAN_POINT('Ctrl Pts',(-3.62684270366593,-2.59509221455348,
4.33312445356927));
#17589=CARTESIAN_POINT('Ctrl Pts',(-3.77846161739066,-2.4832160890933,4.32201066451248));
#17590=CARTESIAN_POINT('Ctrl Pts',(-3.76671079422265,-2.29527426875025,
4.31089687545566));
#17591=CARTESIAN_POINT('Ctrl Pts',(-3.60241192612029,-2.2029822262702,4.29978308639886));
#17592=CARTESIAN_POINT('Ctrl Pts',(-3.43581020892599,-2.29144640006724,
4.28866929734205));
#17593=CARTESIAN_POINT('Ctrl Pts',(-3.42516046182893,-2.41599017382995,
4.28126010463752));
#17594=CARTESIAN_POINT('Ctrl Pts',(-3.44735576439472,-2.46674801372685,
4.27755550828525));
#17595=CARTESIAN_POINT('Ctrl Pts',(-3.46322193753412,-2.28366876301903,
5.20748149723825));
#17596=CARTESIAN_POINT('Ctrl Pts',(-3.42453903360214,-2.32915072287504,
5.20377690088598));
#17597=CARTESIAN_POINT('Ctrl Pts',(-3.39681579726281,-2.4609881630556,5.19636770818145));
#17598=CARTESIAN_POINT('Ctrl Pts',(-3.54124741930709,-2.60406869378488,
5.18525391912464));
#17599=CARTESIAN_POINT('Ctrl Pts',(-3.73948939213428,-2.55989608492554,
5.17414013006784));
#17600=CARTESIAN_POINT('Ctrl Pts',(-3.81003648820324,-2.36959601450513,
5.16302634101103));
#17601=CARTESIAN_POINT('Ctrl Pts',(-3.68834430970071,-2.20701205474802,
5.15191255195423));
#17602=CARTESIAN_POINT('Ctrl Pts',(-3.48578482260197,-2.22112854865384,
5.14079876289742));
#17603=CARTESIAN_POINT('Ctrl Pts',(-3.38777016084835,-2.39893994737108,
5.12968497384062));
#17604=CARTESIAN_POINT('Ctrl Pts',(-3.4840106899703,-2.57773568888292,5.11857118478382));
#17605=CARTESIAN_POINT('Ctrl Pts',(-3.68641814314374,-2.59384091479198,
5.10745739572701));
#17606=CARTESIAN_POINT('Ctrl Pts',(-3.8097257936157,-2.43252486085572,5.0963436066702));
#17607=CARTESIAN_POINT('Ctrl Pts',(-3.74106919467933,-2.2414366811261,5.08522981761341));
#17608=CARTESIAN_POINT('Ctrl Pts',(-3.54329028813742,-2.19548418024617,
5.0741160285566));
#17609=CARTESIAN_POINT('Ctrl Pts',(-3.39741846089223,-2.33672689164815,
5.06300223949979));
#17610=CARTESIAN_POINT('Ctrl Pts',(-3.43697179539676,-2.53588441488314,
5.051888450443));
#17611=CARTESIAN_POINT('Ctrl Pts',(-3.62574670364252,-2.61066528317513,
5.04077466138618));
#17612=CARTESIAN_POINT('Ctrl Pts',(-3.79095535746114,-2.4926218830884,5.02966087232938));
#17613=CARTESIAN_POINT('Ctrl Pts',(-3.78138040930963,-2.28980059583054,
5.01854708327258));
#17614=CARTESIAN_POINT('Ctrl Pts',(-3.60578591437709,-2.1878460865274,5.00743329421578));
#17615=CARTESIAN_POINT('Ctrl Pts',(-3.42489550697087,-2.28007845343676,
4.99631950515897));
#17616=CARTESIAN_POINT('Ctrl Pts',(-3.40428022756837,-2.48207637530325,
4.98520571610216));
#17617=CARTESIAN_POINT('Ctrl Pts',(-3.56280947562848,-2.60894885835481,
4.97409192704536));
#17618=CARTESIAN_POINT('Ctrl Pts',(-3.75537963234378,-2.54456808255722,
4.96297813798856));
#17619=CARTESIAN_POINT('Ctrl Pts',(-3.80572904948554,-2.34786250085983,
4.95186434893175));
#17620=CARTESIAN_POINT('Ctrl Pts',(-3.6677723344893,-2.19887896361545,4.94075055987495));
#17621=CARTESIAN_POINT('Ctrl Pts',(-3.46778283315333,-2.23398379173638,
4.92963677081814));
#17622=CARTESIAN_POINT('Ctrl Pts',(-3.38881320407234,-2.42104513808537,
4.91852298176134));
#17623=CARTESIAN_POINT('Ctrl Pts',(-3.50314524432732,-2.5888436308505,4.90740919270454));
#17624=CARTESIAN_POINT('Ctrl Pts',(-3.70612954085602,-2.58379140667882,
4.89629540364773));
#17625=CARTESIAN_POINT('Ctrl Pts',(-3.81197226504892,-2.41051282363117,
4.88518161459093));
#17626=CARTESIAN_POINT('Ctrl Pts',(-3.72379437111327,-2.22761173389364,
4.87406782553412));
#17627=CARTESIAN_POINT('Ctrl Pts',(-3.52230608537413,-2.20249957913754,
4.86295403647732));
#17628=CARTESIAN_POINT('Ctrl Pts',(-3.3919319208009,-2.35816179940478,4.85184024742052));
#17629=CARTESIAN_POINT('Ctrl Pts',(-3.45200482877115,-2.55211899915388,
4.84072645836371));
#17630=CARTESIAN_POINT('Ctrl Pts',(-3.64753939534654,-2.60683995383086,
4.82961266930691));
#17631=CARTESIAN_POINT('Ctrl Pts',(-3.79956061422784,-2.47223795304173,
4.8184988802501));
#17632=CARTESIAN_POINT('Ctrl Pts',(-3.7689217397351,-2.27151573459945,4.8073850911933));
#17633=CARTESIAN_POINT('Ctrl Pts',(-3.58366688116,-2.18839662138894,4.79627130213649));
#17634=CARTESIAN_POINT('Ctrl Pts',(-3.41336191148932,-2.29896048036668,
4.78515751307969));
#17635=CARTESIAN_POINT('Ctrl Pts',(-3.41388890085234,-2.50200695753087,
4.77404372402289));
#17636=CARTESIAN_POINT('Ctrl Pts',(-3.58476548990864,-2.61168530962949,
4.76292993496608));
#17637=CARTESIAN_POINT('Ctrl Pts',(-3.76958639882265,-2.52760569714953,
4.75181614590928));
#17638=CARTESIAN_POINT('Ctrl Pts',(-3.79918295365372,-2.32672714292159,
4.74070235685248));
#17639=CARTESIAN_POINT('Ctrl Pts',(-3.64646509211721,-2.19291606574822,
4.72958856779567));
#17640=CARTESIAN_POINT('Ctrl Pts',(-3.45121720481583,-2.24865126208706,
4.71847477873887));
#17641=CARTESIAN_POINT('Ctrl Pts',(-3.39215189725818,-2.44291767464904,
4.70736098968205));
#17642=CARTESIAN_POINT('Ctrl Pts',(-3.52333231529793,-2.59790105288522,
4.69624720062526));
#17643=CARTESIAN_POINT('Ctrl Pts',(-3.72468753461616,-2.57174335306496,
4.68513341156845));
#17644=CARTESIAN_POINT('Ctrl Pts',(-3.8119148394474,-2.38838701448227,4.67401962251165));
#17645=CARTESIAN_POINT('Ctrl Pts',(-3.70517408845471,-2.21566017324412,
4.66290583345485));
#17646=CARTESIAN_POINT('Ctrl Pts',(-3.50216630154411,-2.21166166599155,
4.65179204439804));
#17647=CARTESIAN_POINT('Ctrl Pts',(-3.38870680833984,-2.38005137175869,
4.64067825534123));
#17648=CARTESIAN_POINT('Ctrl Pts',(-3.46864636968979,-2.56670028318833,
4.62956446628443));
#17649=CARTESIAN_POINT('Ctrl Pts',(-3.66881539851434,-2.6007665349051,4.61845067722763));
#17650=CARTESIAN_POINT('Ctrl Pts',(-3.80599691265867,-2.45106890037747,
4.60733688817082));
#17651=CARTESIAN_POINT('Ctrl Pts',(-3.75462711648332,-2.25462732217041,
4.59622309911401));
#17652=CARTESIAN_POINT('Ctrl Pts',(-3.56172536699866,-2.1912470046255,4.58510931005722));
#17653=CARTESIAN_POINT('Ctrl Pts',(-3.4038568231667,-2.31894067115399,4.57399552100041));
#17654=CARTESIAN_POINT('Ctrl Pts',(-3.42552035349974,-2.5208288606763,4.56288173194361));
#17655=CARTESIAN_POINT('Ctrl Pts',(-3.60688708301913,-2.61212102367755,
4.5517679428868));
#17656=CARTESIAN_POINT('Ctrl Pts',(-3.78194998732446,-2.50925640819396,
4.54065415383));
#17657=CARTESIAN_POINT('Ctrl Pts',(-3.79047200482221,-2.30638816303176,
4.52954036477319));
#17658=CARTESIAN_POINT('Ctrl Pts',(-3.62465283611923,-2.18920389429099,
4.51842657571639));
#17659=CARTESIAN_POINT('Ctrl Pts',(-3.43626864710937,-2.2649636908672,4.50731278665958));
#17660=CARTESIAN_POINT('Ctrl Pts',(-3.39774962188927,-2.46432375426836,
4.49619899760278));
#17661=CARTESIAN_POINT('Ctrl Pts',(-3.54435266213177,-2.60480755258314,
4.48508520854598));
#17662=CARTESIAN_POINT('Ctrl Pts',(-3.74189034040202,-2.55782868199802,
4.47397141948917));
#17663=CARTESIAN_POINT('Ctrl Pts',(-3.80955418377328,-2.36638741555509,
4.46285763043236));
#17664=CARTESIAN_POINT('Ctrl Pts',(-3.68541070059029,-2.20571215553106,
4.45174384137557));
#17665=CARTESIAN_POINT('Ctrl Pts',(-3.4830898458282,-2.22287070949214,4.44063005231875));
#17666=CARTESIAN_POINT('Ctrl Pts',(-3.3877781584151,-2.40215781882795,4.42951626326196));
#17667=CARTESIAN_POINT('Ctrl Pts',(-3.48671557464955,-2.57946963788377,
4.41840247420515));
#17668=CARTESIAN_POINT('Ctrl Pts',(-3.68934341946097,-2.59251129104238,
4.40728868514835));
#17669=CARTESIAN_POINT('Ctrl Pts',(-3.81019440079089,-2.42934431729619,
4.39617489609154));
#17670=CARTESIAN_POINT('Ctrl Pts',(-3.73865169972831,-2.23931987716506,
4.38506110703474));
#17671=CARTESIAN_POINT('Ctrl Pts',(-3.54020025351852,-2.19636433155117,
4.37394731797794));
#17672=CARTESIAN_POINT('Ctrl Pts',(-3.39648273563768,-2.33980571917207,
4.36283352892113));
#17673=CARTESIAN_POINT('Ctrl Pts',(-3.43904979696867,-2.53832980517198,
4.35171973986433));
#17674=CARTESIAN_POINT('Ctrl Pts',(-3.6289305590181,-2.6102667040308,4.34060595080752));
#17675=CARTESIAN_POINT('Ctrl Pts',(-3.79234256052004,-2.48968872907629,
4.32949216175072));
#17676=CARTESIAN_POINT('Ctrl Pts',(-3.77967774525388,-2.28712858487203,
4.31837837269391));
#17677=CARTESIAN_POINT('Ctrl Pts',(-3.60259952841706,-2.18765796465806,
4.30726458363711));
#17678=CARTESIAN_POINT('Ctrl Pts',(-3.42303934432415,-2.28300298030457,
4.29615079458031));
#17679=CARTESIAN_POINT('Ctrl Pts',(-3.41156124805061,-2.41723390733863,
4.28874160187577));
#17680=CARTESIAN_POINT('Ctrl Pts',(-3.43548292594103,-2.47193974848801,
4.2850370055235));
#17681=CARTESIAN_POINT('Ctrl Pts',(-3.45335096305347,-2.2752733913429,5.2149629944765));
#17682=CARTESIAN_POINT('Ctrl Pts',(-3.41187639830495,-2.32403768505403,
5.21125839812423));
#17683=CARTESIAN_POINT('Ctrl Pts',(-3.38215243645823,-2.46538954577948,
5.20384920541969));
#17684=CARTESIAN_POINT('Ctrl Pts',(-3.53700737368693,-2.61879588637947,
5.19273541636289));
#17685=CARTESIAN_POINT('Ctrl Pts',(-3.74955603736419,-2.571435436671,5.18162162730609));
#17686=CARTESIAN_POINT('Ctrl Pts',(-3.82519436350635,-2.3674018251774,5.17050783824928));
#17687=CARTESIAN_POINT('Ctrl Pts',(-3.69471992586929,-2.19308453561,5.15939404919247));
#17688=CARTESIAN_POINT('Ctrl Pts',(-3.47754216233122,-2.20821978609556,
5.14828026013568));
#17689=CARTESIAN_POINT('Ctrl Pts',(-3.37245399619058,-2.39886344568463,
5.13716647107886));
#17690=CARTESIAN_POINT('Ctrl Pts',(-3.47563999441657,-2.59056248594111,
5.12605268202207));
#17691=CARTESIAN_POINT('Ctrl Pts',(-3.69265475207253,-2.60782999088153,
5.11493889296526));
#17692=CARTESIAN_POINT('Ctrl Pts',(-3.82486124676799,-2.434872109133,5.10382510390846));
#17693=CARTESIAN_POINT('Ctrl Pts',(-3.75124985081366,-2.22999351220008,
5.09271131485165));
#17694=CARTESIAN_POINT('Ctrl Pts',(-3.53919767190563,-2.18072471954551,
5.08159752579485));
#17695=CARTESIAN_POINT('Ctrl Pts',(-3.38279859300748,-2.33216060940528,
5.07048373673804));
#17696=CARTESIAN_POINT('Ctrl Pts',(-3.42520640540474,-2.54569089676662,
5.05936994768124));
#17697=CARTESIAN_POINT('Ctrl Pts',(-3.62760478709563,-2.62586853724007,
5.04825615862444));
#17698=CARTESIAN_POINT('Ctrl Pts',(-3.80473618917098,-2.49930620239979,
5.03714236956763));
#17699=CARTESIAN_POINT('Ctrl Pts',(-3.79447023789256,-2.28184774515603,
5.02602858051083));
#17700=CARTESIAN_POINT('Ctrl Pts',(-3.60620347119968,-2.17253540126032,
5.01491479145402));
#17701=CARTESIAN_POINT('Ctrl Pts',(-3.4122585975793,-2.27142397694788,5.00380100239722));
#17702=CARTESIAN_POINT('Ctrl Pts',(-3.39015555842041,-2.48799964831557,
4.99268721334041));
#17703=CARTESIAN_POINT('Ctrl Pts',(-3.56012551659021,-2.62402824178367,
4.98157342428361));
#17704=CARTESIAN_POINT('Ctrl Pts',(-3.76659304155595,-2.55500124579927,
4.97045963522681));
#17705=CARTESIAN_POINT('Ctrl Pts',(-3.82057606633011,-2.34409985124907,
4.95934584617));
#17706=CARTESIAN_POINT('Ctrl Pts',(-3.67266331607053,-2.18436449702716,
4.9482320571132));
#17707=CARTESIAN_POINT('Ctrl Pts',(-3.45824100856306,-2.22200276403647,
4.93711826805639));
#17708=CARTESIAN_POINT('Ctrl Pts',(-3.37357231356937,-2.42256391980546,
4.92600447899959));
#17709=CARTESIAN_POINT('Ctrl Pts',(-3.49615544783263,-2.60247206385614,
4.91489068994279));
#17710=CARTESIAN_POINT('Ctrl Pts',(-3.71378867837081,-2.59705523168396,
4.90377690088598));
#17711=CARTESIAN_POINT('Ctrl Pts',(-3.82726984114541,-2.41127151118611,
4.89266311182918));
#17712=CARTESIAN_POINT('Ctrl Pts',(-3.73272834090401,-2.21517084867549,
4.88154932277237));
#17713=CARTESIAN_POINT('Ctrl Pts',(-3.51669908499156,-2.18824640447558,
4.87043553371557));
#17714=CARTESIAN_POINT('Ctrl Pts',(-3.37691610128289,-2.35514242770916,
4.85932174465877));
#17715=CARTESIAN_POINT('Ctrl Pts',(-3.44132434001351,-2.56309709557957,
4.84820795560196));
#17716=CARTESIAN_POINT('Ctrl Pts',(-3.65097020983412,-2.62176714221935,
4.83709416654516));
#17717=CARTESIAN_POINT('Ctrl Pts',(-3.81396246855208,-2.47745120857521,
4.82598037748835));
#17718=CARTESIAN_POINT('Ctrl Pts',(-3.78111245330488,-2.26224330536578,
4.81486658843155));
#17719=CARTESIAN_POINT('Ctrl Pts',(-3.58248815559281,-2.1731256670222,4.80375279937474));
#17720=CARTESIAN_POINT('Ctrl Pts',(-3.39989264766446,-2.29166867858314,
4.79263901031794));
#17721=CARTESIAN_POINT('Ctrl Pts',(-3.40045766870055,-2.50936857719767,
4.78152522126113));
#17722=CARTESIAN_POINT('Ctrl Pts',(-3.58366604853898,-2.62696217677915,
4.77041143220433));
#17723=CARTESIAN_POINT('Ctrl Pts',(-3.78182507938928,-2.53681472202852,
4.75929764314753));
#17724=CARTESIAN_POINT('Ctrl Pts',(-3.81355755303793,-2.32143920062071,
4.74818385409072));
#17725=CARTESIAN_POINT('Ctrl Pts',(-3.64981837648358,-2.17797126982482,
4.73707006503392));
#17726=CARTESIAN_POINT('Ctrl Pts',(-3.440479874955,-2.23772875373533,4.72595627597712));
#17727=CARTESIAN_POINT('Ctrl Pts',(-3.37715195296136,-2.44601494963299,
4.71484248692031));
#17728=CARTESIAN_POINT('Ctrl Pts',(-3.51779937569094,-2.61218314028655,
4.7037286978635));
#17729=CARTESIAN_POINT('Ctrl Pts',(-3.73368596206909,-2.58413769631535,
4.69261490880671));
#17730=CARTESIAN_POINT('Ctrl Pts',(-3.82720827126346,-2.38754893064322,
4.68150111974989));
#17731=CARTESIAN_POINT('Ctrl Pts',(-3.71276427305336,-2.20235676995803,
4.6703873306931));
#17732=CARTESIAN_POINT('Ctrl Pts',(-3.49510585688365,-2.19806969915704,
4.65927354163628));
#17733=CARTESIAN_POINT('Ctrl Pts',(-3.37345823948888,-2.37861172276277,
4.64815975257949));
#17734=CARTESIAN_POINT('Ctrl Pts',(-3.45916686464814,-2.57873067908372,
4.63704596352267));
#17735=CARTESIAN_POINT('Ctrl Pts',(-3.67378165575153,-2.61525541789472,
4.62593217446588));
#17736=CARTESIAN_POINT('Ctrl Pts',(-3.82086326060429,-2.45475443154594,
4.61481838540906));
#17737=CARTESIAN_POINT('Ctrl Pts',(-3.76578621826694,-2.24413609304223,
4.60370459635227));
#17738=CARTESIAN_POINT('Ctrl Pts',(-3.55896317020481,-2.17618175620078,
4.59259080729546));
#17739=CARTESIAN_POINT('Ctrl Pts',(-3.38970159784644,-2.3130907961665,4.58147701823866));
#17740=CARTESIAN_POINT('Ctrl Pts',(-3.41292853791948,-2.52954881604603,
4.57036322918185));
#17741=CARTESIAN_POINT('Ctrl Pts',(-3.60738410878117,-2.62742933535986,
4.55924944012506));
#17742=CARTESIAN_POINT('Ctrl Pts',(-3.79508092111058,-2.51714120490541,
4.54813565106824));
#17743=CARTESIAN_POINT('Ctrl Pts',(-3.8042179540262,-2.29963240090777,4.53702186201145));
#17744=CARTESIAN_POINT('Ctrl Pts',(-3.62643197753871,-2.17399119904908,
4.52590807295463));
#17745=CARTESIAN_POINT('Ctrl Pts',(-3.42445251243888,-2.25521841492616,
4.51479428389784));
#17746=CARTESIAN_POINT('Ctrl Pts',(-3.38315365317149,-2.46896585933577,
4.50368049484102));
#17747=CARTESIAN_POINT('Ctrl Pts',(-3.54033671511431,-2.61958806700588,
4.49256670578423));
#17748=CARTESIAN_POINT('Ctrl Pts',(-3.75213025683239,-2.56921883378282,
4.48145291672742));
#17749=CARTESIAN_POINT('Ctrl Pts',(-3.82467725221749,-2.3639616686385,4.47033912767062));
#17750=CARTESIAN_POINT('Ctrl Pts',(-3.69157460458704,-2.1916908255014,4.45922533861381));
#17751=CARTESIAN_POINT('Ctrl Pts',(-3.47465269496093,-2.21008767488223,
4.44811154955701));
#17752=CARTESIAN_POINT('Ctrl Pts',(-3.37246257092429,-2.40231354390696,
4.4369977605002));
#17753=CARTESIAN_POINT('Ctrl Pts',(-3.47854008472427,-2.59242157025994,
4.4258839714434));
#17754=CARTESIAN_POINT('Ctrl Pts',(-3.69579113920209,-2.60640441108558,
4.41477018238659));
#17755=CARTESIAN_POINT('Ctrl Pts',(-3.82536367230107,-2.43146203268096,
4.4036563933298));
#17756=CARTESIAN_POINT('Ctrl Pts',(-3.74865789052413,-2.22772394311352,
4.39254260427298));
#17757=CARTESIAN_POINT('Ctrl Pts',(-3.53588463622708,-2.18166838945074,
4.38142881521619));
#17758=CARTESIAN_POINT('Ctrl Pts',(-3.38179533850196,-2.33546162919725,
4.37031502615938));
#17759=CARTESIAN_POINT('Ctrl Pts',(-3.42743437181836,-2.54831276553967,
4.35920123710258));
#17760=CARTESIAN_POINT('Ctrl Pts',(-3.63101841437027,-2.62544119350812,
4.34808744804577));
#17761=CARTESIAN_POINT('Ctrl Pts',(-3.80622350364941,-2.49616136905929,
4.33697365898897));
#17762=CARTESIAN_POINT('Ctrl Pts',(-3.7926446962851,-2.27898290099381,4.32585986993216));
#17763=CARTESIAN_POINT('Ctrl Pts',(-3.60278713071383,-2.17233370304593,
4.31474608087535));
#17764=CARTESIAN_POINT('Ctrl Pts',(-3.4102684797223,-2.27455956054189,4.30363229181856));
#17765=CARTESIAN_POINT('Ctrl Pts',(-3.3979620342723,-2.41847764084731,4.29622309911402));
#17766=CARTESIAN_POINT('Ctrl Pts',(-3.42361008748733,-2.47713148324918,
4.29251850276175));
#17767=CARTESIAN_POINT('Ctrl Pts',(-3.44347998857283,-2.26687801966678,
5.22244449171475));
#17768=CARTESIAN_POINT('Ctrl Pts',(-3.39921376300775,-2.31892464723302,
5.21873989536248));
#17769=CARTESIAN_POINT('Ctrl Pts',(-3.36748907565365,-2.46979092850336,
5.21133070265795));
#17770=CARTESIAN_POINT('Ctrl Pts',(-3.53276732806678,-2.63352307897406,
5.20021691360113));
#17771=CARTESIAN_POINT('Ctrl Pts',(-3.75962268259409,-2.58297478841644,
5.18910312454434));
#17772=CARTESIAN_POINT('Ctrl Pts',(-3.84035223880946,-2.36520763584968,
5.17798933548753));
#17773=CARTESIAN_POINT('Ctrl Pts',(-3.70109554203788,-2.17915701647198,
5.16687554643073));
#17774=CARTESIAN_POINT('Ctrl Pts',(-3.46929950206046,-2.19531102353728,
5.15576175737392));
#17775=CARTESIAN_POINT('Ctrl Pts',(-3.35713783153282,-2.39878694399818,
5.14464796831711));
#17776=CARTESIAN_POINT('Ctrl Pts',(-3.46726929886284,-2.60338928299931,
5.13353417926032));
#17777=CARTESIAN_POINT('Ctrl Pts',(-3.69889136100131,-2.62181906697108,
5.12242039020351));
#17778=CARTESIAN_POINT('Ctrl Pts',(-3.83999669992028,-2.43721935741029,
5.1113066011467));
#17779=CARTESIAN_POINT('Ctrl Pts',(-3.76143050694799,-2.21855034327406,
5.10019281208991));
#17780=CARTESIAN_POINT('Ctrl Pts',(-3.53510505567384,-2.16596525884485,
5.0890790230331));
#17781=CARTESIAN_POINT('Ctrl Pts',(-3.36817872512274,-2.32759432716241,
5.07796523397629));
#17782=CARTESIAN_POINT('Ctrl Pts',(-3.41344101541272,-2.5554973786501,5.06685144491949));
#17783=CARTESIAN_POINT('Ctrl Pts',(-3.62946287054873,-2.64107179130501,
5.05573765586269));
#17784=CARTESIAN_POINT('Ctrl Pts',(-3.81851702088083,-2.50599052171118,
5.04462386680588));
#17785=CARTESIAN_POINT('Ctrl Pts',(-3.8075600664755,-2.27389489448153,5.03351007774907));
#17786=CARTESIAN_POINT('Ctrl Pts',(-3.60662102802227,-2.15722471599323,
5.02239628869228));
#17787=CARTESIAN_POINT('Ctrl Pts',(-3.39962168818772,-2.262769500459,5.01128249963546));
#17788=CARTESIAN_POINT('Ctrl Pts',(-3.37603088927244,-2.49392292132789,
5.00016871057867));
#17789=CARTESIAN_POINT('Ctrl Pts',(-3.55744155755193,-2.63910762521254,
4.98905492152185));
#17790=CARTESIAN_POINT('Ctrl Pts',(-3.77780645076812,-2.56543440904132,
4.97794113246506));
#17791=CARTESIAN_POINT('Ctrl Pts',(-3.83542308317469,-2.34033720163832,
4.96682734340825));
#17792=CARTESIAN_POINT('Ctrl Pts',(-3.67755429765177,-2.16985003043886,
4.95571355435145));
#17793=CARTESIAN_POINT('Ctrl Pts',(-3.44869918397279,-2.21002173633656,
4.94459976529464));
#17794=CARTESIAN_POINT('Ctrl Pts',(-3.3583314230664,-2.42408270152555,4.93348597623784));
#17795=CARTESIAN_POINT('Ctrl Pts',(-3.48916565133794,-2.61610049686178,
4.92237218718103));
#17796=CARTESIAN_POINT('Ctrl Pts',(-3.7214478158856,-2.61031905668909,4.91125839812423));
#17797=CARTESIAN_POINT('Ctrl Pts',(-3.8425674172419,-2.41203019874106,4.90014460906743));
#17798=CARTESIAN_POINT('Ctrl Pts',(-3.74166231069475,-2.20272996345734,
4.88903082001062));
#17799=CARTESIAN_POINT('Ctrl Pts',(-3.511092084609,-2.17399322981363,4.87791703095382));
#17800=CARTESIAN_POINT('Ctrl Pts',(-3.36190028176488,-2.35212305601353,
4.86680324189701));
#17801=CARTESIAN_POINT('Ctrl Pts',(-3.43064385125587,-2.57407519200526,
4.85568945284021));
#17802=CARTESIAN_POINT('Ctrl Pts',(-3.6544010243217,-2.63669433060785,4.84457566378341));
#17803=CARTESIAN_POINT('Ctrl Pts',(-3.82836432287631,-2.48266446410869,
4.8334618747266));
#17804=CARTESIAN_POINT('Ctrl Pts',(-3.79330316687467,-2.25297087613211,
4.8223480856698));
#17805=CARTESIAN_POINT('Ctrl Pts',(-3.58130943002562,-2.15785471265546,
4.81123429661298));
#17806=CARTESIAN_POINT('Ctrl Pts',(-3.38642338383962,-2.28437687679961,
4.8001205075562));
#17807=CARTESIAN_POINT('Ctrl Pts',(-3.38702643654876,-2.51673019686447,
4.78900671849938));
#17808=CARTESIAN_POINT('Ctrl Pts',(-3.58256660716932,-2.64223904392882,
4.77789292944258));
#17809=CARTESIAN_POINT('Ctrl Pts',(-3.79406375995591,-2.54602374690751,
4.76677914038577));
#17810=CARTESIAN_POINT('Ctrl Pts',(-3.82793215242214,-2.31615125831984,
4.75566535132897));
#17811=CARTESIAN_POINT('Ctrl Pts',(-3.65317166084996,-2.16302647390142,
4.74455156227217));
#17812=CARTESIAN_POINT('Ctrl Pts',(-3.42974254509416,-2.22680624538361,
4.73343777321536));
#17813=CARTESIAN_POINT('Ctrl Pts',(-3.36215200866455,-2.44911222461694,
4.72232398415856));
#17814=CARTESIAN_POINT('Ctrl Pts',(-3.51226643608395,-2.62646522768789,
4.71121019510176));
#17815=CARTESIAN_POINT('Ctrl Pts',(-3.74268438952201,-2.59653203956573,
4.70009640604495));
#17816=CARTESIAN_POINT('Ctrl Pts',(-3.84250170307953,-2.38671084680417,
4.68898261698815));
#17817=CARTESIAN_POINT('Ctrl Pts',(-3.72035445765201,-2.18905336667194,
4.67786882793134));
#17818=CARTESIAN_POINT('Ctrl Pts',(-3.4880454122232,-2.18447773232253,4.66675503887454));
#17819=CARTESIAN_POINT('Ctrl Pts',(-3.35820967063793,-2.37717207376684,
4.65564124981773));
#17820=CARTESIAN_POINT('Ctrl Pts',(-3.4496873596065,-2.5907610749791,4.64452746076093));
#17821=CARTESIAN_POINT('Ctrl Pts',(-3.67874791298872,-2.62974430088435,
4.63341367170412));
#17822=CARTESIAN_POINT('Ctrl Pts',(-3.83572960854991,-2.4584399627144,4.62229988264733));
#17823=CARTESIAN_POINT('Ctrl Pts',(-3.77694532005055,-2.23364486391404,
4.61118609359051));
#17824=CARTESIAN_POINT('Ctrl Pts',(-3.55620097341096,-2.16111650777606,
4.60007230453371));
#17825=CARTESIAN_POINT('Ctrl Pts',(-3.37554637252617,-2.307240921179,4.58895851547691));
#17826=CARTESIAN_POINT('Ctrl Pts',(-3.40033672233922,-2.53826877141577,
4.57784472642011));
#17827=CARTESIAN_POINT('Ctrl Pts',(-3.60788113454322,-2.64273764704216,
4.5667309373633));
#17828=CARTESIAN_POINT('Ctrl Pts',(-3.8082118548967,-2.52502600161686,4.5556171483065));
#17829=CARTESIAN_POINT('Ctrl Pts',(-3.8179639032302,-2.29287663878378,4.54450335924969));
#17830=CARTESIAN_POINT('Ctrl Pts',(-3.62821111895818,-2.15877850380716,
4.53338957019289));
#17831=CARTESIAN_POINT('Ctrl Pts',(-3.4126363777684,-2.24547313898512,4.52227578113608));
#17832=CARTESIAN_POINT('Ctrl Pts',(-3.3685576844537,-2.47360796440317,4.51116199207928));
#17833=CARTESIAN_POINT('Ctrl Pts',(-3.53632076809686,-2.63436858142862,
4.50004820302248));
#17834=CARTESIAN_POINT('Ctrl Pts',(-3.76237017326276,-2.5806089855676,4.48893441396567));
#17835=CARTESIAN_POINT('Ctrl Pts',(-3.83980032066171,-2.36153592172191,
4.47782062490887));
#17836=CARTESIAN_POINT('Ctrl Pts',(-3.69773850858379,-2.17766949547173,
4.46670683585206));
#17837=CARTESIAN_POINT('Ctrl Pts',(-3.46621554409366,-2.19730464027232,
4.45559304679525));
#17838=CARTESIAN_POINT('Ctrl Pts',(-3.35714698343348,-2.40246926898597,
4.44447925773846));
#17839=CARTESIAN_POINT('Ctrl Pts',(-3.47036459479899,-2.60537350263611,
4.43336546868164));
#17840=CARTESIAN_POINT('Ctrl Pts',(-3.70223885894321,-2.62029753112878,
4.42225167962485));
#17841=CARTESIAN_POINT('Ctrl Pts',(-3.84053294381125,-2.43357974806573,
4.41113789056804));
#17842=CARTESIAN_POINT('Ctrl Pts',(-3.75866408131995,-2.21612800906199,
4.40002410151124));
#17843=CARTESIAN_POINT('Ctrl Pts',(-3.53156901893564,-2.16697244735031,
4.38891031245443));
#17844=CARTESIAN_POINT('Ctrl Pts',(-3.36710794136624,-2.33111753922242,
4.37779652339762));
#17845=CARTESIAN_POINT('Ctrl Pts',(-3.41581894666805,-2.55829572590735,
4.36668273434083));
#17846=CARTESIAN_POINT('Ctrl Pts',(-3.63310626972243,-2.64061568298545,
4.35556894528402));
#17847=CARTESIAN_POINT('Ctrl Pts',(-3.82010444677879,-2.50263400904229,
4.34445515622722));
#17848=CARTESIAN_POINT('Ctrl Pts',(-3.80561164731632,-2.27083721711559,
4.33334136717041));
#17849=CARTESIAN_POINT('Ctrl Pts',(-3.60297473301061,-2.15700944143379,
4.32222757811361));
#17850=CARTESIAN_POINT('Ctrl Pts',(-3.39749761512046,-2.26611614077921,
4.3111137890568));
#17851=CARTESIAN_POINT('Ctrl Pts',(-3.38436282049399,-2.419721374356,4.30370459635227));
#17852=CARTESIAN_POINT('Ctrl Pts',(-3.41173724903364,-2.48232321801035,
4.3));
#17853=CARTESIAN_POINT('Ctrl Pts',(-3.47309291201476,-2.29206413469515,
5.2));
#17854=CARTESIAN_POINT('Ctrl Pts',(-3.46488110023315,-2.2997248835417,5.2));
#17855=CARTESIAN_POINT('Ctrl Pts',(-3.45756393061001,-2.3082260406838,5.2));
#17856=CARTESIAN_POINT('Ctrl Pts',(-3.45114583189458,-2.31737340047652,
5.2));
#17857=CARTESIAN_POINT('Ctrl Pts',(-3.44637506584917,-2.32417290846779,
5.2));
#17858=CARTESIAN_POINT('Ctrl Pts',(-3.44210141208336,-2.33133076253531,
5.2));
#17859=CARTESIAN_POINT('Ctrl Pts',(-3.43833687158849,-2.33878162457801,
5.2));
#17860=CARTESIAN_POINT('Ctrl Pts',(-3.43611957198332,-2.34317015313494,
5.2));
#17861=CARTESIAN_POINT('Ctrl Pts',(-3.43407750155671,-2.34766554493455,
5.2));
#17862=CARTESIAN_POINT('Ctrl Pts',(-3.43222557143088,-2.35222601439271,
5.2));
#17863=CARTESIAN_POINT('Ctrl Pts',(-3.42766723914997,-2.36345113290954,
5.2));
#17864=CARTESIAN_POINT('Ctrl Pts',(-3.42424191788099,-2.37509439510727,
5.2));
#17865=CARTESIAN_POINT('Ctrl Pts',(-3.42197769676804,-2.38695730471617,
5.2));
#17866=CARTESIAN_POINT('Ctrl Pts',(-3.42053881602809,-2.39449601728207,
5.2));
#17867=CARTESIAN_POINT('Ctrl Pts',(-3.41956956713255,-2.40212431376417,
5.2));
#17868=CARTESIAN_POINT('Ctrl Pts',(-3.41908672349853,-2.40979637190619,
5.2));
#17869=CARTESIAN_POINT('Ctrl Pts',(-3.4188613967758,-2.41337666083611,5.2));
#17870=CARTESIAN_POINT('Ctrl Pts',(-3.41874254028701,-2.41696303084227,
5.2));
#17871=CARTESIAN_POINT('Ctrl Pts',(-3.4187313001846,-2.42054068183377,5.2));
#17872=CARTESIAN_POINT('Ctrl Pts',(-3.41869625236243,-2.43169617411961,
5.2));
#17873=CARTESIAN_POINT('Ctrl Pts',(-3.41970314531555,-2.44279404991157,
5.2));
#17874=CARTESIAN_POINT('Ctrl Pts',(-3.4217856982914,-2.45369315923086,5.2));
#17875=CARTESIAN_POINT('Ctrl Pts',(-3.42294608022389,-2.45976605614203,
5.2));
#17876=CARTESIAN_POINT('Ctrl Pts',(-3.42444095669484,-2.46577748192705,
5.2));
#17877=CARTESIAN_POINT('Ctrl Pts',(-3.42625159798616,-2.47171129566944,
5.2));
#17878=CARTESIAN_POINT('Ctrl Pts',(-3.42738424188737,-2.4754231838156,5.2));
#17879=CARTESIAN_POINT('Ctrl Pts',(-3.4286411006463,-2.47910621955531,5.2));
#17880=CARTESIAN_POINT('Ctrl Pts',(-3.43001647345192,-2.48275158788973,
5.2));
#17881=CARTESIAN_POINT('Ctrl Pts',(-3.43439826051469,-2.49436533198986,
5.2));
#17882=CARTESIAN_POINT('Ctrl Pts',(-3.43994736167241,-2.50551615790537,
5.2));
#17883=CARTESIAN_POINT('Ctrl Pts',(-3.44649835855225,-2.51608152365555,
5.2));
#17884=CARTESIAN_POINT('Ctrl Pts',(-3.45083933347942,-2.52308259366964,
5.2));
#17885=CARTESIAN_POINT('Ctrl Pts',(-3.45562142913928,-2.5298267361278,5.2));
#17886=CARTESIAN_POINT('Ctrl Pts',(-3.46080806253422,-2.53627607801171,
5.2));
#17887=CARTESIAN_POINT('Ctrl Pts',(-3.46351819008795,-2.53964599792162,
5.2));
#17888=CARTESIAN_POINT('Ctrl Pts',(-3.46634016652161,-2.54293674743321,
5.2));
#17889=CARTESIAN_POINT('Ctrl Pts',(-3.46926561316249,-2.5461381198978,5.2));
#17890=CARTESIAN_POINT('Ctrl Pts',(-3.47553204021621,-2.55299559141714,
5.2));
#17891=CARTESIAN_POINT('Ctrl Pts',(-3.48224800724127,-2.55941730873493,
5.2));
#17892=CARTESIAN_POINT('Ctrl Pts',(-3.48935943070669,-2.56535251864156,
5.2));
#17893=CARTESIAN_POINT('Ctrl Pts',(-3.49388595591638,-2.56913036669094,
5.2));
#17894=CARTESIAN_POINT('Ctrl Pts',(-3.49857295100653,-2.57271103243443,
5.2));
#17895=CARTESIAN_POINT('Ctrl Pts',(-3.50340866428261,-2.5760800097667,5.2));
#17896=CARTESIAN_POINT('Ctrl Pts',(-3.50748115648314,-2.57891726109367,
5.2));
#17897=CARTESIAN_POINT('Ctrl Pts',(-3.51165212725609,-2.58159933242901,
5.2));
#17898=CARTESIAN_POINT('Ctrl Pts',(-3.51591076075252,-2.58411660325874,
5.2));
#17899=CARTESIAN_POINT('Ctrl Pts',(-3.52463384142318,-2.58927280102407,
5.2));
#17900=CARTESIAN_POINT('Ctrl Pts',(-3.53372795938425,-2.593741186929,5.2));
#17901=CARTESIAN_POINT('Ctrl Pts',(-3.54313434616876,-2.59744798259885,
5.2));
#17902=CARTESIAN_POINT('Ctrl Pts',(-3.54437365456163,-2.59793635960157,
5.2));
#17903=CARTESIAN_POINT('Ctrl Pts',(-3.54561839868079,-2.59841149645932,
5.2));
#17904=CARTESIAN_POINT('Ctrl Pts',(-3.54686838721289,-2.59887345127292,
5.2));
#17905=CARTESIAN_POINT('Ctrl Pts',(-3.76673281282141,-2.40013003219325,
5.08714803633902));
#17906=CARTESIAN_POINT('Ctrl Pts',(-3.76680596527292,-2.4086546123928,5.08771939403667));
#17907=CARTESIAN_POINT('Ctrl Pts',(-3.76620865763489,-2.417168907206,5.08829075173431));
#17908=CARTESIAN_POINT('Ctrl Pts',(-3.76490523910227,-2.42557368984471,
5.08886210943196));
#17909=CARTESIAN_POINT('Ctrl Pts',(-3.75645407171393,-2.48006902128643,
5.09256670578423));
#17910=CARTESIAN_POINT('Ctrl Pts',(-3.71831780296444,-2.52996042999443,
5.09627130213649));
#17911=CARTESIAN_POINT('Ctrl Pts',(-3.66794964380788,-2.55241564320215,
5.09997589848876));
#17912=CARTESIAN_POINT('Ctrl Pts',(-3.61758148465131,-2.57487085640986,
5.10368049484103));
#17913=CARTESIAN_POINT('Ctrl Pts',(-3.55498143508767,-2.56988987411729,
5.1073850911933));
#17914=CARTESIAN_POINT('Ctrl Pts',(-3.50879890030286,-2.53975064250981,
5.11108968754557));
#17915=CARTESIAN_POINT('Ctrl Pts',(-3.46261636551805,-2.50961141090233,
5.11479428389784));
#17916=CARTESIAN_POINT('Ctrl Pts',(-3.43285134551208,-2.45431392997993,
5.1184988802501));
#17917=CARTESIAN_POINT('Ctrl Pts',(-3.4331256950702,-2.3991686665445,5.12220347660237));
#17918=CARTESIAN_POINT('Ctrl Pts',(-3.43340004462832,-2.34402340310906,
5.12590807295464));
#17919=CARTESIAN_POINT('Ctrl Pts',(-3.46371376375052,-2.28903035716059,
5.12961266930691));
#17920=CARTESIAN_POINT('Ctrl Pts',(-3.51019415842152,-2.25935087796534,
5.13331726565918));
#17921=CARTESIAN_POINT('Ctrl Pts',(-3.55667455309252,-2.22967139877009,
5.13702186201145));
#17922=CARTESIAN_POINT('Ctrl Pts',(-3.61932162331232,-2.22530548632806,
5.14072645836371));
#17923=CARTESIAN_POINT('Ctrl Pts',(-3.66946347831689,-2.24826430176485,
5.14443105471598));
#17924=CARTESIAN_POINT('Ctrl Pts',(-3.71960533332146,-2.27122311720164,
5.14813565106825));
#17925=CARTESIAN_POINT('Ctrl Pts',(-3.7572419731108,-2.32150666051725,5.15184024742051));
#17926=CARTESIAN_POINT('Ctrl Pts',(-3.76515098200617,-2.37607618706626,
5.15554484377278));
#17927=CARTESIAN_POINT('Ctrl Pts',(-3.76629187681735,-2.3839479811825,5.15607924129486));
#17928=CARTESIAN_POINT('Ctrl Pts',(-3.7668141752375,-2.39190896147606,5.15661363881694));
#17929=CARTESIAN_POINT('Ctrl Pts',(-3.76674783764939,-2.3998784327954,5.15714803633902));
#17930=CARTESIAN_POINT('Ctrl Pts',(-3.65301702171886,-2.59851743256717,
5.2));
#17931=CARTESIAN_POINT('Ctrl Pts',(-3.71902879097456,-2.58088801151799,
5.19629540364773));
#17932=CARTESIAN_POINT('Ctrl Pts',(-3.83093278328674,-2.47484748886485,
5.1888862109432));
#17933=CARTESIAN_POINT('Ctrl Pts',(-3.78812295700318,-2.24617213689742,
5.17777242188639));
#17934=CARTESIAN_POINT('Ctrl Pts',(-3.5727867642971,-2.15871465280967,5.16665863282959));
#17935=CARTESIAN_POINT('Ctrl Pts',(-3.38252461999799,-2.29190667528476,
5.15554484377278));
#17936=CARTESIAN_POINT('Ctrl Pts',(-3.39123766053156,-2.52413789941101,
5.14443105471598));
#17937=CARTESIAN_POINT('Ctrl Pts',(-3.59107442597796,-2.64269432067786,
5.13331726565918));
#17938=CARTESIAN_POINT('Ctrl Pts',(-3.79906030223171,-2.53913483234337,
5.12220347660237));
#17939=CARTESIAN_POINT('Ctrl Pts',(-3.82485429799751,-2.30821119218956,
5.11108968754557));
#17940=CARTESIAN_POINT('Ctrl Pts',(-3.64483147519039,-2.16130911215383,
5.09997589848876));
#17941=CARTESIAN_POINT('Ctrl Pts',(-3.42377645640768,-2.23288040078699,
5.08886210943196));
#17942=CARTESIAN_POINT('Ctrl Pts',(-3.36401956629289,-2.45741970591997,
5.07774832037515));
#17943=CARTESIAN_POINT('Ctrl Pts',(-3.52025888222192,-2.62940132794335,
5.06663453131835));
#17944=CARTESIAN_POINT('Ctrl Pts',(-3.74948582853024,-2.5914096999913,5.05552074226155));
#17945=CARTESIAN_POINT('Ctrl Pts',(-3.84188686003135,-2.37821840959849,
5.04440695320474));
#17946=CARTESIAN_POINT('Ctrl Pts',(-3.71288602579316,-2.18496415245566,
5.03329316414794));
#17947=CARTESIAN_POINT('Ctrl Pts',(-3.4805593716682,-2.1885345970333,5.02217937509112));
#17948=CARTESIAN_POINT('Ctrl Pts',(-3.35755805936012,-2.38566174720256,
5.01106558603434));
#17949=CARTESIAN_POINT('Ctrl Pts',(-3.45646661470834,-2.59591285074103,
4.99995179697752));
#17950=CARTESIAN_POINT('Ctrl Pts',(-3.68675290044432,-2.62684270619768,
4.98883800792072));
#17951=CARTESIAN_POINT('Ctrl Pts',(-3.83763327503031,-2.45014085710183,
4.97772421886392));
#17952=CARTESIAN_POINT('Ctrl Pts',(-3.77100521680217,-2.22754451436212,
4.96661042980711));
#17953=CARTESIAN_POINT('Ctrl Pts',(-3.54785414492032,-2.16279863265717,
4.9554966407503));
#17954=CARTESIAN_POINT('Ctrl Pts',(-3.37243276525931,-2.31516585290104,
4.94438285169351));
#17955=CARTESIAN_POINT('Ctrl Pts',(-3.40530625649813,-2.54518272988275,
4.9332690626367));
#17956=CARTESIAN_POINT('Ctrl Pts',(-3.61638513906469,-2.64231220781178,
4.9221552735799));
#17957=CARTESIAN_POINT('Ctrl Pts',(-3.81246651806354,-2.51765057387683,
4.91104148452309));
#17958=CARTESIAN_POINT('Ctrl Pts',(-3.81407488352551,-2.2853020354474,4.89992769546629));
#17959=CARTESIAN_POINT('Ctrl Pts',(-3.61973808033182,-2.15793784472475,
4.88881390640949));
#17960=CARTESIAN_POINT('Ctrl Pts',(-3.4073347883606,-2.25213588990288,4.87770011735268));
#17961=CARTESIAN_POINT('Ctrl Pts',(-3.37128014957741,-2.48167563194308,
4.86658632829587));
#17962=CARTESIAN_POINT('Ctrl Pts',(-3.54457538374435,-2.63645674180255,
4.85547253923907));
#17963=CARTESIAN_POINT('Ctrl Pts',(-3.76860139772859,-2.57480631428759,
4.84435875018227));
#17964=CARTESIAN_POINT('Ctrl Pts',(-3.83830464030165,-2.35315368486712,
4.83324496112546));
#17965=CARTESIAN_POINT('Ctrl Pts',(-3.68988494304833,-2.17438001896094,
4.82213117206866));
#17966=CARTESIAN_POINT('Ctrl Pts',(-3.45919253805822,-2.20211888040452,
4.81101738301185));
#17967=CARTESIAN_POINT('Ctrl Pts',(-3.35738279984868,-2.41098057473832,
4.79990359395505));
#17968=CARTESIAN_POINT('Ctrl Pts',(-3.47764333640382,-2.60979162448597,
4.78878980489824));
#17969=CARTESIAN_POINT('Ctrl Pts',(-3.7098983147675,-2.61657802114276,4.77767601584144));
#17970=CARTESIAN_POINT('Ctrl Pts',(-3.84156211929281,-2.42512809888577,
4.76656222678463));
#17971=CARTESIAN_POINT('Ctrl Pts',(-3.75212137652867,-2.21067814274661,
4.75544843772783));
#17972=CARTESIAN_POINT('Ctrl Pts',(-3.52344221265408,-2.16951662960737,
4.74433464867103));
#17973=CARTESIAN_POINT('Ctrl Pts',(-3.36483725976158,-2.33931915924769,
4.73322085961422));
#17974=CARTESIAN_POINT('Ctrl Pts',(-3.42147942993616,-2.56466355059616,
4.72210707055742));
#17975=CARTESIAN_POINT('Ctrl Pts',(-3.64152350245114,-2.63928952667227,
4.71099328150061));
#17976=CARTESIAN_POINT('Ctrl Pts',(-3.82356064226404,-2.49489108525746,
4.69987949244381));
#17977=CARTESIAN_POINT('Ctrl Pts',(-3.80097019086255,-2.26363775736839,
4.688765703387));
#17978=CARTESIAN_POINT('Ctrl Pts',(-3.59442944460758,-2.15719833661306,
4.6776519143302));
#17979=CARTESIAN_POINT('Ctrl Pts',(-3.3929874908777,-2.27299803191391,4.6665381252734));
#17980=CARTESIAN_POINT('Ctrl Pts',(-3.38102643442896,-2.50504406890429,
4.65542433621659));
#17981=CARTESIAN_POINT('Ctrl Pts',(-3.5694943658766,-2.64094207834572,4.64431054715979));
#17982=CARTESIAN_POINT('Ctrl Pts',(-3.78588445019465,-2.55630307100846,
4.63319675810299));
#17983=CARTESIAN_POINT('Ctrl Pts',(-3.83213238917682,-2.32859809017945,
4.62208296904618));
#17984=CARTESIAN_POINT('Ctrl Pts',(-3.66590691978443,-2.16624808716256,
4.61096917998938));
#17985=CARTESIAN_POINT('Ctrl Pts',(-3.4393560992794,-2.21785386089149,4.59985539093257));
#17986=CARTESIAN_POINT('Ctrl Pts',(-3.35984446292695,-2.43618006142673,
4.58874160187577));
#17987=CARTESIAN_POINT('Ctrl Pts',(-3.50014991321196,-2.62139024142312,
4.57762781281897));
#17988=CARTESIAN_POINT('Ctrl Pts',(-3.73184928030013,-2.60395942271916,
4.56651402376216));
#17989=CARTESIAN_POINT('Ctrl Pts',(-3.84286550587893,-2.3998422313225,4.55540023470536));
#17990=CARTESIAN_POINT('Ctrl Pts',(-3.73158417960078,-2.19586944742698,
4.54428644564855));
#17991=CARTESIAN_POINT('Ctrl Pts',(-3.49986236155564,-2.17873967321655,
4.53317265659175));
#17992=CARTESIAN_POINT('Ctrl Pts',(-3.35979765944108,-2.36413198553984,
4.52205886753494));
#17993=CARTESIAN_POINT('Ctrl Pts',(-3.43959288407154,-2.58235469793693,
4.51094507847814));
#17994=CARTESIAN_POINT('Ctrl Pts',(-3.66621056034765,-2.6336660879353,4.49983128942134));
#17995=CARTESIAN_POINT('Ctrl Pts',(-3.83222496126862,-2.47110025635944,
4.48871750036453));
#17996=CARTESIAN_POINT('Ctrl Pts',(-3.78568121870704,-2.24345555647604,
4.47760371130773));
#17997=CARTESIAN_POINT('Ctrl Pts',(-3.56918135654791,-2.15909775573836,
4.46648992225092));
#17998=CARTESIAN_POINT('Ctrl Pts',(-3.38089013692747,-2.29524052189659,
4.45537613319412));
#17999=CARTESIAN_POINT('Ctrl Pts',(-3.39315268252002,-2.52727080497827,
4.44426234413731));
#18000=CARTESIAN_POINT('Ctrl Pts',(-3.59474487821944,-2.64280871984201,
4.43314855508051));
#18001=CARTESIAN_POINT('Ctrl Pts',(-3.80114723737323,-2.53610097383652,
4.42203476602371));
#18002=CARTESIAN_POINT('Ctrl Pts',(-3.82343706699101,-2.30481863511631,
4.4109209769669));
#18003=CARTESIAN_POINT('Ctrl Pts',(-3.64121277969171,-2.16065653443092,
4.3998071879101));
#18004=CARTESIAN_POINT('Ctrl Pts',(-3.42126523797479,-2.23556891230323,
4.38869339885329));
#18005=CARTESIAN_POINT('Ctrl Pts',(-3.36491711226222,-2.46098554747977,
4.37757960979649));
#18006=CARTESIAN_POINT('Ctrl Pts',(-3.52374009350676,-2.63058418685777,
4.36646582073969));
#18007=CARTESIAN_POINT('Ctrl Pts',(-3.7523704915333,-2.58912096342209,4.35535203168288));
#18008=CARTESIAN_POINT('Ctrl Pts',(-3.84152271736619,-2.3745642740037,4.34423824262608));
#18009=CARTESIAN_POINT('Ctrl Pts',(-3.70962995644976,-2.18326697275372,
4.33312445356927));
#18010=CARTESIAN_POINT('Ctrl Pts',(-3.47734459894833,-2.19039236572141,
4.32201066451247));
#18011=CARTESIAN_POINT('Ctrl Pts',(-3.35742142491826,-2.38928487622609,
4.31089687545566));
#18012=CARTESIAN_POINT('Ctrl Pts',(-3.45934320255763,-2.59816388104693,
4.29978308639886));
#18013=CARTESIAN_POINT('Ctrl Pts',(-3.69040341475663,-2.62529829024268,
4.28866929734205));
#18014=CARTESIAN_POINT('Ctrl Pts',(-3.7885754343637,-2.50643134569448,4.28126010463752));
#18015=CARTESIAN_POINT('Ctrl Pts',(-3.80166758614466,-2.43937207542898,
4.27755550828525));
#18016=CARTESIAN_POINT('Ctrl Pts',(-3.64967348970877,-2.58599788000028,
5.20748149723825));
#18017=CARTESIAN_POINT('Ctrl Pts',(-3.71152220988337,-2.5694802628904,5.20377690088598));
#18018=CARTESIAN_POINT('Ctrl Pts',(-3.81636894835099,-2.47012721287082,
5.19636770818145));
#18019=CARTESIAN_POINT('Ctrl Pts',(-3.77625893469146,-2.25587333035667,
5.18525391912464));
#18020=CARTESIAN_POINT('Ctrl Pts',(-3.57450297395432,-2.17393137483105,
5.17414013006784));
#18021=CARTESIAN_POINT('Ctrl Pts',(-3.39623976035988,-2.29872360840445,
5.16302634101103));
#18022=CARTESIAN_POINT('Ctrl Pts',(-3.40440331076774,-2.5163091110919,5.15191255195424));
#18023=CARTESIAN_POINT('Ctrl Pts',(-3.59163731958239,-2.62738874138378,
5.14079876289742));
#18024=CARTESIAN_POINT('Ctrl Pts',(-3.78650651345082,-2.53036025862013,
5.12968497384062));
#18025=CARTESIAN_POINT('Ctrl Pts',(-3.81067380428838,-2.31399987678807,
5.11857118478382));
#18026=CARTESIAN_POINT('Ctrl Pts',(-3.64200416676191,-2.17636221393428,
5.10745739572701));
#18027=CARTESIAN_POINT('Ctrl Pts',(-3.43489003917469,-2.24341984097745,
5.09634360667021));
#18028=CARTESIAN_POINT('Ctrl Pts',(-3.37890173259108,-2.45379851750672,
5.08522981761341));
#18029=CARTESIAN_POINT('Ctrl Pts',(-3.52528777617272,-2.61493407462981,
5.07411602855659));
#18030=CARTESIAN_POINT('Ctrl Pts',(-3.74005846658983,-2.57933839839392,
5.0630022394998));
#18031=CARTESIAN_POINT('Ctrl Pts',(-3.82663220344909,-2.37959207115806,
5.05188845044299));
#18032=CARTESIAN_POINT('Ctrl Pts',(-3.7057668397564,-2.19852544308029,5.04077466138619));
#18033=CARTESIAN_POINT('Ctrl Pts',(-3.48809192538747,-2.20187071665909,
5.02966087232937));
#18034=CARTESIAN_POINT('Ctrl Pts',(-3.37284772224266,-2.38656599277582,
5.01854708327259));
#18035=CARTESIAN_POINT('Ctrl Pts',(-3.46551858429622,-2.58355755679196,
5.00743329421577));
#18036=CARTESIAN_POINT('Ctrl Pts',(-3.68128180662955,-2.61253681301776,
4.99631950515897));
#18037=CARTESIAN_POINT('Ctrl Pts',(-3.82264687187209,-2.44697871114761,
4.98520571610216));
#18038=CARTESIAN_POINT('Ctrl Pts',(-3.76022072914644,-2.23842046359223,
4.97409192704536));
#18039=CARTESIAN_POINT('Ctrl Pts',(-3.5511427365839,-2.17775779744681,4.96297813798855));
#18040=CARTESIAN_POINT('Ctrl Pts',(-3.38678435101677,-2.32051594004622,
4.95186434893176));
#18041=CARTESIAN_POINT('Ctrl Pts',(-3.41758466713793,-2.53602674395714,
4.94075055987494));
#18042=CARTESIAN_POINT('Ctrl Pts',(-3.6153518060864,-2.62703072656315,4.92963677081815));
#18043=CARTESIAN_POINT('Ctrl Pts',(-3.79906726285858,-2.51023091039877,
4.91852298176134));
#18044=CARTESIAN_POINT('Ctrl Pts',(-3.80057419634206,-2.29253549186461,
4.90740919270453));
#18045=CARTESIAN_POINT('Ctrl Pts',(-3.61849329325651,-2.17320355634632,
4.89629540364773));
#18046=CARTESIAN_POINT('Ctrl Pts',(-3.41948526912059,-2.26146097775627,
4.88518161459093));
#18047=CARTESIAN_POINT('Ctrl Pts',(-3.38570442533712,-2.47652473736257,
4.87406782553412));
#18048=CARTESIAN_POINT('Ctrl Pts',(-3.54807075131856,-2.62154453701271,
4.86295403647732));
#18049=CARTESIAN_POINT('Ctrl Pts',(-3.75796850753643,-2.56378210944851,
4.85184024742052));
#18050=CARTESIAN_POINT('Ctrl Pts',(-3.82327589732119,-2.35610805969097,
4.84072645836371));
#18051=CARTESIAN_POINT('Ctrl Pts',(-3.68421632616712,-2.18860880066658,
4.8296126693069));
#18052=CARTESIAN_POINT('Ctrl Pts',(-3.46807259659411,-2.2145983037314,4.81849888025011));
#18053=CARTESIAN_POINT('Ctrl Pts',(-3.37268351551706,-2.41028808198908,
4.80738509119329));
#18054=CARTESIAN_POINT('Ctrl Pts',(-3.48535979063151,-2.59656106212739,
4.79627130213649));
#18055=CARTESIAN_POINT('Ctrl Pts',(-3.70296754948933,-2.60291947294643,
4.78515751307969));
#18056=CARTESIAN_POINT('Ctrl Pts',(-3.82632794256814,-2.42354338891427,
4.77404372402288));
#18057=CARTESIAN_POINT('Ctrl Pts',(-3.74252780308088,-2.22261777400868,
4.76292993496608));
#18058=CARTESIAN_POINT('Ctrl Pts',(-3.52827034905847,-2.18405212220422,
4.75181614590928));
#18059=CARTESIAN_POINT('Ctrl Pts',(-3.37966785801241,-2.34314601196173,
4.74070235685247));
#18060=CARTESIAN_POINT('Ctrl Pts',(-3.43273787526403,-2.55427900173875,
4.72958856779567));
#18061=CARTESIAN_POINT('Ctrl Pts',(-3.63890481216799,-2.62419867158141,
4.71847477873886));
#18062=CARTESIAN_POINT('Ctrl Pts',(-3.80946173328402,-2.48890675473974,
4.70736098968206));
#18063=CARTESIAN_POINT('Ctrl Pts',(-3.78829595446756,-2.27223747701361,
4.69624720062526));
#18064=CARTESIAN_POINT('Ctrl Pts',(-3.59478075310558,-2.17251068550248,
4.68513341156845));
#18065=CARTESIAN_POINT('Ctrl Pts',(-3.40604278761636,-2.28100744345521,
4.67401962251164));
#18066=CARTESIAN_POINT('Ctrl Pts',(-3.39483605824625,-2.4984194378808,4.66290583345485));
#18067=CARTESIAN_POINT('Ctrl Pts',(-3.57141821148077,-2.62574700466167,
4.65179204439804));
#18068=CARTESIAN_POINT('Ctrl Pts',(-3.77416159988632,-2.54644577793071,
4.64067825534124));
#18069=CARTESIAN_POINT('Ctrl Pts',(-3.81749290078935,-2.33310106985138,
4.62956446628443));
#18070=CARTESIAN_POINT('Ctrl Pts',(-3.66175048306201,-2.18098971122316,
4.61845067722763));
#18071=CARTESIAN_POINT('Ctrl Pts',(-3.44948714789117,-2.22934095365678,
4.60733688817083));
#18072=CARTESIAN_POINT('Ctrl Pts',(-3.37498993318483,-2.43389835661598,
4.59622309911401));
#18073=CARTESIAN_POINT('Ctrl Pts',(-3.50644698442724,-2.60742820932623,
4.58510931005722));
#18074=CARTESIAN_POINT('Ctrl Pts',(-3.72353417177652,-2.59109666965397,
4.57399552100041));
#18075=CARTESIAN_POINT('Ctrl Pts',(-3.82754913074644,-2.39985218104442,
4.56288173194361));
#18076=CARTESIAN_POINT('Ctrl Pts',(-3.72328578972046,-2.20874299284009,
4.5517679428868));
#18077=CARTESIAN_POINT('Ctrl Pts',(-3.50617756728955,-2.19269351221351,
4.54065415383));
#18078=CARTESIAN_POINT('Ctrl Pts',(-3.37494608137275,-2.36639401102897,
4.52954036477319));
#18079=CARTESIAN_POINT('Ctrl Pts',(-3.44970899978995,-2.57085445235588,
4.51842657571639));
#18080=CARTESIAN_POINT('Ctrl Pts',(-3.66203497445559,-2.61892987644406,
4.50731278665958));
#18081=CARTESIAN_POINT('Ctrl Pts',(-3.81757963479854,-2.46661630054004,
4.49619899760278));
#18082=CARTESIAN_POINT('Ctrl Pts',(-3.77397118524436,-2.2533280717731,4.48508520854598));
#18083=CARTESIAN_POINT('Ctrl Pts',(-3.5711249421653,-2.17429031727573,4.47397141948917));
#18084=CARTESIAN_POINT('Ctrl Pts',(-3.39470835638149,-2.30184720512856,
4.46285763043237));
#18085=CARTESIAN_POINT('Ctrl Pts',(-3.40619756140558,-2.51924443916973,
4.45174384137556));
#18086=CARTESIAN_POINT('Ctrl Pts',(-3.59507629381618,-2.62749592593544,
4.44063005231876));
#18087=CARTESIAN_POINT('Ctrl Pts',(-3.78846183549484,-2.52751773117457,
4.42951626326196));
#18088=CARTESIAN_POINT('Ctrl Pts',(-3.80934595131713,-2.31082127219277,
4.41840247420515));
#18089=CARTESIAN_POINT('Ctrl Pts',(-3.63861368521871,-2.17575079119208,
4.40728868514835));
#18090=CARTESIAN_POINT('Ctrl Pts',(-3.43253719137339,-2.24593880082853,
4.39617489609154));
#18091=CARTESIAN_POINT('Ctrl Pts',(-3.37974267459471,-2.45713947835818,
4.38506110703474));
#18092=CARTESIAN_POINT('Ctrl Pts',(-3.52854944397912,-2.61604233624481,
4.37394731797793));
#18093=CARTESIAN_POINT('Ctrl Pts',(-3.74276120758414,-2.57719400158078,
4.36283352892113));
#18094=CARTESIAN_POINT('Ctrl Pts',(-3.82629102553408,-2.37616838455746,
4.35171973986432));
#18095=CARTESIAN_POINT('Ctrl Pts',(-3.70271611525743,-2.19693529644954,
4.34060595080753));
#18096=CARTESIAN_POINT('Ctrl Pts',(-3.48507989312992,-2.2036113246906,4.32949216175072));
#18097=CARTESIAN_POINT('Ctrl Pts',(-3.37271970468676,-2.38996062824249,
4.31837837269391));
#18098=CARTESIAN_POINT('Ctrl Pts',(-3.4682137593984,-2.58566662529692,4.30726458363711));
#18099=CARTESIAN_POINT('Ctrl Pts',(-3.68470210032476,-2.61108979604925,
4.2961507945803));
#18100=CARTESIAN_POINT('Ctrl Pts',(-3.77668287645173,-2.49971922570604,
4.28874160187577));
#18101=CARTESIAN_POINT('Ctrl Pts',(-3.78894936833816,-2.43688906544025,
4.2850370055235));
#18102=CARTESIAN_POINT('Ctrl Pts',(-3.64632995769868,-2.57347832743338,
5.2149629944765));
#18103=CARTESIAN_POINT('Ctrl Pts',(-3.70401562879218,-2.55807251426281,
5.21125839812423));
#18104=CARTESIAN_POINT('Ctrl Pts',(-3.80180511341523,-2.46540693687679,
5.20384920541969));
#18105=CARTESIAN_POINT('Ctrl Pts',(-3.76439491237975,-2.26557452381591,
5.19273541636289));
#18106=CARTESIAN_POINT('Ctrl Pts',(-3.57621918361154,-2.18914809685241,
5.18162162730608));
#18107=CARTESIAN_POINT('Ctrl Pts',(-3.40995490072177,-2.30554054152415,
5.17050783824929));
#18108=CARTESIAN_POINT('Ctrl Pts',(-3.41756896100391,-2.5084803227728,5.15939404919247));
#18109=CARTESIAN_POINT('Ctrl Pts',(-3.59220021318681,-2.6120831620897,5.14828026013568));
#18110=CARTESIAN_POINT('Ctrl Pts',(-3.77395272466994,-2.52158568489689,
5.13716647107886));
#18111=CARTESIAN_POINT('Ctrl Pts',(-3.79649331057924,-2.31978856138657,
5.12605268202207));
#18112=CARTESIAN_POINT('Ctrl Pts',(-3.63917685833343,-2.19141531571474,
5.11493889296526));
#18113=CARTESIAN_POINT('Ctrl Pts',(-3.44600362194169,-2.25395928116791,
5.10382510390846));
#18114=CARTESIAN_POINT('Ctrl Pts',(-3.39378389888927,-2.45017732909347,
5.09271131485166));
#18115=CARTESIAN_POINT('Ctrl Pts',(-3.53031667012352,-2.60046682131627,
5.08159752579484));
#18116=CARTESIAN_POINT('Ctrl Pts',(-3.73063110464943,-2.56726709679655,
5.07048373673805));
#18117=CARTESIAN_POINT('Ctrl Pts',(-3.81137754686683,-2.38096573271764,
5.05936994768124));
#18118=CARTESIAN_POINT('Ctrl Pts',(-3.69864765371964,-2.21208673370492,
5.04825615862444));
#18119=CARTESIAN_POINT('Ctrl Pts',(-3.49562447910673,-2.21520683628489,
5.03714236956762));
#18120=CARTESIAN_POINT('Ctrl Pts',(-3.38813738512521,-2.38747023834909,
5.02602858051084));
#18121=CARTESIAN_POINT('Ctrl Pts',(-3.47457055388411,-2.57120226284288,
5.01491479145402));
#18122=CARTESIAN_POINT('Ctrl Pts',(-3.67581071281477,-2.59823091983783,
5.00380100239722));
#18123=CARTESIAN_POINT('Ctrl Pts',(-3.80766046871388,-2.44381656519338,
4.99268721334042));
#18124=CARTESIAN_POINT('Ctrl Pts',(-3.74943624149071,-2.24929641282234,
4.9815734242836));
#18125=CARTESIAN_POINT('Ctrl Pts',(-3.55443132824748,-2.19271696223645,
4.97045963522681));
#18126=CARTESIAN_POINT('Ctrl Pts',(-3.40113593677424,-2.32586602719142,
4.95934584617));
#18127=CARTESIAN_POINT('Ctrl Pts',(-3.42986307777772,-2.52687075803154,
4.94823205711319));
#18128=CARTESIAN_POINT('Ctrl Pts',(-3.61431847310812,-2.61174924531453,
4.9371182680564));
#18129=CARTESIAN_POINT('Ctrl Pts',(-3.78566800765362,-2.50281124692072,
4.92600447899958));
#18130=CARTESIAN_POINT('Ctrl Pts',(-3.78707350915862,-2.29976894828182,
4.91489068994279));
#18131=CARTESIAN_POINT('Ctrl Pts',(-3.6172485061812,-2.18846926796789,4.90377690088598));
#18132=CARTESIAN_POINT('Ctrl Pts',(-3.43163574988059,-2.27078606560966,
4.89266311182917));
#18133=CARTESIAN_POINT('Ctrl Pts',(-3.40012870109683,-2.47137384278207,
4.88154932277237));
#18134=CARTESIAN_POINT('Ctrl Pts',(-3.55156611889279,-2.60663233222288,
4.87043553371556));
#18135=CARTESIAN_POINT('Ctrl Pts',(-3.74733561734428,-2.55275790460943,
4.85932174465877));
#18136=CARTESIAN_POINT('Ctrl Pts',(-3.80824715434074,-2.35906243451482,
4.84820795560196));
#18137=CARTESIAN_POINT('Ctrl Pts',(-3.6785477092859,-2.2028375823722,4.83709416654515));
#18138=CARTESIAN_POINT('Ctrl Pts',(-3.47695265513,-2.22707772705829,4.82598037748836));
#18139=CARTESIAN_POINT('Ctrl Pts',(-3.38798423118545,-2.40959558923983,
4.81486658843155));
#18140=CARTESIAN_POINT('Ctrl Pts',(-3.49307624485919,-2.5833304997688,4.80375279937474));
#18141=CARTESIAN_POINT('Ctrl Pts',(-3.69603678421119,-2.5892609247501,4.79263901031794));
#18142=CARTESIAN_POINT('Ctrl Pts',(-3.81109376584347,-2.42195867894277,
4.78152522126113));
#18143=CARTESIAN_POINT('Ctrl Pts',(-3.7329342296331,-2.23455740527076,4.77041143220433));
#18144=CARTESIAN_POINT('Ctrl Pts',(-3.53309848546286,-2.19858761480107,
4.75929764314753));
#18145=CARTESIAN_POINT('Ctrl Pts',(-3.39449845626323,-2.34697286467576,
4.74818385409072));
#18146=CARTESIAN_POINT('Ctrl Pts',(-3.4439963205919,-2.54389445288135,4.73707006503392));
#18147=CARTESIAN_POINT('Ctrl Pts',(-3.63628612188485,-2.60910781649055,
4.72595627597711));
#18148=CARTESIAN_POINT('Ctrl Pts',(-3.79536282430398,-2.48292242422203,
4.71484248692031));
#18149=CARTESIAN_POINT('Ctrl Pts',(-3.77562171807257,-2.28083719665882,
4.7037286978635));
#18150=CARTESIAN_POINT('Ctrl Pts',(-3.59513206160358,-2.18782303439192,
4.6926149088067));
#18151=CARTESIAN_POINT('Ctrl Pts',(-3.41909808435503,-2.28901685499652,
4.6815011197499));
#18152=CARTESIAN_POINT('Ctrl Pts',(-3.40864568206353,-2.49179480685731,
4.67038733069309));
#18153=CARTESIAN_POINT('Ctrl Pts',(-3.57334205708494,-2.61055193097763,
4.65927354163629));
#18154=CARTESIAN_POINT('Ctrl Pts',(-3.76243874957797,-2.53658848485295,
4.64815975257949));
#18155=CARTESIAN_POINT('Ctrl Pts',(-3.80285341240188,-2.33760404952332,
4.63704596352268));
#18156=CARTESIAN_POINT('Ctrl Pts',(-3.65759404633958,-2.19573133528376,
4.62593217446587));
#18157=CARTESIAN_POINT('Ctrl Pts',(-3.45961819650295,-2.24082804642207,
4.61481838540908));
#18158=CARTESIAN_POINT('Ctrl Pts',(-3.39013540344272,-2.43161665180523,
4.60370459635226));
#18159=CARTESIAN_POINT('Ctrl Pts',(-3.51274405564254,-2.59346617722935,
4.59259080729546));
#18160=CARTESIAN_POINT('Ctrl Pts',(-3.71521906325291,-2.57823391658879,
4.58147701823866));
#18161=CARTESIAN_POINT('Ctrl Pts',(-3.81223275561396,-2.39986213076634,
4.57036322918186));
#18162=CARTESIAN_POINT('Ctrl Pts',(-3.71498739984013,-2.2216165382532,4.55924944012505));
#18163=CARTESIAN_POINT('Ctrl Pts',(-3.51249277302345,-2.20664735121048,
4.54813565106825));
#18164=CARTESIAN_POINT('Ctrl Pts',(-3.39009450330442,-2.36865603651811,
4.53702186201144));
#18165=CARTESIAN_POINT('Ctrl Pts',(-3.45982511550835,-2.55935420677483,
4.52590807295464));
#18166=CARTESIAN_POINT('Ctrl Pts',(-3.65785938856352,-2.60419366495283,
4.51479428389783));
#18167=CARTESIAN_POINT('Ctrl Pts',(-3.80293430832847,-2.46213234472064,
4.50368049484103));
#18168=CARTESIAN_POINT('Ctrl Pts',(-3.76226115178167,-2.26320058707017,
4.49256670578422));
#18169=CARTESIAN_POINT('Ctrl Pts',(-3.57306852778269,-2.1894828788131,4.48145291672742));
#18170=CARTESIAN_POINT('Ctrl Pts',(-3.40852657583551,-2.30845388836054,
4.47033912767062));
#18171=CARTESIAN_POINT('Ctrl Pts',(-3.41924244029115,-2.51121807336119,
4.45922533861381));
#18172=CARTESIAN_POINT('Ctrl Pts',(-3.59540770941291,-2.61218313202887,
4.44811154955701));
#18173=CARTESIAN_POINT('Ctrl Pts',(-3.77577643361645,-2.51893448851262,
4.4369977605002));
#18174=CARTESIAN_POINT('Ctrl Pts',(-3.79525483564324,-2.31682390926922,
4.42588397144341));
#18175=CARTESIAN_POINT('Ctrl Pts',(-3.63601459074572,-2.19084504795324,
4.41477018238659));
#18176=CARTESIAN_POINT('Ctrl Pts',(-3.44380914477199,-2.25630868935384,
4.4036563933298));
#18177=CARTESIAN_POINT('Ctrl Pts',(-3.3945682369272,-2.45329340923659,4.39254260427298));
#18178=CARTESIAN_POINT('Ctrl Pts',(-3.53335879445148,-2.60150048563184,
4.38142881521619));
#18179=CARTESIAN_POINT('Ctrl Pts',(-3.73315192363498,-2.56526703973946,
4.37031502615937));
#18180=CARTESIAN_POINT('Ctrl Pts',(-3.81105933370197,-2.37777249511123,
4.35920123710258));
#18181=CARTESIAN_POINT('Ctrl Pts',(-3.69580227406509,-2.21060362014537,
4.34808744804577));
#18182=CARTESIAN_POINT('Ctrl Pts',(-3.49281518731151,-2.21683028365978,
4.33697365898897));
#18183=CARTESIAN_POINT('Ctrl Pts',(-3.38801798445527,-2.3906363802589,4.32585986993216));
#18184=CARTESIAN_POINT('Ctrl Pts',(-3.47708431623917,-2.57316936954691,
4.31474608087536));
#18185=CARTESIAN_POINT('Ctrl Pts',(-3.6790007858929,-2.59688130185582,4.30363229181855));
#18186=CARTESIAN_POINT('Ctrl Pts',(-3.76479031853975,-2.4930071057176,4.29622309911402));
#18187=CARTESIAN_POINT('Ctrl Pts',(-3.77623115053166,-2.43440605545153,
4.29251850276175));
#18188=CARTESIAN_POINT('Ctrl Pts',(-3.64298642568859,-2.56095877486649,
5.22244449171475));
#18189=CARTESIAN_POINT('Ctrl Pts',(-3.69650904770099,-2.54666476563522,
5.21873989536248));
#18190=CARTESIAN_POINT('Ctrl Pts',(-3.78724127847948,-2.46068666088276,
5.21133070265795));
#18191=CARTESIAN_POINT('Ctrl Pts',(-3.75253089006804,-2.27527571727515,
5.20021691360113));
#18192=CARTESIAN_POINT('Ctrl Pts',(-3.57793539326875,-2.20436481887379,
5.18910312454434));
#18193=CARTESIAN_POINT('Ctrl Pts',(-3.42367004108366,-2.31235747464383,
5.17798933548752));
#18194=CARTESIAN_POINT('Ctrl Pts',(-3.43073461124009,-2.5006515344537,5.16687554643073));
#18195=CARTESIAN_POINT('Ctrl Pts',(-3.59276310679123,-2.59677758279563,
5.15576175737392));
#18196=CARTESIAN_POINT('Ctrl Pts',(-3.76139893588905,-2.51281111117365,
5.14464796831712));
#18197=CARTESIAN_POINT('Ctrl Pts',(-3.78231281687012,-2.32557724598507,
5.13353417926031));
#18198=CARTESIAN_POINT('Ctrl Pts',(-3.63634954990495,-2.2064684174952,5.12242039020351));
#18199=CARTESIAN_POINT('Ctrl Pts',(-3.4571172047087,-2.26449872135838,5.1113066011467));
#18200=CARTESIAN_POINT('Ctrl Pts',(-3.40866606518746,-2.44655614068022,
5.10019281208991));
#18201=CARTESIAN_POINT('Ctrl Pts',(-3.53534556407432,-2.58599956800273,
5.08907902303309));
#18202=CARTESIAN_POINT('Ctrl Pts',(-3.72120374270903,-2.55519579519918,
5.0779652339763));
#18203=CARTESIAN_POINT('Ctrl Pts',(-3.79612289028458,-2.3823393942772,5.06685144491949));
#18204=CARTESIAN_POINT('Ctrl Pts',(-3.69152846768288,-2.22564802432955,
5.05573765586268));
#18205=CARTESIAN_POINT('Ctrl Pts',(-3.503157032826,-2.22854295591068,5.04462386680587));
#18206=CARTESIAN_POINT('Ctrl Pts',(-3.40342704800776,-2.38837448392236,
5.03351007774909));
#18207=CARTESIAN_POINT('Ctrl Pts',(-3.483622523472,-2.55884696889381,5.02239628869226));
#18208=CARTESIAN_POINT('Ctrl Pts',(-3.670339619,-2.58392502665791,5.01128249963547));
#18209=CARTESIAN_POINT('Ctrl Pts',(-3.79267406555566,-2.44065441923915,
5.00016871057867));
#18210=CARTESIAN_POINT('Ctrl Pts',(-3.73865175383498,-2.26017236205245,
4.98905492152186));
#18211=CARTESIAN_POINT('Ctrl Pts',(-3.55771991991106,-2.20767612702608,
4.97794113246506));
#18212=CARTESIAN_POINT('Ctrl Pts',(-3.4154875225317,-2.3312161143366,4.96682734340825));
#18213=CARTESIAN_POINT('Ctrl Pts',(-3.44214148841752,-2.51771477210593,
4.95571355435145));
#18214=CARTESIAN_POINT('Ctrl Pts',(-3.61328514012983,-2.59646776406591,
4.94459976529465));
#18215=CARTESIAN_POINT('Ctrl Pts',(-3.77226875244865,-2.49539158344266,
4.93348597623784));
#18216=CARTESIAN_POINT('Ctrl Pts',(-3.77357282197517,-2.30700240469905,
4.92237218718103));
#18217=CARTESIAN_POINT('Ctrl Pts',(-3.61600371910589,-2.20373497958946,
4.91125839812423));
#18218=CARTESIAN_POINT('Ctrl Pts',(-3.44378623064059,-2.28011115346305,
4.90014460906743));
#18219=CARTESIAN_POINT('Ctrl Pts',(-3.41455297685654,-2.46622294820157,
4.88903082001062));
#18220=CARTESIAN_POINT('Ctrl Pts',(-3.555061486467,-2.59172012743304,4.87791703095382));
#18221=CARTESIAN_POINT('Ctrl Pts',(-3.73670272715212,-2.54173369977035,
4.86680324189701));
#18222=CARTESIAN_POINT('Ctrl Pts',(-3.79321841136028,-2.36201680933867,
4.85568945284021));
#18223=CARTESIAN_POINT('Ctrl Pts',(-3.67287909240468,-2.21706636407783,
4.8445756637834));
#18224=CARTESIAN_POINT('Ctrl Pts',(-3.48583271366589,-2.23955715038517,
4.83346187472661));
#18225=CARTESIAN_POINT('Ctrl Pts',(-3.40328494685383,-2.40890309649059,
4.82234808566979));
#18226=CARTESIAN_POINT('Ctrl Pts',(-3.50079269908688,-2.57009993741021,
4.811234296613));
#18227=CARTESIAN_POINT('Ctrl Pts',(-3.68910601893303,-2.57560237655376,
4.80012050755619));
#18228=CARTESIAN_POINT('Ctrl Pts',(-3.79585958911879,-2.42037396897126,
4.78900671849938));
#18229=CARTESIAN_POINT('Ctrl Pts',(-3.72334065618531,-2.24649703653284,
4.77789292944258));
#18230=CARTESIAN_POINT('Ctrl Pts',(-3.53792662186724,-2.21312310739792,
4.76677914038578));
#18231=CARTESIAN_POINT('Ctrl Pts',(-3.40932905451407,-2.35079971738979,
4.75566535132897));
#18232=CARTESIAN_POINT('Ctrl Pts',(-3.45525476591977,-2.53350990402394,
4.74455156227217));
#18233=CARTESIAN_POINT('Ctrl Pts',(-3.6336674316017,-2.59401696139969,4.73343777321536));
#18234=CARTESIAN_POINT('Ctrl Pts',(-3.78126391532395,-2.47693809370431,
4.72232398415856));
#18235=CARTESIAN_POINT('Ctrl Pts',(-3.76294748167758,-2.28943691630404,
4.71121019510175));
#18236=CARTESIAN_POINT('Ctrl Pts',(-3.59548337010158,-2.20313538328135,
4.70009640604495));
#18237=CARTESIAN_POINT('Ctrl Pts',(-3.43215338109369,-2.29702626653782,
4.68898261698815));
#18238=CARTESIAN_POINT('Ctrl Pts',(-3.42245530588083,-2.48517017583382,
4.67786882793134));
#18239=CARTESIAN_POINT('Ctrl Pts',(-3.5752659026891,-2.59535685729358,4.66675503887453));
#18240=CARTESIAN_POINT('Ctrl Pts',(-3.75071589926964,-2.5267311917752,4.65564124981774));
#18241=CARTESIAN_POINT('Ctrl Pts',(-3.7882139240144,-2.34210702919526,4.64452746076093));
#18242=CARTESIAN_POINT('Ctrl Pts',(-3.65343760961716,-2.21047295934436,
4.63341367170412));
#18243=CARTESIAN_POINT('Ctrl Pts',(-3.46974924511472,-2.25231513918736,
4.62229988264733));
#18244=CARTESIAN_POINT('Ctrl Pts',(-3.4052808737006,-2.42933494699449,4.61118609359051));
#18245=CARTESIAN_POINT('Ctrl Pts',(-3.51904112685782,-2.57950414513246,
4.60007230453372));
#18246=CARTESIAN_POINT('Ctrl Pts',(-3.7069039547293,-2.5653711635236,4.5889585154769));
#18247=CARTESIAN_POINT('Ctrl Pts',(-3.79691638048147,-2.39987208048827,
4.57784472642011));
#18248=CARTESIAN_POINT('Ctrl Pts',(-3.7066890099598,-2.23449008366631,4.5667309373633));
#18249=CARTESIAN_POINT('Ctrl Pts',(-3.51880797875736,-2.22060119020745,
4.5556171483065));
#18250=CARTESIAN_POINT('Ctrl Pts',(-3.40524292523608,-2.37091806200724,
4.54450335924969));
#18251=CARTESIAN_POINT('Ctrl Pts',(-3.46994123122676,-2.54785396119378,
4.53338957019289));
#18252=CARTESIAN_POINT('Ctrl Pts',(-3.65368380267146,-2.5894574534616,4.52227578113609));
#18253=CARTESIAN_POINT('Ctrl Pts',(-3.78828898185839,-2.45764838890124,
4.51116199207927));
#18254=CARTESIAN_POINT('Ctrl Pts',(-3.75055111831899,-2.27307310236724,
4.50004820302248));
#18255=CARTESIAN_POINT('Ctrl Pts',(-3.57501211340008,-2.20467544035046,
4.48893441396567));
#18256=CARTESIAN_POINT('Ctrl Pts',(-3.42234479528953,-2.31506057159251,
4.47782062490887));
#18257=CARTESIAN_POINT('Ctrl Pts',(-3.43228731917671,-2.50319170755265,
4.46670683585206));
#18258=CARTESIAN_POINT('Ctrl Pts',(-3.59573912500965,-2.5968703381223,4.45559304679526));
#18259=CARTESIAN_POINT('Ctrl Pts',(-3.76309103173807,-2.51035124585066,
4.44447925773846));
#18260=CARTESIAN_POINT('Ctrl Pts',(-3.78116371996935,-2.32282654634568,
4.43336546868165));
#18261=CARTESIAN_POINT('Ctrl Pts',(-3.63341549627273,-2.20593930471439,
4.42225167962485));
#18262=CARTESIAN_POINT('Ctrl Pts',(-3.45508109817058,-2.26667857787915,
4.41113789056804));
#18263=CARTESIAN_POINT('Ctrl Pts',(-3.40939379925969,-2.449447340115,4.40002410151124));
#18264=CARTESIAN_POINT('Ctrl Pts',(-3.53816814492384,-2.58695863501888,
4.38891031245443));
#18265=CARTESIAN_POINT('Ctrl Pts',(-3.72354263968583,-2.55334007789814,
4.37779652339763));
#18266=CARTESIAN_POINT('Ctrl Pts',(-3.79582764186986,-2.379376605665,4.36668273434082));
#18267=CARTESIAN_POINT('Ctrl Pts',(-3.68888843287276,-2.22427194384119,
4.35556894528402));
#18268=CARTESIAN_POINT('Ctrl Pts',(-3.50055048149309,-2.23004924262897,
4.34445515622722));
#18269=CARTESIAN_POINT('Ctrl Pts',(-3.40331626422378,-2.3913121322753,4.33334136717041));
#18270=CARTESIAN_POINT('Ctrl Pts',(-3.48595487307994,-2.5606721137969,4.32222757811361));
#18271=CARTESIAN_POINT('Ctrl Pts',(-3.67329947146103,-2.58267280766239,
4.3111137890568));
#18272=CARTESIAN_POINT('Ctrl Pts',(-3.75289776062778,-2.48629498572916,
4.30370459635227));
#18273=CARTESIAN_POINT('Ctrl Pts',(-3.76351293272515,-2.4319230454628,4.3));
#18274=CARTESIAN_POINT('Ctrl Pts',(-3.76638442554721,-2.39990578503699,
5.13785196366098));
#18275=CARTESIAN_POINT('Ctrl Pts',(-3.76649613683224,-2.3783172805639,5.13641270219409));
#18276=CARTESIAN_POINT('Ctrl Pts',(-3.76259705167907,-2.35676746354197,
5.1349734407272));
#18277=CARTESIAN_POINT('Ctrl Pts',(-3.75449995887908,-2.33693141876819,
5.13353417926032));
#18278=CARTESIAN_POINT('Ctrl Pts',(-3.73365839454839,-2.28587430315511,
5.12982958290805));
#18279=CARTESIAN_POINT('Ctrl Pts',(-3.68500397222667,-2.24617136032516,
5.12612498655578));
#18280=CARTESIAN_POINT('Ctrl Pts',(-3.6308047035331,-2.23599160622071,5.12242039020351));
#18281=CARTESIAN_POINT('Ctrl Pts',(-3.57660543483953,-2.22581185211626,
5.11871579385124));
#18282=CARTESIAN_POINT('Ctrl Pts',(-3.51686131977411,-2.24515528673732,
5.11501119749897));
#18283=CARTESIAN_POINT('Ctrl Pts',(-3.4789140723212,-2.28516990726816,5.1113066011467));
#18284=CARTESIAN_POINT('Ctrl Pts',(-3.44096682486829,-2.32518452779899,
5.10760200479444));
#18285=CARTESIAN_POINT('Ctrl Pts',(-3.42481644502788,-2.3858703342396,5.10389740844217));
#18286=CARTESIAN_POINT('Ctrl Pts',(-3.43785450492215,-2.43945380868033,
5.1001928120899));
#18287=CARTESIAN_POINT('Ctrl Pts',(-3.45089256481642,-2.49303728312105,
5.09648821573763));
#18288=CARTESIAN_POINT('Ctrl Pts',(-3.49311906444537,-2.53951842556189,
5.09278361938536));
#18289=CARTESIAN_POINT('Ctrl Pts',(-3.54520867736563,-2.55762503464839,
5.08907902303309));
#18290=CARTESIAN_POINT('Ctrl Pts',(-3.59729829028589,-2.57573164373488,
5.08537442668083));
#18291=CARTESIAN_POINT('Ctrl Pts',(-3.65925101649746,-2.56546371946703,
5.08166983032856));
#18292=CARTESIAN_POINT('Ctrl Pts',(-3.70271390419917,-2.53152035717944,
5.07796523397629));
#18293=CARTESIAN_POINT('Ctrl Pts',(-3.74226404589835,-2.50063274572034,
5.07459414387119));
#18294=CARTESIAN_POINT('Ctrl Pts',(-3.76650359324528,-2.4501405807959,5.07122305376609));
#18295=CARTESIAN_POINT('Ctrl Pts',(-3.7668206250807,-2.39991359866148,5.06785196366098));
#18296=CARTESIAN_POINT('Ctrl Pts',(-3.65301702171886,-2.59851743256717,
5.2));
#18297=CARTESIAN_POINT('Ctrl Pts',(-3.66542047324148,-2.59392489431986,
5.2));
#18298=CARTESIAN_POINT('Ctrl Pts',(-3.67726976851323,-2.58806562778896,
5.2));
#18299=CARTESIAN_POINT('Ctrl Pts',(-3.6884471572875,-2.58110287343,5.2));
#18300=CARTESIAN_POINT('Ctrl Pts',(-3.69411332072466,-2.57757323829184,
5.2));
#18301=CARTESIAN_POINT('Ctrl Pts',(-3.69960638117381,-2.57375928297626,
5.2));
#18302=CARTESIAN_POINT('Ctrl Pts',(-3.70490756348411,-2.56967869660782,
5.2));
#18303=CARTESIAN_POINT('Ctrl Pts',(-3.7094943667238,-2.56614800370216,5.2));
#18304=CARTESIAN_POINT('Ctrl Pts',(-3.71393749668481,-2.56241764644412,
5.2));
#18305=CARTESIAN_POINT('Ctrl Pts',(-3.71822298464189,-2.55849819748795,
5.2));
#18306=CARTESIAN_POINT('Ctrl Pts',(-3.7213335990699,-2.55565327187038,5.2));
#18307=CARTESIAN_POINT('Ctrl Pts',(-3.72435497328541,-2.55271413748664,
5.2));
#18308=CARTESIAN_POINT('Ctrl Pts',(-3.72727770073803,-2.54969101779411,
5.2));
#18309=CARTESIAN_POINT('Ctrl Pts',(-3.73622270492435,-2.54043876326685,
5.2));
#18310=CARTESIAN_POINT('Ctrl Pts',(-3.7442634301432,-2.53038665580988,5.2));
#18311=CARTESIAN_POINT('Ctrl Pts',(-3.75126083636282,-2.51966573521934,
5.2));
#18312=CARTESIAN_POINT('Ctrl Pts',(-3.75579169616378,-2.51272387896453,
5.2));
#18313=CARTESIAN_POINT('Ctrl Pts',(-3.75988429343086,-2.5055010355982,5.2));
#18314=CARTESIAN_POINT('Ctrl Pts',(-3.76348914806144,-2.49803012759629,
5.2));
#18315=CARTESIAN_POINT('Ctrl Pts',(-3.76515593070928,-2.49457579140323,
5.2));
#18316=CARTESIAN_POINT('Ctrl Pts',(-3.76671430859645,-2.49107651026494,
5.2));
#18317=CARTESIAN_POINT('Ctrl Pts',(-3.76815914917795,-2.48753923965477,
5.2));
#18318=CARTESIAN_POINT('Ctrl Pts',(-3.77216127817835,-2.47774119447769,
5.2));
#18319=CARTESIAN_POINT('Ctrl Pts',(-3.77529843764987,-2.46764366345261,
5.2));
#18320=CARTESIAN_POINT('Ctrl Pts',(-3.77747651250232,-2.45732003292749,
5.2));
#18321=CARTESIAN_POINT('Ctrl Pts',(-3.779330303747,-2.44853344055707,5.2));
#18322=CARTESIAN_POINT('Ctrl Pts',(-3.78048859875581,-2.43958258054595,
5.2));
#18323=CARTESIAN_POINT('Ctrl Pts',(-3.78096402676373,-2.43054575199388,
5.2));
#18324=CARTESIAN_POINT('Ctrl Pts',(-3.78113316899519,-2.42733073453364,
5.2));
#18325=CARTESIAN_POINT('Ctrl Pts',(-3.78121551844131,-2.4241062749112,5.2));
#18326=CARTESIAN_POINT('Ctrl Pts',(-3.78121200526832,-2.42088560814198,
5.2));
#18327=CARTESIAN_POINT('Ctrl Pts',(-3.78119923320481,-2.40917694458053,
5.2));
#18328=CARTESIAN_POINT('Ctrl Pts',(-3.78005717128054,-2.39748206272171,
5.2));
#18329=CARTESIAN_POINT('Ctrl Pts',(-3.77783120534438,-2.38597327518306,
5.2));
#18330=CARTESIAN_POINT('Ctrl Pts',(-3.77668820057652,-2.38006366137664,
5.2));
#18331=CARTESIAN_POINT('Ctrl Pts',(-3.77525871074905,-2.37420329819383,
5.2));
#18332=CARTESIAN_POINT('Ctrl Pts',(-3.77354495279965,-2.36841778018193,
5.2));
#18333=CARTESIAN_POINT('Ctrl Pts',(-3.771857709037,-2.36272177207139,5.2));
#18334=CARTESIAN_POINT('Ctrl Pts',(-3.76989216970551,-2.35709287385817,
5.2));
#18335=CARTESIAN_POINT('Ctrl Pts',(-3.76766230775392,-2.35158840548752,
5.2));
#18336=CARTESIAN_POINT('Ctrl Pts',(-3.76420558159522,-2.34305539303218,
5.2));
#18337=CARTESIAN_POINT('Ctrl Pts',(-3.76011199819993,-2.33480777321703,
5.2));
#18338=CARTESIAN_POINT('Ctrl Pts',(-3.75539090007917,-2.32694141045687,
5.2));
#18339=CARTESIAN_POINT('Ctrl Pts',(-3.75297689160326,-2.32291915421652,
5.2));
#18340=CARTESIAN_POINT('Ctrl Pts',(-3.75039789394566,-2.31899648610286,
5.2));
#18341=CARTESIAN_POINT('Ctrl Pts',(-3.74766394659108,-2.31519991459367,
5.2));
#18342=CARTESIAN_POINT('Ctrl Pts',(-3.7422293448357,-2.30765300475514,5.2));
#18343=CARTESIAN_POINT('Ctrl Pts',(-3.73617584795258,-2.30058959872182,
5.2));
#18344=CARTESIAN_POINT('Ctrl Pts',(-3.7295081063639,-2.29412082362908,5.2));
#18345=CARTESIAN_POINT('Ctrl Pts',(-3.72872963705521,-2.29336558397147,
5.2));
#18346=CARTESIAN_POINT('Ctrl Pts',(-3.72794278071792,-2.29261847520289,
5.2));
#18347=CARTESIAN_POINT('Ctrl Pts',(-3.72714769448934,-2.29187956305505,
5.2));
#18348=CARTESIAN_POINT('Origin',(-3.6,-2.4,4.7));
#18349=CARTESIAN_POINT('Origin',(3.6,-2.4,4.3));
#18350=CARTESIAN_POINT('Ctrl Pts',(3.43648706727485,-2.43192304546281,4.3));
#18351=CARTESIAN_POINT('Ctrl Pts',(3.43713128683253,-2.44021936733391,4.3));
#18352=CARTESIAN_POINT('Ctrl Pts',(3.43844438912273,-2.44842976439641,4.3));
#18353=CARTESIAN_POINT('Ctrl Pts',(3.44036779101517,-2.45650290183658,4.3));
#18354=CARTESIAN_POINT('Ctrl Pts',(3.44142971550231,-2.46096014104879,4.3));
#18355=CARTESIAN_POINT('Ctrl Pts',(3.44267796071139,-2.46537560589173,4.3));
#18356=CARTESIAN_POINT('Ctrl Pts',(3.44410466214797,-2.4697408265362,4.3));
#18357=CARTESIAN_POINT('Ctrl Pts',(3.44564437628146,-2.47445182755564,4.3));
#18358=CARTESIAN_POINT('Ctrl Pts',(3.44738954450943,-2.47909640503965,4.3));
#18359=CARTESIAN_POINT('Ctrl Pts',(3.44932653760859,-2.48365784749895,4.3));
#18360=CARTESIAN_POINT('Ctrl Pts',(3.45254730792056,-2.49124246845553,4.3));
#18361=CARTESIAN_POINT('Ctrl Pts',(3.45629958145885,-2.49860290469935,4.3));
#18362=CARTESIAN_POINT('Ctrl Pts',(3.460540361967,-2.50569093557372,4.3));
#18363=CARTESIAN_POINT('Ctrl Pts',(3.46239352486579,-2.50878830781843,4.3));
#18364=CARTESIAN_POINT('Ctrl Pts',(3.46433983439221,-2.51183274422802,4.3));
#18365=CARTESIAN_POINT('Ctrl Pts',(3.46636982169588,-2.5148117549636,4.3));
#18366=CARTESIAN_POINT('Ctrl Pts',(3.4732458122516,-2.52490228589753,4.3));
#18367=CARTESIAN_POINT('Ctrl Pts',(3.48109363537456,-2.5342702737356,4.3));
#18368=CARTESIAN_POINT('Ctrl Pts',(3.4897794934809,-2.54276723354547,4.3));
#18369=CARTESIAN_POINT('Ctrl Pts',(3.49400930325249,-2.54690505426423,4.3));
#18370=CARTESIAN_POINT('Ctrl Pts',(3.49843862851918,-2.55083612678489,4.3));
#18371=CARTESIAN_POINT('Ctrl Pts',(3.50305595405548,-2.55454125034048,4.3));
#18372=CARTESIAN_POINT('Ctrl Pts',(3.50696190635494,-2.55767554004086,4.3));
#18373=CARTESIAN_POINT('Ctrl Pts',(3.51100694759131,-2.56065060854479,4.3));
#18374=CARTESIAN_POINT('Ctrl Pts',(3.51515869554757,-2.56343734237232,4.3));
#18375=CARTESIAN_POINT('Ctrl Pts',(3.52023397904373,-2.56684397118314,4.3));
#18376=CARTESIAN_POINT('Ctrl Pts',(3.52547419237578,-2.56997446151731,4.3));
#18377=CARTESIAN_POINT('Ctrl Pts',(3.53086407609141,-2.57281069688687,4.3));
#18378=CARTESIAN_POINT('Ctrl Pts',(3.53843716228638,-2.57679576522158,4.3));
#18379=CARTESIAN_POINT('Ctrl Pts',(3.5463054085634,-2.58020053156405,4.3));
#18380=CARTESIAN_POINT('Ctrl Pts',(3.55440202217605,-2.58304072456499,4.3));
#18381=CARTESIAN_POINT('Ctrl Pts',(3.56031216163472,-2.58511392918216,4.3));
#18382=CARTESIAN_POINT('Ctrl Pts',(3.5663442123363,-2.58688610080112,4.3));
#18383=CARTESIAN_POINT('Ctrl Pts',(3.57247443059928,-2.58835971156752,4.3));
#18384=CARTESIAN_POINT('Ctrl Pts',(3.57600236806727,-2.58920777380822,4.3));
#18385=CARTESIAN_POINT('Ctrl Pts',(3.57955832823423,-2.58995565186198,4.3));
#18386=CARTESIAN_POINT('Ctrl Pts',(3.58312950627136,-2.59060308036101,4.3));
#18387=CARTESIAN_POINT('Ctrl Pts',(3.59464642713376,-2.59269101400921,4.3));
#18388=CARTESIAN_POINT('Ctrl Pts',(3.6063444588111,-2.59374267077427,4.3));
#18389=CARTESIAN_POINT('Ctrl Pts',(3.61806681517941,-2.59379134323091,4.3));
#18390=CARTESIAN_POINT('Ctrl Pts',(3.62473112824741,-2.59381901415975,4.3));
#18391=CARTESIAN_POINT('Ctrl Pts',(3.63140369181744,-2.59352192189353,4.3));
#18392=CARTESIAN_POINT('Ctrl Pts',(3.63805736597901,-2.59290136699938,4.3));
#18393=CARTESIAN_POINT('Ctrl Pts',(3.64215429545284,-2.59251926688834,4.3));
#18394=CARTESIAN_POINT('Ctrl Pts',(3.64624613464129,-2.59201413768455,4.3));
#18395=CARTESIAN_POINT('Ctrl Pts',(3.65032004640889,-2.59138662655135,4.3));
#18396=CARTESIAN_POINT('Ctrl Pts',(3.6635759835922,-2.58934479338508,4.3));
#18397=CARTESIAN_POINT('Ctrl Pts',(3.67655554403262,-2.58602558677096,4.3));
#18398=CARTESIAN_POINT('Ctrl Pts',(3.68904453335804,-2.58146163637399,4.3));
#18399=CARTESIAN_POINT('Ctrl Pts',(3.69937751045428,-2.5776855746214,4.3));
#18400=CARTESIAN_POINT('Ctrl Pts',(3.70937567296629,-2.57305657585047,4.3));
#18401=CARTESIAN_POINT('Ctrl Pts',(3.7189159065364,-2.56756614624894,4.3));
#18402=CARTESIAN_POINT('Ctrl Pts',(3.72007018633274,-2.56690185517936,4.3));
#18403=CARTESIAN_POINT('Ctrl Pts',(3.72121775119647,-2.56622492375,4.3));
#18404=CARTESIAN_POINT('Ctrl Pts',(3.72235852099786,-2.56553552032368,4.3));
#18405=CARTESIAN_POINT('Ctrl Pts',(3.78826275096637,-2.48232321801033,4.3));
#18406=CARTESIAN_POINT('Ctrl Pts',(3.79091867325729,-2.4742706313139,4.3));
#18407=CARTESIAN_POINT('Ctrl Pts',(3.79302804122654,-2.46606039506531,4.3));
#18408=CARTESIAN_POINT('Ctrl Pts',(3.79460324133206,-2.45774386615892,4.3));
#18409=CARTESIAN_POINT('Ctrl Pts',(3.79578956705146,-2.45148046374845,4.3));
#18410=CARTESIAN_POINT('Ctrl Pts',(3.79667272255332,-2.44515671383718,4.3));
#18411=CARTESIAN_POINT('Ctrl Pts',(3.79725488779627,-2.43879482378833,4.3));
#18412=CARTESIAN_POINT('Ctrl Pts',(3.79769087373759,-2.43403037820329,4.3));
#18413=CARTESIAN_POINT('Ctrl Pts',(3.79795758751143,-2.42924591021267,4.3));
#18414=CARTESIAN_POINT('Ctrl Pts',(3.79805591662036,-2.4244630110418,4.3));
#18415=CARTESIAN_POINT('Ctrl Pts',(3.79826160078478,-2.41445817493456,4.3));
#18416=CARTESIAN_POINT('Ctrl Pts',(3.79773307923007,-2.40444525216584,4.3));
#18417=CARTESIAN_POINT('Ctrl Pts',(3.7964780509907,-2.39451257334247,4.3));
#18418=CARTESIAN_POINT('Ctrl Pts',(3.79582248849211,-2.38932425044823,4.3));
#18419=CARTESIAN_POINT('Ctrl Pts',(3.7949674129287,-2.38415491083777,4.3));
#18420=CARTESIAN_POINT('Ctrl Pts',(3.79391844712734,-2.37904222861684,4.3));
#18421=CARTESIAN_POINT('Ctrl Pts',(3.79135149974265,-2.3665308710123,4.3));
#18422=CARTESIAN_POINT('Ctrl Pts',(3.78762424888679,-2.35432630792998,4.3));
#18423=CARTESIAN_POINT('Ctrl Pts',(3.78275036269461,-2.34261709433331,4.3));
#18424=CARTESIAN_POINT('Ctrl Pts',(3.78051279286925,-2.33724146962858,4.3));
#18425=CARTESIAN_POINT('Ctrl Pts',(3.77803293300414,-2.33197059787363,4.3));
#18426=CARTESIAN_POINT('Ctrl Pts',(3.77530918258224,-2.32682518237142,4.3));
#18427=CARTESIAN_POINT('Ctrl Pts',(3.77352855433059,-2.32346141154425,4.3));
#18428=CARTESIAN_POINT('Ctrl Pts',(3.77164258388613,-2.32014955771335,4.3));
#18429=CARTESIAN_POINT('Ctrl Pts',(3.76965386637616,-2.31690144569075,4.3));
#18430=CARTESIAN_POINT('Ctrl Pts',(3.76538144816038,-2.30992343453397,4.3));
#18431=CARTESIAN_POINT('Ctrl Pts',(3.76065257819642,-2.3032660772289,4.3));
#18432=CARTESIAN_POINT('Ctrl Pts',(3.7554693784929,-2.29698171698016,4.3));
#18433=CARTESIAN_POINT('Ctrl Pts',(3.74976402854315,-2.29006427669614,4.3));
#18434=CARTESIAN_POINT('Ctrl Pts',(3.74350800901797,-2.28359846633093,4.3));
#18435=CARTESIAN_POINT('Ctrl Pts',(3.73677358655615,-2.27761728545388,4.3));
#18436=CARTESIAN_POINT('Ctrl Pts',(3.73252958089122,-2.2738479695743,4.3));
#18437=CARTESIAN_POINT('Ctrl Pts',(3.72809540845025,-2.27027136680987,4.3));
#18438=CARTESIAN_POINT('Ctrl Pts',(3.72348829039508,-2.26689850911598,4.3));
#18439=CARTESIAN_POINT('Ctrl Pts',(3.72067474538276,-2.26483872101672,4.3));
#18440=CARTESIAN_POINT('Ctrl Pts',(3.71780010895487,-2.26285764263401,4.3));
#18441=CARTESIAN_POINT('Ctrl Pts',(3.71487541375918,-2.26096143585197,4.3));
#18442=CARTESIAN_POINT('Ctrl Pts',(3.70626359340869,-2.25537801909854,4.3));
#18443=CARTESIAN_POINT('Ctrl Pts',(3.69720132775591,-2.25051601191126,4.3));
#18444=CARTESIAN_POINT('Ctrl Pts',(3.6877975535831,-2.24642648892188,4.3));
#18445=CARTESIAN_POINT('Ctrl Pts',(3.67897161991428,-2.24258825780551,4.3));
#18446=CARTESIAN_POINT('Ctrl Pts',(3.66984418789588,-2.23943054868187,4.3));
#18447=CARTESIAN_POINT('Ctrl Pts',(3.66050482692203,-2.23701743659906,4.3));
#18448=CARTESIAN_POINT('Ctrl Pts',(3.65701754284817,-2.23611638915498,4.3));
#18449=CARTESIAN_POINT('Ctrl Pts',(3.65350925028094,-2.23532164136865,4.3));
#18450=CARTESIAN_POINT('Ctrl Pts',(3.64998794572223,-2.2346361398089,4.3));
#18451=CARTESIAN_POINT('Ctrl Pts',(3.63890673460959,-2.23247893148594,4.3));
#18452=CARTESIAN_POINT('Ctrl Pts',(3.62768565700141,-2.23139728883196,4.3));
#18453=CARTESIAN_POINT('Ctrl Pts',(3.61647532022068,-2.23148774583768,4.3));
#18454=CARTESIAN_POINT('Ctrl Pts',(3.61029342610439,-2.23153762798149,4.3));
#18455=CARTESIAN_POINT('Ctrl Pts',(3.60411490309515,-2.23194477515726,4.3));
#18456=CARTESIAN_POINT('Ctrl Pts',(3.59796731355722,-2.23273189751379,4.3));
#18457=CARTESIAN_POINT('Ctrl Pts',(3.59689164899642,-2.23286962297817,4.3));
#18458=CARTESIAN_POINT('Ctrl Pts',(3.59581693782457,-2.2330189937725,4.3));
#18459=CARTESIAN_POINT('Ctrl Pts',(3.5947433329992,-2.23317993884958,4.3));
#18460=CARTESIAN_POINT('Origin',(3.6,-2.4,5.35459252805377));
#18461=CARTESIAN_POINT('Ctrl Pts',(3.39434265963601,-2.39985006386652,5.17959252805377));
#18462=CARTESIAN_POINT('Ctrl Pts',(3.39426084301402,-2.39002096866549,5.17905813053169));
#18463=CARTESIAN_POINT('Ctrl Pts',(3.39937061245186,-2.31213684688635,5.17481913665734));
#18464=CARTESIAN_POINT('Ctrl Pts',(3.49890445172815,-2.1791570162937,5.16687554643073));
#18465=CARTESIAN_POINT('Ctrl Pts',(3.73070050348011,-2.19531101338576,5.15576175737392));
#18466=CARTESIAN_POINT('Ctrl Pts',(3.84286217522106,-2.398786946145,5.14464796831712));
#18467=CARTESIAN_POINT('Ctrl Pts',(3.73273070558319,-2.60338928804541,5.13353417926031));
#18468=CARTESIAN_POINT('Ctrl Pts',(3.50110863577888,-2.62181907448596,5.12242039020351));
#18469=CARTESIAN_POINT('Ctrl Pts',(3.39978420932204,-2.4892623620427,5.11443983980132));
#18470=CARTESIAN_POINT('Ctrl Pts',(3.3942709677865,-2.41067410874191,5.11016388575141));
#18471=CARTESIAN_POINT('Ctrl Pts',(3.39436118987868,-2.40016037422423,5.10959252805377));
#18472=CARTESIAN_POINT('Ctrl Pts',(3.39473290683218,-2.40022967700174,5.18540747194623));
#18473=CARTESIAN_POINT('Ctrl Pts',(3.39508769549541,-2.35320983503088,5.18286245525962));
#18474=CARTESIAN_POINT('Ctrl Pts',(3.4343446160921,-2.23704698664849,5.17661284222074));
#18475=CARTESIAN_POINT('Ctrl Pts',(3.62721323091929,-2.15871475485289,5.16665863282959));
#18476=CARTESIAN_POINT('Ctrl Pts',(3.81747535364037,-2.29190664293025,5.15554484377279));
#18477=CARTESIAN_POINT('Ctrl Pts',(3.80876232171537,-2.52413791100821,5.14443105471598));
#18478=CARTESIAN_POINT('Ctrl Pts',(3.60892556988421,-2.64269428158759,5.13331726565918));
#18479=CARTESIAN_POINT('Ctrl Pts',(3.42787437077081,-2.55254601515802,5.12364273806926));
#18480=CARTESIAN_POINT('Ctrl Pts',(3.39500775643356,-2.44179202298147,5.11767280683161));
#18481=CARTESIAN_POINT('Ctrl Pts',(3.39479089893477,-2.39988380139174,5.11540747194623));
#18482=CARTESIAN_POINT('Ctrl Pts',(3.72690708798524,-2.29206413469515,5.2));
#18483=CARTESIAN_POINT('Ctrl Pts',(3.76279833110066,-2.33426376069605,5.19629540364773));
#18484=CARTESIAN_POINT('Ctrl Pts',(3.78852079223234,-2.45658683270444,5.18888621094319));
#18485=CARTESIAN_POINT('Ctrl Pts',(3.65451255926051,-2.58934148319728,5.1777724218864));
#18486=CARTESIAN_POINT('Ctrl Pts',(3.47057723832131,-2.54835675254144,5.16665863282959));
#18487=CARTESIAN_POINT('Ctrl Pts',(3.40512138630522,-2.37179019391731,5.15554484377279));
#18488=CARTESIAN_POINT('Ctrl Pts',(3.51803130141336,-2.22093957374148,5.14443105471598));
#18489=CARTESIAN_POINT('Ctrl Pts',(3.7059725216196,-2.23403730298123,5.13331726565917));
#18490=CARTESIAN_POINT('Ctrl Pts',(3.79691367996997,-2.39901645079819,5.12220347660237));
#18491=CARTESIAN_POINT('Ctrl Pts',(3.70761861808084,-2.56490889591613,5.11108968754556));
#18492=CARTESIAN_POINT('Ctrl Pts',(3.5198184631744,-2.57985184479553,5.09997589848876));
#18493=CARTESIAN_POINT('Ctrl Pts',(3.40540965360542,-2.43017761320763,5.08886210943196));
#18494=CARTESIAN_POINT('Ctrl Pts',(3.46911145738791,-2.25287984568082,5.07774832037515));
#18495=CARTESIAN_POINT('Ctrl Pts',(3.65261709726835,-2.21024363500907,5.06663453131835));
#18496=CARTESIAN_POINT('Ctrl Pts',(3.7879616770095,-2.34129317212888,5.05552074226154));
#18497=CARTESIAN_POINT('Ctrl Pts',(3.75126281927757,-2.52607793686066,5.04440695320475));
#18498=CARTESIAN_POINT('Ctrl Pts',(3.57611137907248,-2.59546203514889,5.03329316414793));
#18499=CARTESIAN_POINT('Ctrl Pts',(3.42282546878807,-2.4859375664189,5.02217937509114));
#18500=CARTESIAN_POINT('Ctrl Pts',(3.43170941408529,-2.29775344335704,5.01106558603433));
#18501=CARTESIAN_POINT('Ctrl Pts',(3.59463164228021,-2.20315676572473,4.99995179697753));
#18502=CARTESIAN_POINT('Ctrl Pts',(3.76246758864558,-2.28873292649683,4.98883800792072));
#18503=CARTESIAN_POINT('Ctrl Pts',(3.78159510888145,-2.47615310463782,4.97772421886392));
#18504=CARTESIAN_POINT('Ctrl Pts',(3.63450656639691,-2.59386948090233,4.96661042980711));
#18505=CARTESIAN_POINT('Ctrl Pts',(3.45583377242442,-2.53413492344978,4.95549664075031));
#18506=CARTESIAN_POINT('Ctrl Pts',(3.40911796147502,-2.3516251489795,4.94438285169351));
#18507=CARTESIAN_POINT('Ctrl Pts',(3.53711864515359,-2.21339342445149,4.93326906263669));
#18508=CARTESIAN_POINT('Ctrl Pts',(3.7226753460379,-2.24596481468812,4.9221552735799));
#18509=CARTESIAN_POINT('Ctrl Pts',(3.7959459114648,-2.41952635696717,4.91104148452308));
#18510=CARTESIAN_POINT('Ctrl Pts',(3.68986496194813,-2.57521520324594,4.89992769546629));
#18511=CARTESIAN_POINT('Ctrl Pts',(3.50152959362338,-2.57052758693027,4.88881390640948));
#18512=CARTESIAN_POINT('Ctrl Pts',(3.403325304985,-2.4097541363769,4.87770011735268));
#18513=CARTESIAN_POINT('Ctrl Pts',(3.48513959513685,-2.24005261418135,4.86658632829587));
#18514=CARTESIAN_POINT('Ctrl Pts',(3.6720869164654,-2.21675274815082,4.85547253923907));
#18515=CARTESIAN_POINT('Ctrl Pts',(3.79305226563199,-2.36118116990379,4.84435875018227));
#18516=CARTESIAN_POINT('Ctrl Pts',(3.73731468670399,-2.54114090707891,4.83324496112546));
#18517=CARTESIAN_POINT('Ctrl Pts',(3.55589141778138,-2.59191277135814,4.82213117206866));
#18518=CARTESIAN_POINT('Ctrl Pts',(3.41484123438881,-2.46702469957432,4.81101738301185));
#18519=CARTESIAN_POINT('Ctrl Pts',(3.44326896900338,-2.28078816015838,4.79990359395505));
#18520=CARTESIAN_POINT('Ctrl Pts',(3.61515439373994,-2.20366756970366,4.78878980489824));
#18521=CARTESIAN_POINT('Ctrl Pts',(3.77316883002382,-2.3062522792604,4.77767601584144));
#18522=CARTESIAN_POINT('Ctrl Pts',(3.77267987231879,-2.49464534078155,4.76656222678464));
#18523=CARTESIAN_POINT('Ctrl Pts',(3.61413506915742,-2.59640844853418,4.75544843772783));
#18524=CARTESIAN_POINT('Ctrl Pts',(3.44265227689368,-2.51839667592017,4.74433464867102));
#18525=CARTESIAN_POINT('Ctrl Pts',(3.4151916400337,-2.33201508312681,4.73322085961423));
#18526=CARTESIAN_POINT('Ctrl Pts',(3.55688819092022,-2.20786085574886,4.72210707055742));
#18527=CARTESIAN_POINT('Ctrl Pts',(3.73804546957863,-2.25957376611009,4.71099328150061));
#18528=CARTESIAN_POINT('Ctrl Pts',(3.79284816438962,-2.43982040089255,4.69987949244382));
#18529=CARTESIAN_POINT('Ctrl Pts',(3.67113474728785,-2.58361897114401,4.688765703387));
#18530=CARTESIAN_POINT('Ctrl Pts',(3.48431088927061,-2.55934901472658,4.67765191433021));
#18531=CARTESIAN_POINT('Ctrl Pts',(3.40337858630773,-2.38922509798919,4.66653812527339));
#18532=CARTESIAN_POINT('Ctrl Pts',(3.50241609313587,-2.22896357125796,4.6554243362166));
#18533=CARTESIAN_POINT('Ctrl Pts',(3.69077325659353,-2.22525362743943,4.64431054715978));
#18534=CARTESIAN_POINT('Ctrl Pts',(3.79604462885236,-2.38149102018406,4.63319675810299));
#18535=CARTESIAN_POINT('Ctrl Pts',(3.72187412902538,-2.5546698920607,4.62208296904618));
#18536=CARTESIAN_POINT('Ctrl Pts',(3.53615085675469,-2.58627765765756,4.61096917998938));
#18537=CARTESIAN_POINT('Ctrl Pts',(3.40886942939528,-2.44738337066962,4.59985539093257));
#18538=CARTESIAN_POINT('Ctrl Pts',(3.45653198087784,-2.26511854714084,4.58874160187577));
#18539=CARTESIAN_POINT('Ctrl Pts',(3.63551243730216,-2.20631224707971,4.57762781281896));
#18540=CARTESIAN_POINT('Ctrl Pts',(3.78198795712288,-2.32479054382313,4.56651402376216));
#18541=CARTESIAN_POINT('Ctrl Pts',(3.76188783591025,-2.51210890876234,4.55540023470536));
#18542=CARTESIAN_POINT('Ctrl Pts',(3.59360994254596,-2.59681271806211,4.54428644564855));
#18543=CARTESIAN_POINT('Ctrl Pts',(3.43118094125773,-2.50137161460726,4.53317265659175));
#18544=CARTESIAN_POINT('Ctrl Pts',(3.42327393893419,-2.31314392247853,4.52205886753494));
#18545=CARTESIAN_POINT('Ctrl Pts',(3.57712630459504,-2.2044165835037,4.51094507847814));
#18546=CARTESIAN_POINT('Ctrl Pts',(3.75191522290318,-2.2747089629466,4.49983128942133));
#18547=CARTESIAN_POINT('Ctrl Pts',(3.78765441517707,-2.45968165103968,4.48871750036453));
#18548=CARTESIAN_POINT('Ctrl Pts',(3.6516313924431,-2.59002704401991,4.47760371130773));
#18549=CARTESIAN_POINT('Ctrl Pts',(3.46834957196871,-2.54643853472375,4.46648992225092));
#18550=CARTESIAN_POINT('Ctrl Pts',(3.40556887868038,-2.36881316151698,4.45537613319412));
#18551=CARTESIAN_POINT('Ctrl Pts',(3.52075320095807,-2.21973347999151,4.44426234413732));
#18552=CARTESIAN_POINT('Ctrl Pts',(3.70847300665902,-2.23565373905929,4.43314855508051));
#18553=CARTESIAN_POINT('Ctrl Pts',(3.79690626014289,-2.40200209376731,4.4220347660237));
#18554=CARTESIAN_POINT('Ctrl Pts',(3.70510893870568,-2.56651771072077,4.4109209769669));
#18555=CARTESIAN_POINT('Ctrl Pts',(3.51710429764661,-2.57861817635772,4.3998071879101));
#18556=CARTESIAN_POINT('Ctrl Pts',(3.4049748648587,-2.42722660301959,4.3886933988533));
#18557=CARTESIAN_POINT('Ctrl Pts',(3.47135448681048,-2.25091580613535,4.37757960979649));
#18558=CARTESIAN_POINT('Ctrl Pts',(3.65548413146169,-2.21106026869437,4.36646582073969));
#18559=CARTESIAN_POINT('Ctrl Pts',(3.78882987196794,-2.34414980590083,4.35535203168288));
#18560=CARTESIAN_POINT('Ctrl Pts',(3.74933478455633,-2.5283468513898,4.34423824262608));
#18561=CARTESIAN_POINT('Ctrl Pts',(3.57315729153603,-2.59509221614966,4.33312445356927));
#18562=CARTESIAN_POINT('Ctrl Pts',(3.42153838470822,-2.4832160988167,4.32201066451247));
#18563=CARTESIAN_POINT('Ctrl Pts',(3.43328918604681,-2.2952742544727,4.31089687545567));
#18564=CARTESIAN_POINT('Ctrl Pts',(3.59758810222901,-2.20298223652265,4.29978308639886));
#18565=CARTESIAN_POINT('Ctrl Pts',(3.76418972838082,-2.29144636425406,4.28866929734206));
#18566=CARTESIAN_POINT('Ctrl Pts',(3.77483953817107,-2.41599017382994,4.28126010463752));
#18567=CARTESIAN_POINT('Ctrl Pts',(3.75264423560529,-2.46674801372684,4.27755550828525));
#18568=CARTESIAN_POINT('Ctrl Pts',(3.73677806246588,-2.28366876301903,5.20748149723825));
#18569=CARTESIAN_POINT('Ctrl Pts',(3.77546096639785,-2.32915072287504,5.20377690088598));
#18570=CARTESIAN_POINT('Ctrl Pts',(3.80318414917118,-2.46098821950194,5.19636770818144));
#18571=CARTESIAN_POINT('Ctrl Pts',(3.65875260676202,-2.60406867439235,5.18525391912464));
#18572=CARTESIAN_POINT('Ctrl Pts',(3.46051059194224,-2.55989610579284,5.17414013006784));
#18573=CARTESIAN_POINT('Ctrl Pts',(3.38996351094031,-2.36959600381834,5.16302634101104));
#18574=CARTESIAN_POINT('Ctrl Pts',(3.51165568485162,-2.20701205459222,5.15191255195423));
#18575=CARTESIAN_POINT('Ctrl Pts',(3.71421518223977,-2.22112853978274,5.14079876289742));
#18576=CARTESIAN_POINT('Ctrl Pts',(3.81222984505367,-2.39893994924713,5.12968497384063));
#18577=CARTESIAN_POINT('Ctrl Pts',(3.71598931391495,-2.57773569329255,5.11857118478381));
#18578=CARTESIAN_POINT('Ctrl Pts',(3.51358185404256,-2.59384092135901,5.10745739572702));
#18579=CARTESIAN_POINT('Ctrl Pts',(3.3902741999918,-2.43252486153385,5.0963436066702));
#18580=CARTESIAN_POINT('Ctrl Pts',(3.45893080093723,-2.2414366764148,5.08522981761341));
#18581=CARTESIAN_POINT('Ctrl Pts',(3.65670971362751,-2.19548417384656,5.07411602855659));
#18582=CARTESIAN_POINT('Ctrl Pts',(3.80258154534432,-2.33672688974895,5.0630022394998));
#18583=CARTESIAN_POINT('Ctrl Pts',(3.76302820963254,-2.53588441904446,5.05188845044299));
#18584=CARTESIAN_POINT('Ctrl Pts',(3.57425329556196,-2.61066528968353,5.04077466138618));
#18585=CARTESIAN_POINT('Ctrl Pts',(3.40904463665349,-2.49262188593578,5.02966087232938));
#18586=CARTESIAN_POINT('Ctrl Pts',(3.41861958509882,-2.28980059243768,5.01854708327258));
#18587=CARTESIAN_POINT('Ctrl Pts',(3.59421408544476,-2.18784607998553,5.00743329421577));
#18588=CARTESIAN_POINT('Ctrl Pts',(3.77510449842668,-2.28007844974125,4.99631950515897));
#18589=CARTESIAN_POINT('Ctrl Pts',(3.79571977846481,-2.48207637783269,4.98520571610217));
#18590=CARTESIAN_POINT('Ctrl Pts',(3.63719052551791,-2.60894886479604,4.97409192704536));
#18591=CARTESIAN_POINT('Ctrl Pts',(3.4446203628666,-2.54456808701342,4.96297813798855));
#18592=CARTESIAN_POINT('Ctrl Pts',(3.39427094417278,-2.34786249925276,4.95186434893176));
#18593=CARTESIAN_POINT('Ctrl Pts',(3.53222766342159,-2.19887895741578,4.94075055987495));
#18594=CARTESIAN_POINT('Ctrl Pts',(3.73221717092231,-2.23398378661889,4.92963677081814));
#18595=CARTESIAN_POINT('Ctrl Pts',(3.81118680243757,-2.42104513873408,4.91852298176134));
#18596=CARTESIAN_POINT('Ctrl Pts',(3.69685475865827,-2.58884363667168,4.90740919270454));
#18597=CARTESIAN_POINT('Ctrl Pts',(3.4938704558725,-2.58379141234426,4.89629540364773));
#18598=CARTESIAN_POINT('Ctrl Pts',(3.38802772841696,-2.41051282395524,4.88518161459093));
#18599=CARTESIAN_POINT('Ctrl Pts',(3.47620562507071,-2.22761172857971,4.87406782553412));
#18600=CARTESIAN_POINT('Ctrl Pts',(3.67769391702081,-2.20249957304951,4.86295403647733));
#18601=CARTESIAN_POINT('Ctrl Pts',(3.80806808561287,-2.35816179811509,4.85184024742051));
#18602=CARTESIAN_POINT('Ctrl Pts',(3.74799517579086,-2.552119003843,4.84072645836372));
#18603=CARTESIAN_POINT('Ctrl Pts',(3.55246060318804,-2.60683996020677,4.8296126693069));
#18604=CARTESIAN_POINT('Ctrl Pts',(3.40043937962063,-2.4722379552685,4.8184988802501));
#18605=CARTESIAN_POINT('Ctrl Pts',(3.43107825505782,-2.27151573063888,4.8073850911933));
#18606=CARTESIAN_POINT('Ctrl Pts',(3.61633311934347,-2.18839661486619,4.79627130213649));
#18607=CARTESIAN_POINT('Ctrl Pts',(3.78663809426387,-2.29896047725209,4.78515751307969));
#18608=CARTESIAN_POINT('Ctrl Pts',(3.7861111048846,-2.50200696067527,4.77404372402288));
#18609=CARTESIAN_POINT('Ctrl Pts',(3.61523451056097,-2.61168531615476,4.76292993496608));
#18610=CARTESIAN_POINT('Ctrl Pts',(3.43041359594979,-2.52760570108303,4.75181614590928));
#18611=CARTESIAN_POINT('Ctrl Pts',(3.40081704020639,-2.32672714066293,4.74070235685248));
#18612=CARTESIAN_POINT('Ctrl Pts',(3.55353490645048,-2.19291605936479,4.72958856779566));
#18613=CARTESIAN_POINT('Ctrl Pts',(3.74878279977045,-2.24865125742167,4.71847477873887));
#18614=CARTESIAN_POINT('Ctrl Pts',(3.80784810914882,-2.44291767597198,4.70736098968206));
#18615=CARTESIAN_POINT('Ctrl Pts',(3.67666768706539,-2.59790105898559,4.69624720062525));
#18616=CARTESIAN_POINT('Ctrl Pts',(3.47531246154031,-2.57174335835902,4.68513341156846));
#18617=CARTESIAN_POINT('Ctrl Pts',(3.38808515402025,-2.38838701412431,4.67401962251165));
#18618=CARTESIAN_POINT('Ctrl Pts',(3.49482590830325,-2.21566016756178,4.66290583345484));
#18619=CARTESIAN_POINT('Ctrl Pts',(3.69783370147164,-2.21166166018595,4.65179204439804));
#18620=CARTESIAN_POINT('Ctrl Pts',(3.81129319817336,-2.38005137114376,4.64067825534124));
#18621=CARTESIAN_POINT('Ctrl Pts',(3.73135363435924,-2.56670028832692,4.62956446628443));
#18622=CARTESIAN_POINT('Ctrl Pts',(3.53118459936441,-2.60076654109381,4.61845067722763));
#18623=CARTESIAN_POINT('Ctrl Pts',(3.3940030809914,-2.45106890195169,4.60733688817082));
#18624=CARTESIAN_POINT('Ctrl Pts',(3.44537287875023,-2.25462731768926,4.59622309911402));
#18625=CARTESIAN_POINT('Ctrl Pts',(3.63827463418116,-2.1912469981906,4.58510931005721));
#18626=CARTESIAN_POINT('Ctrl Pts',(3.79614318287948,-2.31894066865531,4.57399552100041));
#18627=CARTESIAN_POINT('Ctrl Pts',(3.77447965187866,-2.52082886440086,4.56288173194361));
#18628=CARTESIAN_POINT('Ctrl Pts',(3.59311291676859,-2.6121210302163,4.55176794288681));
#18629=CARTESIAN_POINT('Ctrl Pts',(3.41805000706685,-2.50925641156176,4.54065415383));
#18630=CARTESIAN_POINT('Ctrl Pts',(3.40952798930647,-2.3063881601463,4.52954036477319));
#18631=CARTESIAN_POINT('Ctrl Pts',(3.57534716312072,-2.18920388779283,4.51842657571639));
#18632=CARTESIAN_POINT('Ctrl Pts',(3.76373135793792,-2.26496368670519,4.50731278665958));
#18633=CARTESIAN_POINT('Ctrl Pts',(3.80225038434475,-2.46432375625011,4.49619899760278));
#18634=CARTESIAN_POINT('Ctrl Pts',(3.65564733958441,-2.60480755889841,4.48508520854597));
#18635=CARTESIAN_POINT('Ctrl Pts',(3.45810965522258,-2.55782868685937,4.47397141948917));
#18636=CARTESIAN_POINT('Ctrl Pts',(3.39044580977021,-2.36638741452612,4.46285763043237));
#18637=CARTESIAN_POINT('Ctrl Pts',(3.51458929677089,-2.20571214952866,4.45174384137556));
#18638=CARTESIAN_POINT('Ctrl Pts',(3.71691015778721,-2.22287070405714,4.44063005231876));
#18639=CARTESIAN_POINT('Ctrl Pts',(3.81222184810419,-2.40215781884775,4.42951626326195));
#18640=CARTESIAN_POINT('Ctrl Pts',(3.71328442888611,-2.57946964350242,4.41840247420515));
#18641=CARTESIAN_POINT('Ctrl Pts',(3.51065657770066,-2.59251129681771,4.40728868514835));
#18642=CARTESIAN_POINT('Ctrl Pts',(3.38980559289267,-2.42934431849055,4.39617489609154));
#18643=CARTESIAN_POINT('Ctrl Pts',(3.46134829568354,-2.23931987168859,4.38506110703474));
#18644=CARTESIAN_POINT('Ctrl Pts',(3.65979974892982,-2.19636432620836,4.37394731797793));
#18645=CARTESIAN_POINT('Ctrl Pts',(3.80351726947246,-2.33980571567353,4.36283352892113));
#18646=CARTESIAN_POINT('Ctrl Pts',(3.76095021022585,-2.5383298122697,4.35171973986433));
#18647=CARTESIAN_POINT('Ctrl Pts',(3.57106943581066,-2.61026670575114,4.34060595080752));
#18648=CARTESIAN_POINT('Ctrl Pts',(3.4076574417421,-2.48968873955599,4.32949216175071));
#18649=CARTESIAN_POINT('Ctrl Pts',(3.42032223348093,-2.28712856948396,4.31837837269392));
#18650=CARTESIAN_POINT('Ctrl Pts',(3.59740050213728,-2.18765797570795,4.30726458363711));
#18651=CARTESIAN_POINT('Ctrl Pts',(3.77696058810632,-2.28300294170579,4.29615079458031));
#18652=CARTESIAN_POINT('Ctrl Pts',(3.78843875194939,-2.41723390733862,4.28874160187577));
#18653=CARTESIAN_POINT('Ctrl Pts',(3.76451707405898,-2.471939748488,4.2850370055235));
#18654=CARTESIAN_POINT('Ctrl Pts',(3.74664903694653,-2.2752733913429,5.2149629944765));
#18655=CARTESIAN_POINT('Ctrl Pts',(3.78812360169505,-2.32403768505403,5.21125839812423));
#18656=CARTESIAN_POINT('Ctrl Pts',(3.81784750611002,-2.46538960629943,5.20384920541969));
#18657=CARTESIAN_POINT('Ctrl Pts',(3.66299265426352,-2.61879586558741,5.19273541636289));
#18658=CARTESIAN_POINT('Ctrl Pts',(3.45044394556317,-2.57143545904423,5.18162162730609));
#18659=CARTESIAN_POINT('Ctrl Pts',(3.37480563557539,-2.36740181371937,5.17050783824928));
#18660=CARTESIAN_POINT('Ctrl Pts',(3.50528006828989,-2.19308453544296,5.15939404919248));
#18661=CARTESIAN_POINT('Ctrl Pts',(3.72245784285994,-2.20821977658425,5.14828026013567));
#18662=CARTESIAN_POINT('Ctrl Pts',(3.82754601013736,-2.39886344769606,5.13716647107887));
#18663=CARTESIAN_POINT('Ctrl Pts',(3.72436000974907,-2.59056249066898,5.12605268202206));
#18664=CARTESIAN_POINT('Ctrl Pts',(3.50734524491072,-2.60782999792249,5.11493889296526));
#18665=CARTESIAN_POINT('Ctrl Pts',(3.37513874637818,-2.43487210986008,5.10382510390845));
#18666=CARTESIAN_POINT('Ctrl Pts',(3.44875014448657,-2.22999350714877,5.09271131485166));
#18667=CARTESIAN_POINT('Ctrl Pts',(3.66080232998667,-2.18072471268405,5.08159752579485));
#18668=CARTESIAN_POINT('Ctrl Pts',(3.81720141367915,-2.33216060736901,5.07048373673804));
#18669=CARTESIAN_POINT('Ctrl Pts',(3.77479359998752,-2.54569090122825,5.05936994768124));
#18670=CARTESIAN_POINT('Ctrl Pts',(3.57239521205144,-2.62586854421817,5.04825615862443));
#18671=CARTESIAN_POINT('Ctrl Pts',(3.39526380451891,-2.49930620545266,5.03714236956763));
#18672=CARTESIAN_POINT('Ctrl Pts',(3.40552975611236,-2.28184774151832,5.02602858051083));
#18673=CARTESIAN_POINT('Ctrl Pts',(3.59379652860931,-2.17253539424633,5.01491479145402));
#18674=CARTESIAN_POINT('Ctrl Pts',(3.78774140820779,-2.27142397298568,5.00380100239722));
#18675=CARTESIAN_POINT('Ctrl Pts',(3.80984444804818,-2.48799965102756,4.99268721334042));
#18676=CARTESIAN_POINT('Ctrl Pts',(3.63987448463892,-2.62402824868975,4.98157342428361));
#18677=CARTESIAN_POINT('Ctrl Pts',(3.43340695330878,-2.55500125057707,4.9704596352268));
#18678=CARTESIAN_POINT('Ctrl Pts',(3.37942392687054,-2.34409984952602,4.95934584617001));
#18679=CARTESIAN_POINT('Ctrl Pts',(3.52733668168959,-2.18436449038006,4.94823205711319));
#18680=CARTESIAN_POINT('Ctrl Pts',(3.74175899580671,-2.22200275854966,4.9371182680564));
#18681=CARTESIAN_POINT('Ctrl Pts',(3.82642769341035,-2.42256392050098,4.92600447899958));
#18682=CARTESIAN_POINT('Ctrl Pts',(3.70384455536842,-2.60247207009742,4.91489068994279));
#18683=CARTESIAN_POINT('Ctrl Pts',(3.48621131812161,-2.59705523775825,4.90377690088598));
#18684=CARTESIAN_POINT('Ctrl Pts',(3.37273015184892,-2.41127151153357,4.89266311182918));
#18685=CARTESIAN_POINT('Ctrl Pts',(3.46727165500458,-2.21517084297807,4.88154932277238));
#18686=CARTESIAN_POINT('Ctrl Pts',(3.68330091757622,-2.1882463979482,4.87043553371556));
#18687=CARTESIAN_POINT('Ctrl Pts',(3.82308390559375,-2.3551424263264,4.85932174465877));
#18688=CARTESIAN_POINT('Ctrl Pts',(3.75867566487773,-2.56309710060709,4.84820795560196));
#18689=CARTESIAN_POINT('Ctrl Pts',(3.54902978859471,-2.62176714905541,4.83709416654515));
#18690=CARTESIAN_POINT('Ctrl Pts',(3.38603752485245,-2.47745121096268,4.82598037748835));
#18691=CARTESIAN_POINT('Ctrl Pts',(3.41888754111225,-2.26224330111939,4.81486658843154));
#18692=CARTESIAN_POINT('Ctrl Pts',(3.61751184494699,-2.17312566002871,4.80375279937474));
#18693=CARTESIAN_POINT('Ctrl Pts',(3.80010735850391,-2.29166867524379,4.79263901031795));
#18694=CARTESIAN_POINT('Ctrl Pts',(3.79954233745042,-2.50936858056899,4.78152522126113));
#18695=CARTESIAN_POINT('Ctrl Pts',(3.61633395196453,-2.62696218377534,4.77041143220433));
#18696=CARTESIAN_POINT('Ctrl Pts',(3.4181749150059,-2.53681472624589,4.75929764314752));
#18697=CARTESIAN_POINT('Ctrl Pts',(3.38644244037908,-2.32143919819905,4.74818385409072));
#18698=CARTESIAN_POINT('Ctrl Pts',(3.55018162198074,-2.1779712629807,4.73707006503392));
#18699=CARTESIAN_POINT('Ctrl Pts',(3.75952012996226,-2.23772874873326,4.72595627597711));
#18700=CARTESIAN_POINT('Ctrl Pts',(3.82284805390801,-2.44601495105141,4.71484248692031));
#18701=CARTESIAN_POINT('Ctrl Pts',(3.68220062684293,-2.61218314682717,4.7037286978635));
#18702=CARTESIAN_POINT('Ctrl Pts',(3.46631403381001,-2.58413770199147,4.69261490880671));
#18703=CARTESIAN_POINT('Ctrl Pts',(3.37279172173275,-2.38754893025942,4.68150111974989));
#18704=CARTESIAN_POINT('Ctrl Pts',(3.48723572347063,-2.20235676386561,4.6703873306931));
#18705=CARTESIAN_POINT('Ctrl Pts',(3.70489414634973,-2.19806969293246,4.65927354163628));
#18706=CARTESIAN_POINT('Ctrl Pts',(3.82654176749436,-2.37861172210345,4.64815975257949));
#18707=CARTESIAN_POINT('Ctrl Pts',(3.7408331396931,-2.57873068459315,4.63704596352267));
#18708=CARTESIAN_POINT('Ctrl Pts',(3.52621834197413,-2.61525542453006,4.62593217446588));
#18709=CARTESIAN_POINT('Ctrl Pts',(3.37913673258752,-2.45475443323377,4.61481838540907));
#18710=CARTESIAN_POINT('Ctrl Pts',(3.43421377662264,-2.24413608823767,4.60370459635227));
#18711=CARTESIAN_POINT('Ctrl Pts',(3.64103683106015,-2.17618174930149,4.59259080729546));
#18712=CARTESIAN_POINT('Ctrl Pts',(3.81029840863609,-2.31309079348749,4.58147701823866));
#18713=CARTESIAN_POINT('Ctrl Pts',(3.78707146784707,-2.52954882003939,4.57036322918186));
#18714=CARTESIAN_POINT('Ctrl Pts',(3.59261589099123,-2.62742934237049,4.55924944012505));
#18715=CARTESIAN_POINT('Ctrl Pts',(3.40491907287596,-2.51714120851626,4.54813565106824));
#18716=CARTESIAN_POINT('Ctrl Pts',(3.39578203967876,-2.29963239781408,4.53702186201144));
#18717=CARTESIAN_POINT('Ctrl Pts',(3.57356802164639,-2.17399119208196,4.52590807295464));
#18718=CARTESIAN_POINT('Ctrl Pts',(3.77554749297266,-2.2552184104638,4.51479428389784));
#18719=CARTESIAN_POINT('Ctrl Pts',(3.81684635351243,-2.46896586146052,4.50368049484103));
#18720=CARTESIAN_POINT('Ctrl Pts',(3.65966328672572,-2.61958807377691,4.49256670578423));
#18721=CARTESIAN_POINT('Ctrl Pts',(3.44786973847645,-2.56921883899499,4.48145291672742));
#18722=CARTESIAN_POINT('Ctrl Pts',(3.37532274086005,-2.36396166753528,4.47033912767061));
#18723=CARTESIAN_POINT('Ctrl Pts',(3.5084253925837,-2.19169081906581,4.45922533861382));
#18724=CARTESIAN_POINT('Ctrl Pts',(3.7253473089154,-2.21008766905501,4.44811154955701));
#18725=CARTESIAN_POINT('Ctrl Pts',(3.82753743606548,-2.40231354392819,4.43699776050021));
#18726=CARTESIAN_POINT('Ctrl Pts',(3.72145991906655,-2.59242157628407,4.4258839714434));
#18727=CARTESIAN_POINT('Ctrl Pts',(3.5042088577547,-2.60640441727771,4.41477018238659));
#18728=CARTESIAN_POINT('Ctrl Pts',(3.37463632092665,-2.43146203396151,4.4036563933298));
#18729=CARTESIAN_POINT('Ctrl Pts',(3.45134210455661,-2.22772393724184,4.39254260427299));
#18730=CARTESIAN_POINT('Ctrl Pts',(3.66411536639796,-2.18166838372235,4.38142881521618));
#18731=CARTESIAN_POINT('Ctrl Pts',(3.81820466697696,-2.33546162544623,4.37031502615938));
#18732=CARTESIAN_POINT('Ctrl Pts',(3.77256563589538,-2.54831277314961,4.35920123710258));
#18733=CARTESIAN_POINT('Ctrl Pts',(3.5689815800853,-2.62544119535262,4.34808744804577));
#18734=CARTESIAN_POINT('Ctrl Pts',(3.39377649877598,-2.49616138029528,4.33697365898897));
#18735=CARTESIAN_POINT('Ctrl Pts',(3.40735528091504,-2.27898288449522,4.32585986993216));
#18736=CARTESIAN_POINT('Ctrl Pts',(3.59721290204555,-2.17233371489326,4.31474608087536));
#18737=CARTESIAN_POINT('Ctrl Pts',(3.78973144783182,-2.27455951915752,4.30363229181856));
#18738=CARTESIAN_POINT('Ctrl Pts',(3.8020379657277,-2.4184776408473,4.29622309911402));
#18739=CARTESIAN_POINT('Ctrl Pts',(3.77638991251267,-2.47713148324917,4.29251850276175));
#18740=CARTESIAN_POINT('Ctrl Pts',(3.75652001142717,-2.26687801966678,5.22244449171475));
#18741=CARTESIAN_POINT('Ctrl Pts',(3.80078623699225,-2.31892464723302,5.21873989536248));
#18742=CARTESIAN_POINT('Ctrl Pts',(3.83251086304886,-2.46979099309691,5.21133070265794));
#18743=CARTESIAN_POINT('Ctrl Pts',(3.66723270176503,-2.63352305678248,5.20021691360114));
#18744=CARTESIAN_POINT('Ctrl Pts',(3.4403772991841,-2.58297481229563,5.18910312454433));
#18745=CARTESIAN_POINT('Ctrl Pts',(3.35964776021048,-2.3652076236204,5.17798933548753));
#18746=CARTESIAN_POINT('Ctrl Pts',(3.49890445172815,-2.1791570162937,5.16687554643073));
#18747=CARTESIAN_POINT('Ctrl Pts',(3.73070050348011,-2.19531101338576,5.15576175737392));
#18748=CARTESIAN_POINT('Ctrl Pts',(3.84286217522106,-2.398786946145,5.14464796831712));
#18749=CARTESIAN_POINT('Ctrl Pts',(3.73273070558319,-2.60338928804541,5.13353417926031));
#18750=CARTESIAN_POINT('Ctrl Pts',(3.50110863577888,-2.62181907448596,5.12242039020351));
#18751=CARTESIAN_POINT('Ctrl Pts',(3.36000329276455,-2.4372193581863,5.1113066011467));
#18752=CARTESIAN_POINT('Ctrl Pts',(3.4385694880359,-2.21855033788275,5.10019281208991));
#18753=CARTESIAN_POINT('Ctrl Pts',(3.66489494634582,-2.16596525152154,5.08907902303309));
#18754=CARTESIAN_POINT('Ctrl Pts',(3.83182128201397,-2.32759432498908,5.07796523397629));
#18755=CARTESIAN_POINT('Ctrl Pts',(3.78655899034249,-2.55549738341204,5.06685144491949));
#18756=CARTESIAN_POINT('Ctrl Pts',(3.57053712854092,-2.64107179875281,5.05573765586268));
#18757=CARTESIAN_POINT('Ctrl Pts',(3.38148297238433,-2.50599052496954,5.04462386680588));
#18758=CARTESIAN_POINT('Ctrl Pts',(3.3924399271259,-2.27389489059897,5.03351007774908));
#18759=CARTESIAN_POINT('Ctrl Pts',(3.59337897177386,-2.15722470850713,5.02239628869227));
#18760=CARTESIAN_POINT('Ctrl Pts',(3.8003783179889,-2.26276949623011,5.01128249963547));
#18761=CARTESIAN_POINT('Ctrl Pts',(3.82396911763155,-2.49392292422242,5.00016871057867));
#18762=CARTESIAN_POINT('Ctrl Pts',(3.64255844375993,-2.63910763258347,4.98905492152186));
#18763=CARTESIAN_POINT('Ctrl Pts',(3.42219354375095,-2.56543441414071,4.97794113246505));
#18764=CARTESIAN_POINT('Ctrl Pts',(3.3645769095683,-2.34033719979929,4.96682734340826));
#18765=CARTESIAN_POINT('Ctrl Pts',(3.52244569995759,-2.16985002334435,4.95571355435144));
#18766=CARTESIAN_POINT('Ctrl Pts',(3.75130082069111,-2.21002173048044,4.94459976529465));
#18767=CARTESIAN_POINT('Ctrl Pts',(3.84166858438312,-2.42408270226789,4.93348597623783));
#18768=CARTESIAN_POINT('Ctrl Pts',(3.71083435207858,-2.61610050352316,4.92237218718104));
#18769=CARTESIAN_POINT('Ctrl Pts',(3.47855218037073,-2.61031906317225,4.91125839812423));
#18770=CARTESIAN_POINT('Ctrl Pts',(3.35743257528088,-2.4120301991119,4.90014460906743));
#18771=CARTESIAN_POINT('Ctrl Pts',(3.45833768493844,-2.20272995737643,4.88903082001062));
#18772=CARTESIAN_POINT('Ctrl Pts',(3.68890791813162,-2.17399322284688,4.87791703095382));
#18773=CARTESIAN_POINT('Ctrl Pts',(3.83809972557463,-2.3521230545377,4.86680324189701));
#18774=CARTESIAN_POINT('Ctrl Pts',(3.76935615396461,-2.57407519737118,4.85568945284021));
#18775=CARTESIAN_POINT('Ctrl Pts',(3.54559897400137,-2.63669433790405,4.8445756637834));
#18776=CARTESIAN_POINT('Ctrl Pts',(3.37163567008428,-2.48266446665686,4.8334618747266));
#18777=CARTESIAN_POINT('Ctrl Pts',(3.40669682716669,-2.25297087159989,4.8223480856698));
#18778=CARTESIAN_POINT('Ctrl Pts',(3.61869057055051,-2.15785470519124,4.81123429661299));
#18779=CARTESIAN_POINT('Ctrl Pts',(3.81357662274397,-2.28437687323548,4.80012050755619));
#18780=CARTESIAN_POINT('Ctrl Pts',(3.81297357001622,-2.51673020046272,4.78900671849938));
#18781=CARTESIAN_POINT('Ctrl Pts',(3.61743339336808,-2.64223905139592,4.77789292944258));
#18782=CARTESIAN_POINT('Ctrl Pts',(3.405936234062,-2.54602375140875,4.76677914038577));
#18783=CARTESIAN_POINT('Ctrl Pts',(3.37206784055177,-2.31615125573517,4.75566535132898));
#18784=CARTESIAN_POINT('Ctrl Pts',(3.546828337511,-2.16302646659663,4.74455156227216));
#18785=CARTESIAN_POINT('Ctrl Pts',(3.77025746015408,-2.22680624004484,4.73343777321537));
#18786=CARTESIAN_POINT('Ctrl Pts',(3.83784799866721,-2.44911222613084,4.72232398415856));
#18787=CARTESIAN_POINT('Ctrl Pts',(3.68773356662048,-2.62646523466876,4.71121019510175));
#18788=CARTESIAN_POINT('Ctrl Pts',(3.4573156060797,-2.59653204562391,4.70009640604496));
#18789=CARTESIAN_POINT('Ctrl Pts',(3.35749828944527,-2.38671084639454,4.68898261698814));
#18790=CARTESIAN_POINT('Ctrl Pts',(3.47964553863801,-2.18905336016944,4.67786882793135));
#18791=CARTESIAN_POINT('Ctrl Pts',(3.71195459122784,-2.18447772567898,4.66675503887453));
#18792=CARTESIAN_POINT('Ctrl Pts',(3.84179033681535,-2.37717207306315,4.65564124981774));
#18793=CARTESIAN_POINT('Ctrl Pts',(3.75031264502696,-2.59076108085938,4.64452746076093));
#18794=CARTESIAN_POINT('Ctrl Pts',(3.52125208458385,-2.6297443079663,4.63341367170413));
#18795=CARTESIAN_POINT('Ctrl Pts',(3.36427038418365,-2.45843996451585,4.62229988264732));
#18796=CARTESIAN_POINT('Ctrl Pts',(3.42305467449503,-2.23364485878609,4.61118609359052));
#18797=CARTESIAN_POINT('Ctrl Pts',(3.64379902793915,-2.16111650041238,4.60007230453371));
#18798=CARTESIAN_POINT('Ctrl Pts',(3.82445363439269,-2.30724091831967,4.58895851547691));
#18799=CARTESIAN_POINT('Ctrl Pts',(3.79966328381548,-2.53826877567792,4.57784472642011));
#18800=CARTESIAN_POINT('Ctrl Pts',(3.59211886521387,-2.64273765452468,4.5667309373633));
#18801=CARTESIAN_POINT('Ctrl Pts',(3.39178813868507,-2.52502600547076,4.5556171483065));
#18802=CARTESIAN_POINT('Ctrl Pts',(3.38203609005104,-2.29287663548185,4.54450335924969));
#18803=CARTESIAN_POINT('Ctrl Pts',(3.57178888017207,-2.15877849637109,4.53338957019289));
#18804=CARTESIAN_POINT('Ctrl Pts',(3.78736362800739,-2.2454731342224,4.52227578113608));
#18805=CARTESIAN_POINT('Ctrl Pts',(3.83144232268012,-2.47360796667095,4.51116199207928));
#18806=CARTESIAN_POINT('Ctrl Pts',(3.66367923386702,-2.6343685886554,4.50004820302247));
#18807=CARTESIAN_POINT('Ctrl Pts',(3.43762982173032,-2.58060899113062,4.48893441396567));
#18808=CARTESIAN_POINT('Ctrl Pts',(3.36019967194989,-2.36153592054442,4.47782062490886));
#18809=CARTESIAN_POINT('Ctrl Pts',(3.50226148839652,-2.17766948860297,4.46670683585206));
#18810=CARTESIAN_POINT('Ctrl Pts',(3.73378446004359,-2.19730463405286,4.45559304679526));
#18811=CARTESIAN_POINT('Ctrl Pts',(3.84285302402677,-2.40246926900864,4.44447925773845));
#18812=CARTESIAN_POINT('Ctrl Pts',(3.72963540924699,-2.60537350906572,4.43336546868165));
#18813=CARTESIAN_POINT('Ctrl Pts',(3.49776113780875,-2.62029753773771,4.42225167962485));
#18814=CARTESIAN_POINT('Ctrl Pts',(3.35946704896063,-2.43357974943247,4.41113789056804));
#18815=CARTESIAN_POINT('Ctrl Pts',(3.44133591342967,-2.21612800279508,4.40002410151124));
#18816=CARTESIAN_POINT('Ctrl Pts',(3.66843098386609,-2.16697244123634,4.38891031245443));
#18817=CARTESIAN_POINT('Ctrl Pts',(3.83289206448147,-2.33111753521892,4.37779652339763));
#18818=CARTESIAN_POINT('Ctrl Pts',(3.7841810615649,-2.55829573402952,4.36668273434082));
#18819=CARTESIAN_POINT('Ctrl Pts',(3.56689372435994,-2.6406156849541,4.35556894528403));
#18820=CARTESIAN_POINT('Ctrl Pts',(3.37989555580985,-2.50263402103458,4.34445515622721));
#18821=CARTESIAN_POINT('Ctrl Pts',(3.39438832834916,-2.27083719950648,4.33334136717041));
#18822=CARTESIAN_POINT('Ctrl Pts',(3.59702530195382,-2.15700945407857,4.32222757811361));
#18823=CARTESIAN_POINT('Ctrl Pts',(3.80250230755732,-2.26611609660926,4.31111378905681));
#18824=CARTESIAN_POINT('Ctrl Pts',(3.81563717950601,-2.41972137435598,4.30370459635227));
#18825=CARTESIAN_POINT('Ctrl Pts',(3.78826275096636,-2.48232321801033,4.3));
#18826=CARTESIAN_POINT('Ctrl Pts',(3.72690708798524,-2.29206413469515,5.2));
#18827=CARTESIAN_POINT('Ctrl Pts',(3.73511889692415,-2.29972488088976,5.2));
#18828=CARTESIAN_POINT('Ctrl Pts',(3.74243606331987,-2.3082260358574,5.2));
#18829=CARTESIAN_POINT('Ctrl Pts',(3.74885415883116,-2.3173733937361,5.2));
#18830=CARTESIAN_POINT('Ctrl Pts',(3.75362492547366,-2.32417290455016,5.2));
#18831=CARTESIAN_POINT('Ctrl Pts',(3.75789857922842,-2.33133076203089,5.2));
#18832=CARTESIAN_POINT('Ctrl Pts',(3.7616631192462,-2.3387816278666,5.2));
#18833=CARTESIAN_POINT('Ctrl Pts',(3.76388041855661,-2.34317015863036,5.2));
#18834=CARTESIAN_POINT('Ctrl Pts',(3.76592248852987,-2.34766555277529,5.2));
#18835=CARTESIAN_POINT('Ctrl Pts',(3.76777441807103,-2.35222602465318,5.2));
#18836=CARTESIAN_POINT('Ctrl Pts',(3.77233274722043,-2.36345114495818,5.2));
#18837=CARTESIAN_POINT('Ctrl Pts',(3.77575806540191,-2.37509440908006,5.2));
#18838=CARTESIAN_POINT('Ctrl Pts',(3.77802228391775,-2.38695732035888,5.2));
#18839=CARTESIAN_POINT('Ctrl Pts',(3.77946116292117,-2.39449603353478,5.2));
#18840=CARTESIAN_POINT('Ctrl Pts',(3.78043041033378,-2.40212433051409,5.2));
#18841=CARTESIAN_POINT('Ctrl Pts',(3.78091325285907,-2.40979638894873,5.2));
#18842=CARTESIAN_POINT('Ctrl Pts',(3.78113857897669,-2.41337667662164,5.2));
#18843=CARTESIAN_POINT('Ctrl Pts',(3.78125743502661,-2.41696304534708,5.2));
#18844=CARTESIAN_POINT('Ctrl Pts',(3.78126867486757,-2.42054069500775,5.2));
#18845=CARTESIAN_POINT('Ctrl Pts',(3.78130372190818,-2.4316961938677,5.2));
#18846=CARTESIAN_POINT('Ctrl Pts',(3.78029682789473,-2.44279407568189,5.2));
#18847=CARTESIAN_POINT('Ctrl Pts',(3.77821427386403,-2.45369318996624,5.2));
#18848=CARTESIAN_POINT('Ctrl Pts',(3.77705389172366,-2.45976608765585,5.2));
#18849=CARTESIAN_POINT('Ctrl Pts',(3.77555901526444,-2.46577751393184,5.2));
#18850=CARTESIAN_POINT('Ctrl Pts',(3.77374837416276,-2.47171132791926,5.2));
#18851=CARTESIAN_POINT('Ctrl Pts',(3.77261573055045,-2.47542321566067,5.2));
#18852=CARTESIAN_POINT('Ctrl Pts',(3.77135887218697,-2.47910625090944,5.2));
#18853=CARTESIAN_POINT('Ctrl Pts',(3.76998349987259,-2.48275161867489,5.2));
#18854=CARTESIAN_POINT('Ctrl Pts',(3.76560171320323,-2.49436536406777,5.2));
#18855=CARTESIAN_POINT('Ctrl Pts',(3.76005261276,-2.50551619028979,5.2));
#18856=CARTESIAN_POINT('Ctrl Pts',(3.75350161664164,-2.51608155564839,5.2));
#18857=CARTESIAN_POINT('Ctrl Pts',(3.74916064083137,-2.52308262764107,5.2));
#18858=CARTESIAN_POINT('Ctrl Pts',(3.7443785440277,-2.5298267716061,5.2));
#18859=CARTESIAN_POINT('Ctrl Pts',(3.73919190918146,-2.53627611456138,5.2));
#18860=CARTESIAN_POINT('Ctrl Pts',(3.73648178297727,-2.53964603241007,5.2));
#18861=CARTESIAN_POINT('Ctrl Pts',(3.73365980796544,-2.54293677988309,5.2));
#18862=CARTESIAN_POINT('Ctrl Pts',(3.73073436285314,-2.54613815029323,5.2));
#18863=CARTESIAN_POINT('Ctrl Pts',(3.72446793550896,-2.55299562131278,5.2));
#18864=CARTESIAN_POINT('Ctrl Pts',(3.71775196798206,-2.55941733778444,5.2));
#18865=CARTESIAN_POINT('Ctrl Pts',(3.71064054370859,-2.56535254658103,5.2));
#18866=CARTESIAN_POINT('Ctrl Pts',(3.70611395375814,-2.56913044752735,5.2));
#18867=CARTESIAN_POINT('Ctrl Pts',(3.70142688925274,-2.57271116046832,5.2));
#18868=CARTESIAN_POINT('Ctrl Pts',(3.69659110235036,-2.57608017868915,5.2));
#18869=CARTESIAN_POINT('Ctrl Pts',(3.69251867261816,-2.57891737773199,5.2));
#18870=CARTESIAN_POINT('Ctrl Pts',(3.68834776817108,-2.58159940125718,5.2));
#18871=CARTESIAN_POINT('Ctrl Pts',(3.68408920348942,-2.58411662981112,5.2));
#18872=CARTESIAN_POINT('Ctrl Pts',(3.67536613625436,-2.58927281635833,5.2));
#18873=CARTESIAN_POINT('Ctrl Pts',(3.6662720325658,-2.59374119323572,5.2));
#18874=CARTESIAN_POINT('Ctrl Pts',(3.65686566045376,-2.59744798255001,5.2));
#18875=CARTESIAN_POINT('Ctrl Pts',(3.6556263522049,-2.59793635942042,5.2));
#18876=CARTESIAN_POINT('Ctrl Pts',(3.65438160822106,-2.59841149615413,5.2));
#18877=CARTESIAN_POINT('Ctrl Pts',(3.65313161981588,-2.59887345085171,5.2));
#18878=CARTESIAN_POINT('Ctrl Pts',(3.43326718206005,-2.40013003210005,5.08714803633902));
#18879=CARTESIAN_POINT('Ctrl Pts',(3.4331940296057,-2.4086546125631,5.08771939403667));
#18880=CARTESIAN_POINT('Ctrl Pts',(3.43379133726061,-2.41716890764345,5.08829075173431));
#18881=CARTESIAN_POINT('Ctrl Pts',(3.43509475583067,-2.42557369055115,5.08886210943196));
#18882=CARTESIAN_POINT('Ctrl Pts',(3.44354592346175,-2.48006902373693,5.09256670578423));
#18883=CARTESIAN_POINT('Ctrl Pts',(3.48168219331808,-2.52996043426623,5.0962713021365));
#18884=CARTESIAN_POINT('Ctrl Pts',(3.53205035406398,-2.55241564805098,5.09997589848876));
#18885=CARTESIAN_POINT('Ctrl Pts',(3.58241851480988,-2.57487086183573,5.10368049484103));
#18886=CARTESIAN_POINT('Ctrl Pts',(3.64501856644536,-2.56988987887593,5.1073850911933));
#18887=CARTESIAN_POINT('Ctrl Pts',(3.69120110257795,-2.53975064654304,5.11108968754557));
#18888=CARTESIAN_POINT('Ctrl Pts',(3.73738363871054,-2.50961141421015,5.11479428389783));
#18889=CARTESIAN_POINT('Ctrl Pts',(3.76714865934026,-2.45431393250417,5.1184988802501));
#18890=CARTESIAN_POINT('Ctrl Pts',(3.76687430993005,-2.39916866701502,5.12220347660237));
#18891=CARTESIAN_POINT('Ctrl Pts',(3.76659996051984,-2.34402340152587,5.12590807295464));
#18892=CARTESIAN_POINT('Ctrl Pts',(3.73628624106972,-2.28903035225355,5.12961266930691));
#18893=CARTESIAN_POINT('Ctrl Pts',(3.68980584464362,-2.2593508727441,5.13331726565917));
#18894=CARTESIAN_POINT('Ctrl Pts',(3.64332544821752,-2.22967139323465,5.13702186201144));
#18895=CARTESIAN_POINT('Ctrl Pts',(3.58067837481544,-2.22530548348806,5.14072645836371));
#18896=CARTESIAN_POINT('Ctrl Pts',(3.53053651892971,-2.24826429864408,5.14443105471598));
#18897=CARTESIAN_POINT('Ctrl Pts',(3.48039466304398,-2.27122311380009,5.14813565106825));
#18898=CARTESIAN_POINT('Ctrl Pts',(3.4427580246746,-2.3215066538587,5.15184024742052));
#18899=CARTESIAN_POINT('Ctrl Pts',(3.43484901415926,-2.37607618365869,5.15554484377278));
#18900=CARTESIAN_POINT('Ctrl Pts',(3.4337081191144,-2.3839479782439,5.15607924129486));
#18901=CARTESIAN_POINT('Ctrl Pts',(3.43318582039731,-2.39190895914184,5.15661363881694));
#18902=CARTESIAN_POINT('Ctrl Pts',(3.43325215766083,-2.39987843114813,5.15714803633902));
#18903=CARTESIAN_POINT('Ctrl Pts',(3.54698297828114,-2.59851743256717,5.2));
#18904=CARTESIAN_POINT('Ctrl Pts',(3.48097120902544,-2.58088801151799,5.19629540364773));
#18905=CARTESIAN_POINT('Ctrl Pts',(3.36906717021742,-2.4748477879482,5.1888862109432));
#18906=CARTESIAN_POINT('Ctrl Pts',(3.41187708350278,-2.24617201703375,5.17777242188639));
#18907=CARTESIAN_POINT('Ctrl Pts',(3.62721323091929,-2.15871475485289,5.16665863282959));
#18908=CARTESIAN_POINT('Ctrl Pts',(3.81747535364037,-2.29190664293025,5.15554484377279));
#18909=CARTESIAN_POINT('Ctrl Pts',(3.80876232171537,-2.52413791100821,5.14443105471598));
#18910=CARTESIAN_POINT('Ctrl Pts',(3.60892556988421,-2.64269428158759,5.13331726565918));
#18911=CARTESIAN_POINT('Ctrl Pts',(3.40093972078443,-2.539134825312,5.12220347660237));
#18912=CARTESIAN_POINT('Ctrl Pts',(3.37514572416652,-2.30821119768585,5.11108968754557));
#18913=CARTESIAN_POINT('Ctrl Pts',(3.55516853033383,-2.16130913937078,5.09997589848876));
#18914=CARTESIAN_POINT('Ctrl Pts',(3.77622352465696,-2.23288041708187,5.08886210943196));
#18915=CARTESIAN_POINT('Ctrl Pts',(3.83598040928192,-2.457419700552,5.07774832037515));
#18916=CARTESIAN_POINT('Ctrl Pts',(3.67974110927284,-2.62940130358481,5.06663453131835));
#18917=CARTESIAN_POINT('Ctrl Pts',(3.45051418720664,-2.59140968013522,5.05552074226155));
#18918=CARTESIAN_POINT('Ctrl Pts',(3.35811316524308,-2.37821841178234,5.04440695320474));
#18919=CARTESIAN_POINT('Ctrl Pts',(3.48711398605093,-2.18496417501817,5.03329316414794));
#18920=CARTESIAN_POINT('Ctrl Pts',(3.71944061581356,-2.18853461914439,5.02217937509113));
#18921=CARTESIAN_POINT('Ctrl Pts',(3.84244191526684,-2.38566174871763,5.01106558603433));
#18922=CARTESIAN_POINT('Ctrl Pts',(3.74353337026135,-2.59591283022398,4.99995179697752));
#18923=CARTESIAN_POINT('Ctrl Pts',(3.51324710863985,-2.62684268245385,4.98883800792072));
#18924=CARTESIAN_POINT('Ctrl Pts',(3.36236674984584,-2.4501408518507,4.97772421886391));
#18925=CARTESIAN_POINT('Ctrl Pts',(3.42899480110061,-2.22754453241715,4.96661042980712));
#18926=CARTESIAN_POINT('Ctrl Pts',(3.65214584962031,-2.16279865748873,4.9554966407503));
#18927=CARTESIAN_POINT('Ctrl Pts',(3.82756721091734,-2.31516586178242,4.94438285169351));
#18928=CARTESIAN_POINT('Ctrl Pts',(3.79469372311971,-2.54518271468373,4.9332690626367));
#18929=CARTESIAN_POINT('Ctrl Pts',(3.58361486265069,-2.64231218244471,4.9221552735799));
#18930=CARTESIAN_POINT('Ctrl Pts',(3.38753350417909,-2.51765056156021,4.91104148452309));
#18931=CARTESIAN_POINT('Ctrl Pts',(3.38592513888554,-2.28530204745491,4.89992769546629));
#18932=CARTESIAN_POINT('Ctrl Pts',(3.5802619217345,-2.1579378700657,4.88881390640948));
#18933=CARTESIAN_POINT('Ctrl Pts',(3.7926651914697,-2.25213590538246,4.87770011735268));
#18934=CARTESIAN_POINT('Ctrl Pts',(3.8287198264784,-2.48167562339262,4.86658632829587));
#18935=CARTESIAN_POINT('Ctrl Pts',(3.65542461045338,-2.63645671704841,4.85547253923907));
#18936=CARTESIAN_POINT('Ctrl Pts',(3.43139861992193,-2.5748062959875,4.84435875018227));
#18937=CARTESIAN_POINT('Ctrl Pts',(3.36169538464595,-2.35315368977137,4.83324496112546));
#18938=CARTESIAN_POINT('Ctrl Pts',(3.51011506636152,-2.17438004258061,4.82213117206865));
#18939=CARTESIAN_POINT('Ctrl Pts',(3.74080744720095,-2.20211890112026,4.81101738301186));
#18940=CARTESIAN_POINT('Ctrl Pts',(3.84261717475225,-2.41098057358878,4.79990359395505));
#18941=CARTESIAN_POINT('Ctrl Pts',(3.72235665078693,-2.60979160252334,4.78878980489825));
#18942=CARTESIAN_POINT('Ctrl Pts',(3.49010169673754,-2.61657799846968,4.77767601584144));
#18943=CARTESIAN_POINT('Ctrl Pts',(3.3584379059958,-2.42512809625518,4.76656222678464));
#18944=CARTESIAN_POINT('Ctrl Pts',(3.44787863939658,-2.21067816256631,4.75544843772783));
#18945=CARTESIAN_POINT('Ctrl Pts',(3.67655777933124,-2.16951665373617,4.74433464867103));
#18946=CARTESIAN_POINT('Ctrl Pts',(3.83516271561975,-2.33931916560024,4.73322085961422));
#18947=CARTESIAN_POINT('Ctrl Pts',(3.77852055137491,-2.56466353335787,4.72210707055742));
#18948=CARTESIAN_POINT('Ctrl Pts',(3.55847650189588,-2.63928950162157,4.71099328150062));
#18949=CARTESIAN_POINT('Ctrl Pts',(3.37643938114003,-2.49489107532353,4.69987949244381));
#18950=CARTESIAN_POINT('Ctrl Pts',(3.39902983017658,-2.26363777164387,4.68876570338701));
#18951=CARTESIAN_POINT('Ctrl Pts',(3.60557055480924,-2.15719836203143,4.6776519143302));
#18952=CARTESIAN_POINT('Ctrl Pts',(3.8070124874506,-2.27299804520947,4.6665381252734));
#18953=CARTESIAN_POINT('Ctrl Pts',(3.81897354264718,-2.50504405790744,4.65542433621659));
#18954=CARTESIAN_POINT('Ctrl Pts',(3.63050563092984,-2.64094205312202,4.64431054715979));
#18955=CARTESIAN_POINT('Ctrl Pts',(3.4141155692652,-2.55630305464544,4.63319675810298));
#18956=CARTESIAN_POINT('Ctrl Pts',(3.3678676351246,-2.32859809765437,4.62208296904619));
#18957=CARTESIAN_POINT('Ctrl Pts',(3.53409308711521,-2.16624811163355,4.61096917998937));
#18958=CARTESIAN_POINT('Ctrl Pts',(3.76064388390312,-2.21785387995996,4.59985539093258));
#18959=CARTESIAN_POINT('Ctrl Pts',(3.8401555119317,-2.4361800576391,4.58874160187577));
#18960=CARTESIAN_POINT('Ctrl Pts',(3.69985007633495,-2.62139021824623,4.57762781281896));
#18961=CARTESIAN_POINT('Ctrl Pts',(3.46815073350293,-2.60395940136712,4.56651402376216));
#18962=CARTESIAN_POINT('Ctrl Pts',(3.35713451954606,-2.39984223133897,4.55540023470536));
#18963=CARTESIAN_POINT('Ctrl Pts',(3.46841583417461,-2.19586946879708,4.54428644564855));
#18964=CARTESIAN_POINT('Ctrl Pts',(3.70013762796088,-2.17873969637961,4.53317265659175));
#18965=CARTESIAN_POINT('Ctrl Pts',(3.84020231541317,-2.36413198929513,4.52205886753494));
#18966=CARTESIAN_POINT('Ctrl Pts',(3.7604070991348,-2.58235467884591,4.51094507847814));
#18967=CARTESIAN_POINT('Ctrl Pts',(3.53378944658573,-2.63366606347461,4.49983128942134));
#18968=CARTESIAN_POINT('Ctrl Pts',(3.36777506303883,-2.47110024891367,4.48871750036453));
#18969=CARTESIAN_POINT('Ctrl Pts',(3.41431880073856,-2.24345557286895,4.47760371130772));
#18970=CARTESIAN_POINT('Ctrl Pts',(3.63081864021225,-2.15909778094929,4.46648992225093));
#18971=CARTESIAN_POINT('Ctrl Pts',(3.81910984016012,-2.29524053287965,4.45537613319411));
#18972=CARTESIAN_POINT('Ctrl Pts',(3.80684729577664,-2.52727079162485,4.44426234413733));
#18973=CARTESIAN_POINT('Ctrl Pts',(3.60525512132335,-2.64280869447754,4.4331485550805));
#18974=CARTESIAN_POINT('Ctrl Pts',(3.39885278350865,-2.53610095948868,4.42203476602371));
#18975=CARTESIAN_POINT('Ctrl Pts',(3.37656295673162,-2.30481864526098,4.4109209769669));
#18976=CARTESIAN_POINT('Ctrl Pts',(3.55878722400007,-2.16065655916503,4.3998071879101));
#18977=CARTESIAN_POINT('Ctrl Pts',(3.77873474447839,-2.23556893008468,4.38869339885329));
#18978=CARTESIAN_POINT('Ctrl Pts',(3.83508286096032,-2.4609855401145,4.37757960979649));
#18979=CARTESIAN_POINT('Ctrl Pts',(3.67625990251943,-2.63058416437082,4.36646582073969));
#18980=CARTESIAN_POINT('Ctrl Pts',(3.44762951704948,-2.58912094093836,4.35535203168288));
#18981=CARTESIAN_POINT('Ctrl Pts',(3.35847732135144,-2.37456428079453,4.34423824262607));
#18982=CARTESIAN_POINT('Ctrl Pts',(3.49037003077072,-2.18326698967564,4.33312445356928));
#18983=CARTESIAN_POINT('Ctrl Pts',(3.72265543153543,-2.19039239422561,4.32201066451247));
#18984=CARTESIAN_POINT('Ctrl Pts',(3.84257847294968,-2.38928487404799,4.31089687545567));
#18985=CARTESIAN_POINT('Ctrl Pts',(3.74065691978671,-2.59816384879942,4.29978308639886));
#18986=CARTESIAN_POINT('Ctrl Pts',(3.50959628368763,-2.62529831625878,4.28866929734206));
#18987=CARTESIAN_POINT('Ctrl Pts',(3.41142456563631,-2.50643134569449,4.28126010463752));
#18988=CARTESIAN_POINT('Ctrl Pts',(3.39833241385534,-2.439372075429,4.27755550828525));
#18989=CARTESIAN_POINT('Ctrl Pts',(3.55032651029123,-2.58599788000028,5.20748149723825));
#18990=CARTESIAN_POINT('Ctrl Pts',(3.48847779011663,-2.5694802628904,5.20377690088598));
#18991=CARTESIAN_POINT('Ctrl Pts',(3.38363100808545,-2.4701274930924,5.19636770818144));
#18992=CARTESIAN_POINT('Ctrl Pts',(3.42374110325997,-2.25587321805223,5.18525391912464));
#18993=CARTESIAN_POINT('Ctrl Pts',(3.62549702156375,-2.17393147043888,5.17414013006783));
#18994=CARTESIAN_POINT('Ctrl Pts',(3.80376021494099,-2.29872357809039,5.16302634101103));
#18995=CARTESIAN_POINT('Ctrl Pts',(3.79559667259879,-2.51630912195772,5.15191255195423));
#18996=CARTESIAN_POINT('Ctrl Pts',(3.60836267654075,-2.62738870475875,5.14079876289742));
#18997=CARTESIAN_POINT('Ctrl Pts',(3.41349350811379,-2.53036025203219,5.12968497384062));
#18998=CARTESIAN_POINT('Ctrl Pts',(3.38932621647788,-2.31399988193773,5.11857118478382));
#18999=CARTESIAN_POINT('Ctrl Pts',(3.55799583841393,-2.17636223943479,5.10745739572701));
#19000=CARTESIAN_POINT('Ctrl Pts',(3.76510994308412,-2.24341985624469,5.09634360667021));
#19001=CARTESIAN_POINT('Ctrl Pts',(3.8210982445241,-2.45379851247728,5.0852298176134));
#19002=CARTESIAN_POINT('Ctrl Pts',(3.67471221585842,-2.61493405180745,5.0741160285566));
#19003=CARTESIAN_POINT('Ctrl Pts',(3.4599415481546,-2.57933837979007,5.0630022394998));
#19004=CARTESIAN_POINT('Ctrl Pts',(3.3733678202314,-2.37959207320419,5.05188845044299));
#19005=CARTESIAN_POINT('Ctrl Pts',(3.49423317134075,-2.19852546421989,5.04077466138618));
#19006=CARTESIAN_POINT('Ctrl Pts',(3.71190806288376,-2.20187073737575,5.02966087232939));
#19007=CARTESIAN_POINT('Ctrl Pts',(3.82715225398445,-2.38656599419535,5.01854708327258));
#19008=CARTESIAN_POINT('Ctrl Pts',(3.73448140162136,-2.58355753756882,5.00743329421578));
#19009=CARTESIAN_POINT('Ctrl Pts',(3.51871820188173,-2.61253679077134,4.99631950515897));
#19010=CARTESIAN_POINT('Ctrl Pts',(3.37735315143523,-2.44697870622763,4.98520571610217));
#19011=CARTESIAN_POINT('Ctrl Pts',(3.4397792876273,-2.23842048050862,4.97409192704536));
#19012=CARTESIAN_POINT('Ctrl Pts',(3.64885725830102,-2.17775782071235,4.96297813798855));
#19013=CARTESIAN_POINT('Ctrl Pts',(3.81321562666231,-2.3205159483675,4.95186434893175));
#19014=CARTESIAN_POINT('Ctrl Pts',(3.78241531376532,-2.53602672971665,4.94075055987495));
#19015=CARTESIAN_POINT('Ctrl Pts',(3.5846481955208,-2.62703070279587,4.92963677081815));
#19016=CARTESIAN_POINT('Ctrl Pts',(3.40093275798132,-2.51023089885891,4.91852298176134));
#19017=CARTESIAN_POINT('Ctrl Pts',(3.39942582465563,-2.29253550311487,4.90740919270454));
#19018=CARTESIAN_POINT('Ctrl Pts',(3.5815067086795,-2.17320358008914,4.89629540364773));
#19019=CARTESIAN_POINT('Ctrl Pts',(3.78051471198171,-2.26146099225962,4.88518161459093));
#19020=CARTESIAN_POINT('Ctrl Pts',(3.81429555222874,-2.47652472935135,4.87406782553412));
#19021=CARTESIAN_POINT('Ctrl Pts',(3.65192924324508,-2.6215445138197,4.86295403647732));
#19022=CARTESIAN_POINT('Ctrl Pts',(3.44203150900096,-2.56378209230252,4.85184024742051));
#19023=CARTESIAN_POINT('Ctrl Pts',(3.37672412605308,-2.35610806428593,4.84072645836371));
#19024=CARTESIAN_POINT('Ctrl Pts',(3.5157836826493,-2.18860882279666,4.8296126693069));
#19025=CARTESIAN_POINT('Ctrl Pts',(3.73192738959469,-2.2145983231407,4.8184988802501));
#19026=CARTESIAN_POINT('Ctrl Pts',(3.82731646068567,-2.41028808091203,4.8073850911933));
#19027=CARTESIAN_POINT('Ctrl Pts',(3.71464019736706,-2.59656104154983,4.79627130213649));
#19028=CARTESIAN_POINT('Ctrl Pts',(3.49703246129012,-2.60291945170324,4.78515751307969));
#19029=CARTESIAN_POINT('Ctrl Pts',(3.37367208112564,-2.42354338644957,4.77404372402289));
#19030=CARTESIAN_POINT('Ctrl Pts',(3.45747221184004,-2.22261779257846,4.76292993496608));
#19031=CARTESIAN_POINT('Ctrl Pts',(3.6717296434323,-2.18405214481133,4.75181614590928));
#19032=CARTESIAN_POINT('Ctrl Pts',(3.8203321189215,-2.34314601791364,4.74070235685247));
#19033=CARTESIAN_POINT('Ctrl Pts',(3.76726210722566,-2.55427898558761,4.72958856779567));
#19034=CARTESIAN_POINT('Ctrl Pts',(3.56109519190488,-2.62419864811054,4.71847477873887));
#19035=CARTESIAN_POINT('Ctrl Pts',(3.39053828864408,-2.4889067454323,4.70736098968206));
#19036=CARTESIAN_POINT('Ctrl Pts',(3.41170406524473,-2.2722374903888,4.69624720062525));
#19037=CARTESIAN_POINT('Ctrl Pts',(3.60521924634802,-2.17251070931785,4.68513341156845));
#19038=CARTESIAN_POINT('Ctrl Pts',(3.79395719207867,-2.28100745591228,4.67401962251165));
#19039=CARTESIAN_POINT('Ctrl Pts',(3.80516392027559,-2.49841942757747,4.66290583345484));
#19040=CARTESIAN_POINT('Ctrl Pts',(3.62858178552708,-2.6257469810287,4.65179204439804));
#19041=CARTESIAN_POINT('Ctrl Pts',(3.4258384183463,-2.54644576259963,4.64067825534124));
#19042=CARTESIAN_POINT('Ctrl Pts',(3.3825071219795,-2.3331010768549,4.62956446628443));
#19043=CARTESIAN_POINT('Ctrl Pts',(3.53824952340251,-2.18098973415088,4.61845067722763));
#19044=CARTESIAN_POINT('Ctrl Pts',(3.75051283635195,-2.22934097152269,4.60733688817082));
#19045=CARTESIAN_POINT('Ctrl Pts',(3.82501004325936,-2.43389835306723,4.59622309911402));
#19046=CARTESIAN_POINT('Ctrl Pts',(3.69355300577889,-2.607428187611,4.58510931005722));
#19047=CARTESIAN_POINT('Ctrl Pts',(3.47646584115605,-2.59109664964851,4.57399552100041));
#19048=CARTESIAN_POINT('Ctrl Pts',(3.37245089307511,-2.39985218105986,4.56288173194361));
#19049=CARTESIAN_POINT('Ctrl Pts',(3.47671422318619,-2.20874301286248,4.5517679428868));
#19050=CARTESIAN_POINT('Ctrl Pts',(3.69382242288812,-2.1926935339158,4.54065415383));
#19051=CARTESIAN_POINT('Ctrl Pts',(3.82505389506733,-2.36639401454743,4.52954036477319));
#19052=CARTESIAN_POINT('Ctrl Pts',(3.75029098447549,-2.57085443446884,4.51842657571639));
#19053=CARTESIAN_POINT('Ctrl Pts',(3.53796503204054,-2.61892985352599,4.50731278665959));
#19054=CARTESIAN_POINT('Ctrl Pts',(3.38242038797595,-2.46661629356384,4.49619899760278));
#19055=CARTESIAN_POINT('Ctrl Pts',(3.42602883297491,-2.25332808713219,4.48508520854598));
#19056=CARTESIAN_POINT('Ctrl Pts',(3.62887505479918,-2.17429034089672,4.47397141948917));
#19057=CARTESIAN_POINT('Ctrl Pts',(3.80529162215107,-2.30184721541898,4.46285763043237));
#19058=CARTESIAN_POINT('Ctrl Pts',(3.7938024182598,-2.51924442665844,4.45174384137557));
#19059=CARTESIAN_POINT('Ctrl Pts',(3.60492370575545,-2.62749590217058,4.44063005231876));
#19060=CARTESIAN_POINT('Ctrl Pts',(3.41153818407012,-2.52751771773158,4.42951626326196));
#19061=CARTESIAN_POINT('Ctrl Pts',(3.39065407090943,-2.31082128169766,4.41840247420515));
#19062=CARTESIAN_POINT('Ctrl Pts',(3.56138631824024,-2.17575081436632,4.40728868514835));
#19063=CARTESIAN_POINT('Ctrl Pts',(3.76746279218639,-2.24593881748859,4.39617489609154));
#19064=CARTESIAN_POINT('Ctrl Pts',(3.82025730031655,-2.4571394714574,4.38506110703474));
#19065=CARTESIAN_POINT('Ctrl Pts',(3.67145055229768,-2.61604231517601,4.37394731797793));
#19066=CARTESIAN_POINT('Ctrl Pts',(3.45723880045736,-2.57719398051498,4.36283352892113));
#19067=CARTESIAN_POINT('Ctrl Pts',(3.37370901074182,-2.37616839092003,4.35171973986433));
#19068=CARTESIAN_POINT('Ctrl Pts',(3.49728387276899,-2.19693531230428,4.34060595080752));
#19069=CARTESIAN_POINT('Ctrl Pts',(3.71492013543138,-2.20361135139717,4.32949216175072));
#19070=CARTESIAN_POINT('Ctrl Pts',(3.82728019962215,-2.38996062620176,4.31837837269391));
#19071=CARTESIAN_POINT('Ctrl Pts',(3.73178635523027,-2.58566659508311,4.30726458363711));
#19072=CARTESIAN_POINT('Ctrl Pts',(3.51529761713718,-2.61108982042464,4.29615079458031));
#19073=CARTESIAN_POINT('Ctrl Pts',(3.42331712354828,-2.49971922570605,4.28874160187577));
#19074=CARTESIAN_POINT('Ctrl Pts',(3.41105063166184,-2.43688906544027,4.2850370055235));
#19075=CARTESIAN_POINT('Ctrl Pts',(3.55367004230132,-2.57347832743338,5.2149629944765));
#19076=CARTESIAN_POINT('Ctrl Pts',(3.49598437120782,-2.55807251426281,5.21125839812423));
#19077=CARTESIAN_POINT('Ctrl Pts',(3.39819484595347,-2.4654071982366,5.2038492054197));
#19078=CARTESIAN_POINT('Ctrl Pts',(3.43560512301717,-2.2655744190707,5.19273541636288));
#19079=CARTESIAN_POINT('Ctrl Pts',(3.62378081220822,-2.18914818602487,5.18162162730609));
#19080=CARTESIAN_POINT('Ctrl Pts',(3.7900450762416,-2.30554051325052,5.17050783824928));
#19081=CARTESIAN_POINT('Ctrl Pts',(3.78243102348222,-2.50848033290724,5.15939404919248));
#19082=CARTESIAN_POINT('Ctrl Pts',(3.60779978319727,-2.6120831279299,5.14828026013567));
#19083=CARTESIAN_POINT('Ctrl Pts',(3.42604729544316,-2.52158567875239,5.13716647107887));
#19084=CARTESIAN_POINT('Ctrl Pts',(3.40350670878923,-2.3197885661896,5.12605268202206));
#19085=CARTESIAN_POINT('Ctrl Pts',(3.56082314649402,-2.19141533949881,5.11493889296526));
#19086=CARTESIAN_POINT('Ctrl Pts',(3.75399636151128,-2.25395929540751,5.10382510390846));
#19087=CARTESIAN_POINT('Ctrl Pts',(3.80621607976629,-2.45017732440257,5.09271131485166));
#19088=CARTESIAN_POINT('Ctrl Pts',(3.66968332244401,-2.60046680003009,5.08159752579485));
#19089=CARTESIAN_POINT('Ctrl Pts',(3.46936890910255,-2.56726707944493,5.07048373673804));
#19090=CARTESIAN_POINT('Ctrl Pts',(3.38862247521972,-2.38096573462603,5.05936994768124));
#19091=CARTESIAN_POINT('Ctrl Pts',(3.50135235663055,-2.21208675342161,5.04825615862443));
#19092=CARTESIAN_POINT('Ctrl Pts',(3.70437550995396,-2.2152068556071,5.03714236956763));
#19093=CARTESIAN_POINT('Ctrl Pts',(3.81186259270206,-2.38747023967307,5.02602858051083));
#19094=CARTESIAN_POINT('Ctrl Pts',(3.72542943298136,-2.57120224491366,5.01491479145402));
#19095=CARTESIAN_POINT('Ctrl Pts',(3.52418929512361,-2.59823089908883,5.00380100239722));
#19096=CARTESIAN_POINT('Ctrl Pts',(3.39233955302463,-2.44381656060457,4.99268721334042));
#19097=CARTESIAN_POINT('Ctrl Pts',(3.45056377415398,-2.24929642860009,4.98157342428361));
#19098=CARTESIAN_POINT('Ctrl Pts',(3.64556866698174,-2.19271698393598,4.97045963522681));
#19099=CARTESIAN_POINT('Ctrl Pts',(3.79886404240727,-2.32586603495258,4.95934584617));
#19100=CARTESIAN_POINT('Ctrl Pts',(3.77013690441093,-2.52687074474958,4.9482320571132));
#19101=CARTESIAN_POINT('Ctrl Pts',(3.58568152839091,-2.61174922314702,4.93711826805639));
#19102=CARTESIAN_POINT('Ctrl Pts',(3.41433201178354,-2.5028112361576,4.92600447899959));
#19103=CARTESIAN_POINT('Ctrl Pts',(3.41292651042572,-2.29976895877483,4.91489068994279));
#19104=CARTESIAN_POINT('Ctrl Pts',(3.58275149562449,-2.18846929011257,4.90377690088598));
#19105=CARTESIAN_POINT('Ctrl Pts',(3.76836423249372,-2.27078607913679,4.89266311182918));
#19106=CARTESIAN_POINT('Ctrl Pts',(3.79987127797908,-2.47137383531008,4.88154932277237));
#19107=CARTESIAN_POINT('Ctrl Pts',(3.64843387603678,-2.60663231059099,4.87043553371557));
#19108=CARTESIAN_POINT('Ctrl Pts',(3.45266439807998,-2.55275788861754,4.85932174465877));
#19109=CARTESIAN_POINT('Ctrl Pts',(3.39175286746021,-2.35906243880049,4.84820795560196));
#19110=CARTESIAN_POINT('Ctrl Pts',(3.52145229893708,-2.20283760301271,4.83709416654516));
#19111=CARTESIAN_POINT('Ctrl Pts',(3.72304733198844,-2.22707774516114,4.82598037748835));
#19112=CARTESIAN_POINT('Ctrl Pts',(3.81201574661908,-2.40959558823528,4.81486658843155));
#19113=CARTESIAN_POINT('Ctrl Pts',(3.7069237439472,-2.58333048057632,4.80375279937474));
#19114=CARTESIAN_POINT('Ctrl Pts',(3.50396322584271,-2.58926090493679,4.79263901031794));
#19115=CARTESIAN_POINT('Ctrl Pts',(3.38890625625548,-2.42195867664397,4.78152522126113));
#19116=CARTESIAN_POINT('Ctrl Pts',(3.46706578428349,-2.2345574225906,4.77041143220433));
#19117=CARTESIAN_POINT('Ctrl Pts',(3.66690150753336,-2.19858763588649,4.75929764314752));
#19118=CARTESIAN_POINT('Ctrl Pts',(3.80550152222325,-2.34697287022705,4.74818385409073));
#19119=CARTESIAN_POINT('Ctrl Pts',(3.75600366307642,-2.54389443781734,4.73707006503391));
#19120=CARTESIAN_POINT('Ctrl Pts',(3.56371388191388,-2.60910779459951,4.72595627597711));
#19121=CARTESIAN_POINT('Ctrl Pts',(3.40463719614813,-2.48292241554106,4.71484248692031));
#19122=CARTESIAN_POINT('Ctrl Pts',(3.42437830031288,-2.28083720913373,4.7037286978635));
#19123=CARTESIAN_POINT('Ctrl Pts',(3.60486793788679,-2.18782305660426,4.6926149088067));
#19124=CARTESIAN_POINT('Ctrl Pts',(3.78090189670674,-2.28901686661509,4.6815011197499));
#19125=CARTESIAN_POINT('Ctrl Pts',(3.79135429790399,-2.4917947972475,4.67038733069309));
#19126=CARTESIAN_POINT('Ctrl Pts',(3.62665794012432,-2.6105519089354,4.65927354163629));
#19127=CARTESIAN_POINT('Ctrl Pts',(3.43756126742739,-2.53658847055381,4.64815975257948));
#19128=CARTESIAN_POINT('Ctrl Pts',(3.3971466088344,-2.33760405605543,4.63704596352268));
#19129=CARTESIAN_POINT('Ctrl Pts',(3.54240595968981,-2.19573135666821,4.62593217446587));
#19130=CARTESIAN_POINT('Ctrl Pts',(3.74038178880077,-2.24082806308542,4.61481838540907));
#19131=CARTESIAN_POINT('Ctrl Pts',(3.80986457458702,-2.43161664849535,4.60370459635227));
#19132=CARTESIAN_POINT('Ctrl Pts',(3.68725593522283,-2.59346615697577,4.59259080729546));
#19133=CARTESIAN_POINT('Ctrl Pts',(3.48478094880917,-2.57823389792989,4.58147701823866));
#19134=CARTESIAN_POINT('Ctrl Pts',(3.38776726660417,-2.39986213078074,4.57036322918185));
#19135=CARTESIAN_POINT('Ctrl Pts',(3.48501261219776,-2.22161655692788,4.55924944012505));
#19136=CARTESIAN_POINT('Ctrl Pts',(3.68750721781536,-2.20664737145198,4.54813565106824));
#19137=CARTESIAN_POINT('Ctrl Pts',(3.80990547472148,-2.36865603979974,4.53702186201144));
#19138=CARTESIAN_POINT('Ctrl Pts',(3.74017486981618,-2.55935419009178,4.52590807295464));
#19139=CARTESIAN_POINT('Ctrl Pts',(3.54214061749534,-2.60419364357738,4.51479428389783));
#19140=CARTESIAN_POINT('Ctrl Pts',(3.39706571291307,-2.46213233821401,4.50368049484103));
#19141=CARTESIAN_POINT('Ctrl Pts',(3.43773886521125,-2.26320060139544,4.49256670578422));
#19142=CARTESIAN_POINT('Ctrl Pts',(3.62693146938611,-2.18948290084415,4.48145291672742));
#19143=CARTESIAN_POINT('Ctrl Pts',(3.79147340414203,-2.30845389795831,4.47033912767061));
#19144=CARTESIAN_POINT('Ctrl Pts',(3.78075754074296,-2.51121806169204,4.45922533861382));
#19145=CARTESIAN_POINT('Ctrl Pts',(3.60459229018754,-2.61218310986363,4.44811154955701));
#19146=CARTESIAN_POINT('Ctrl Pts',(3.42422358463158,-2.51893447597448,4.4369977605002));
#19147=CARTESIAN_POINT('Ctrl Pts',(3.40474518508724,-2.31682391813433,4.4258839714434));
#19148=CARTESIAN_POINT('Ctrl Pts',(3.56398541248042,-2.19084506956762,4.41477018238659));
#19149=CARTESIAN_POINT('Ctrl Pts',(3.75619083989438,-2.25630870489251,4.40365639332979));
#19150=CARTESIAN_POINT('Ctrl Pts',(3.80543173967279,-2.4532934028003,4.39254260427299));
#19151=CARTESIAN_POINT('Ctrl Pts',(3.66664120207593,-2.60150046598119,4.38142881521619));
#19152=CARTESIAN_POINT('Ctrl Pts',(3.46684808386524,-2.5652670200916,4.37031502615938));
#19153=CARTESIAN_POINT('Ctrl Pts',(3.3889407001322,-2.37777250104553,4.35920123710258));
#19154=CARTESIAN_POINT('Ctrl Pts',(3.50419771476727,-2.21060363493292,4.34808744804577));
#19155=CARTESIAN_POINT('Ctrl Pts',(3.70718483932733,-2.21683030856873,4.33697365898897));
#19156=CARTESIAN_POINT('Ctrl Pts',(3.81198192629463,-2.39063637835552,4.32585986993216));
#19157=CARTESIAN_POINT('Ctrl Pts',(3.72291579067381,-2.5731693413668,4.31474608087536));
#19158=CARTESIAN_POINT('Ctrl Pts',(3.52099895058674,-2.5968813245905,4.30363229181856));
#19159=CARTESIAN_POINT('Ctrl Pts',(3.43520968146025,-2.49300710571762,4.29622309911402));
#19160=CARTESIAN_POINT('Ctrl Pts',(3.42376884946835,-2.43440605545154,4.29251850276175));
#19161=CARTESIAN_POINT('Ctrl Pts',(3.55701357431141,-2.56095877486649,5.22244449171475));
#19162=CARTESIAN_POINT('Ctrl Pts',(3.50349095229901,-2.54666476563522,5.21873989536248));
#19163=CARTESIAN_POINT('Ctrl Pts',(3.41275868382149,-2.4606869033808,5.21133070265794));
#19164=CARTESIAN_POINT('Ctrl Pts',(3.44746914277437,-2.27527562008917,5.20021691360114));
#19165=CARTESIAN_POINT('Ctrl Pts',(3.62206460285268,-2.20436490161086,5.18910312454433));
#19166=CARTESIAN_POINT('Ctrl Pts',(3.77632993754221,-2.31235744841065,5.17798933548754));
#19167=CARTESIAN_POINT('Ctrl Pts',(3.76926537436564,-2.50065154385676,5.16687554643072));
#19168=CARTESIAN_POINT('Ctrl Pts',(3.6072368898538,-2.59677755110107,5.15576175737393));
#19169=CARTESIAN_POINT('Ctrl Pts',(3.43860108277253,-2.51281110547259,5.14464796831712));
#19170=CARTESIAN_POINT('Ctrl Pts',(3.41768720110058,-2.32557725044148,5.13353417926032));
#19171=CARTESIAN_POINT('Ctrl Pts',(3.56365045457412,-2.20646843956283,5.12242039020351));
#19172=CARTESIAN_POINT('Ctrl Pts',(3.74288277993844,-2.26449873457034,5.11130660114671));
#19173=CARTESIAN_POINT('Ctrl Pts',(3.79133391500848,-2.44655613632785,5.1001928120899));
#19174=CARTESIAN_POINT('Ctrl Pts',(3.66465442902959,-2.58599954825273,5.0890790230331));
#19175=CARTESIAN_POINT('Ctrl Pts',(3.4787962700505,-2.55519577909978,5.0779652339763));
#19176=CARTESIAN_POINT('Ctrl Pts',(3.40387713020803,-2.38233939604788,5.06685144491948));
#19177=CARTESIAN_POINT('Ctrl Pts',(3.50847154192036,-2.22564804262333,5.05573765586269));
#19178=CARTESIAN_POINT('Ctrl Pts',(3.69684295702416,-2.22854297383845,5.04462386680588));
#19179=CARTESIAN_POINT('Ctrl Pts',(3.79657293141967,-2.38837448515078,5.03351007774908));
#19180=CARTESIAN_POINT('Ctrl Pts',(3.71637746434136,-2.5588469522585,5.02239628869228));
#19181=CARTESIAN_POINT('Ctrl Pts',(3.52966038836549,-2.58392500740631,5.01128249963547));
#19182=CARTESIAN_POINT('Ctrl Pts',(3.40732595461402,-2.44065441498151,5.00016871057866));
#19183=CARTESIAN_POINT('Ctrl Pts',(3.46134826068067,-2.26017237669156,4.98905492152187));
#19184=CARTESIAN_POINT('Ctrl Pts',(3.64228007566245,-2.20767614715961,4.97794113246505));
#19185=CARTESIAN_POINT('Ctrl Pts',(3.78451245815223,-2.33121612153766,4.96682734340826));
#19186=CARTESIAN_POINT('Ctrl Pts',(3.75785849505654,-2.5177147597825,4.95571355435145));
#19187=CARTESIAN_POINT('Ctrl Pts',(3.58671486126101,-2.59646774349818,4.94459976529464));
#19188=CARTESIAN_POINT('Ctrl Pts',(3.42773126558577,-2.49539157345629,4.93348597623784));
#19189=CARTESIAN_POINT('Ctrl Pts',(3.4264271961958,-2.30700241443478,4.92237218718104));
#19190=CARTESIAN_POINT('Ctrl Pts',(3.5839962825695,-2.20373500013601,4.91125839812423));
#19191=CARTESIAN_POINT('Ctrl Pts',(3.75621375300573,-2.28011116601395,4.90014460906743));
#19192=CARTESIAN_POINT('Ctrl Pts',(3.78544700372942,-2.46622294126882,4.88903082001062));
#19193=CARTESIAN_POINT('Ctrl Pts',(3.64493850882848,-2.59172010736228,4.87791703095382));
#19194=CARTESIAN_POINT('Ctrl Pts',(3.463297287159,-2.54173368493256,4.86680324189701));
#19195=CARTESIAN_POINT('Ctrl Pts',(3.40678160886734,-2.36201681331505,4.85568945284021));
#19196=CARTESIAN_POINT('Ctrl Pts',(3.52712091522486,-2.21706638322876,4.8445756637834));
#19197=CARTESIAN_POINT('Ctrl Pts',(3.71416727438218,-2.23955716718158,4.8334618747266));
#19198=CARTESIAN_POINT('Ctrl Pts',(3.7967150325525,-2.40890309555853,4.8223480856698));
#19199=CARTESIAN_POINT('Ctrl Pts',(3.69920729052733,-2.57009991960281,4.81123429661299));
#19200=CARTESIAN_POINT('Ctrl Pts',(3.5108939903953,-2.57560235817033,4.80012050755619));
#19201=CARTESIAN_POINT('Ctrl Pts',(3.40414043138533,-2.42037396683837,4.78900671849938));
#19202=CARTESIAN_POINT('Ctrl Pts',(3.47665935672695,-2.24649705260274,4.77789292944258));
#19203=CARTESIAN_POINT('Ctrl Pts',(3.66207337163443,-2.21312312696165,4.76677914038577));
#19204=CARTESIAN_POINT('Ctrl Pts',(3.790670925525,-2.35079972254045,4.75566535132897));
#19205=CARTESIAN_POINT('Ctrl Pts',(3.74474521892717,-2.53350989004707,4.74455156227217));
#19206=CARTESIAN_POINT('Ctrl Pts',(3.56633257192288,-2.59401694108847,4.73343777321536));
#19207=CARTESIAN_POINT('Ctrl Pts',(3.41873610365217,-2.47693808564983,4.72232398415856));
#19208=CARTESIAN_POINT('Ctrl Pts',(3.43705253538103,-2.28943692787866,4.71121019510175));
#19209=CARTESIAN_POINT('Ctrl Pts',(3.60451662942557,-2.20313540389068,4.70009640604496));
#19210=CARTESIAN_POINT('Ctrl Pts',(3.76784660133481,-2.29702627731791,4.68898261698814));
#19211=CARTESIAN_POINT('Ctrl Pts',(3.7775446755324,-2.48517016691753,4.67786882793135));
#19212=CARTESIAN_POINT('Ctrl Pts',(3.62473409472155,-2.59535683684209,4.66675503887453));
#19213=CARTESIAN_POINT('Ctrl Pts',(3.44928411650849,-2.526731178508,4.65564124981774));
#19214=CARTESIAN_POINT('Ctrl Pts',(3.4117860956893,-2.34210703525596,4.64452746076092));
#19215=CARTESIAN_POINT('Ctrl Pts',(3.5465623959771,-2.21047297918554,4.63341367170413));
#19216=CARTESIAN_POINT('Ctrl Pts',(3.73025074124959,-2.25231515464815,4.62229988264732));
#19217=CARTESIAN_POINT('Ctrl Pts',(3.79471910591469,-2.42933494392347,4.61118609359052));
#19218=CARTESIAN_POINT('Ctrl Pts',(3.68095886466676,-2.57950412634054,4.60007230453372));
#19219=CARTESIAN_POINT('Ctrl Pts',(3.49309605646229,-2.56537114621128,4.5889585154769));
#19220=CARTESIAN_POINT('Ctrl Pts',(3.40308364013322,-2.39987208050163,4.57784472642011));
#19221=CARTESIAN_POINT('Ctrl Pts',(3.49331100120934,-2.23449010099328,4.56673093736329));
#19222=CARTESIAN_POINT('Ctrl Pts',(3.68119201274259,-2.22060120898816,4.5556171483065));
#19223=CARTESIAN_POINT('Ctrl Pts',(3.79475705437564,-2.37091806505204,4.54450335924969));
#19224=CARTESIAN_POINT('Ctrl Pts',(3.73005875515687,-2.5478539457147,4.53338957019289));
#19225=CARTESIAN_POINT('Ctrl Pts',(3.54631620295015,-2.58945743362876,4.52227578113609));
#19226=CARTESIAN_POINT('Ctrl Pts',(3.4117110378502,-2.45764838286418,4.51116199207927));
#19227=CARTESIAN_POINT('Ctrl Pts',(3.4494488974476,-2.27307311565868,4.50004820302248));
#19228=CARTESIAN_POINT('Ctrl Pts',(3.62498788397304,-2.20467546079158,4.48893441396567));
#19229=CARTESIAN_POINT('Ctrl Pts',(3.77765518613299,-2.31506058049763,4.47782062490887));
#19230=CARTESIAN_POINT('Ctrl Pts',(3.76771266322612,-2.50319169672563,4.46670683585206));
#19231=CARTESIAN_POINT('Ctrl Pts',(3.60426087461964,-2.59687031755667,4.45559304679526));
#19232=CARTESIAN_POINT('Ctrl Pts',(3.43690898519305,-2.51035123421737,4.44447925773846));
#19233=CARTESIAN_POINT('Ctrl Pts',(3.41883629926506,-2.32282655457101,4.43336546868165));
#19234=CARTESIAN_POINT('Ctrl Pts',(3.56658450672058,-2.20593932476892,4.42225167962485));
#19235=CARTESIAN_POINT('Ctrl Pts',(3.74491888760239,-2.26667859229642,4.41113789056804));
#19236=CARTESIAN_POINT('Ctrl Pts',(3.79060617902903,-2.4494473341432,4.40002410151123));
#19237=CARTESIAN_POINT('Ctrl Pts',(3.66183185185417,-2.58695861678637,4.38891031245443));
#19238=CARTESIAN_POINT('Ctrl Pts',(3.47645736727312,-2.55334005966823,4.37779652339763));
#19239=CARTESIAN_POINT('Ctrl Pts',(3.40417238952257,-2.37937661117104,4.36668273434082));
#19240=CARTESIAN_POINT('Ctrl Pts',(3.51111155676555,-2.22427195756156,4.35556894528402));
#19241=CARTESIAN_POINT('Ctrl Pts',(3.69944954322327,-2.2300492657403,4.34445515622722));
#19242=CARTESIAN_POINT('Ctrl Pts',(3.79668365296711,-2.39131213050928,4.33334136717041));
#19243=CARTESIAN_POINT('Ctrl Pts',(3.71404522611737,-2.56067208765049,4.32222757811361));
#19244=CARTESIAN_POINT('Ctrl Pts',(3.5267002840363,-2.58267282875636,4.31111378905681));
#19245=CARTESIAN_POINT('Ctrl Pts',(3.44710223937223,-2.48629498572918,4.30370459635227));
#19246=CARTESIAN_POINT('Ctrl Pts',(3.43648706727485,-2.43192304546281,4.3));
#19247=CARTESIAN_POINT('Ctrl Pts',(3.43361559198215,-2.39990578567643,5.13785196366098));
#19248=CARTESIAN_POINT('Ctrl Pts',(3.43350388051965,-2.378317282854,5.13641270219409));
#19249=CARTESIAN_POINT('Ctrl Pts',(3.43740296507651,-2.35676746744261,5.1349734407272));
#19250=CARTESIAN_POINT('Ctrl Pts',(3.44550005695817,-2.33693142446689,5.13353417926032));
#19251=CARTESIAN_POINT('Ctrl Pts',(3.4663416189251,-2.28587431348193,5.12982958290805));
#19252=CARTESIAN_POINT('Ctrl Pts',(3.51499603674961,-2.24617137652238,5.12612498655578));
#19253=CARTESIAN_POINT('Ctrl Pts',(3.56919529988925,-2.23599162387719,5.12242039020351));
#19254=CARTESIAN_POINT('Ctrl Pts',(3.62339456302889,-2.225811871232,5.11871579385124));
#19255=CARTESIAN_POINT('Ctrl Pts',(3.68313867148366,-2.24515530290117,5.11501119749898));
#19256=CARTESIAN_POINT('Ctrl Pts',(3.72108591488939,-2.28516991902867,5.11130660114671));
#19257=CARTESIAN_POINT('Ctrl Pts',(3.75903315829512,-2.32518453515617,5.10760200479444));
#19258=CARTESIAN_POINT('Ctrl Pts',(3.7751835366518,-2.38587033574201,5.10389740844217));
#19259=CARTESIAN_POINT('Ctrl Pts',(3.76214547816699,-2.43945380468907,5.1001928120899));
#19260=CARTESIAN_POINT('Ctrl Pts',(3.74910741968218,-2.49303727363614,5.09648821573763));
#19261=CARTESIAN_POINT('Ctrl Pts',(3.70688092435589,-2.53951841094443,5.09278361938536));
#19262=CARTESIAN_POINT('Ctrl Pts',(3.65479131686289,-2.55762501807309,5.0890790230331));
#19263=CARTESIAN_POINT('Ctrl Pts',(3.60270170936989,-2.57573162520175,5.08537442668083));
#19264=CARTESIAN_POINT('Ctrl Pts',(3.5407489897102,-2.56546370215076,5.08166983032856));
#19265=CARTESIAN_POINT('Ctrl Pts',(3.49728610657327,-2.53152034344996,5.0779652339763));
#19266=CARTESIAN_POINT('Ctrl Pts',(3.45773596902793,-2.50063273525474,5.07459414387119));
#19267=CARTESIAN_POINT('Ctrl Pts',(3.43349642418942,-2.45014057555659,5.07122305376608));
#19268=CARTESIAN_POINT('Ctrl Pts',(3.43317939237559,-2.39991359865598,5.06785196366098));
#19269=CARTESIAN_POINT('Ctrl Pts',(3.54698297828114,-2.59851743256717,5.2));
#19270=CARTESIAN_POINT('Ctrl Pts',(3.53457951946873,-2.59392489162072,5.2));
#19271=CARTESIAN_POINT('Ctrl Pts',(3.52273021669441,-2.5880656264448,5.2));
#19272=CARTESIAN_POINT('Ctrl Pts',(3.51155282078554,-2.58110287559691,5.2));
#19273=CARTESIAN_POINT('Ctrl Pts',(3.50588661273558,-2.57757321670087,5.2));
#19274=CARTESIAN_POINT('Ctrl Pts',(3.50039351027032,-2.5737592340707,5.2));
#19275=CARTESIAN_POINT('Ctrl Pts',(3.49509228904167,-2.56967861696227,5.2));
#19276=CARTESIAN_POINT('Ctrl Pts',(3.4905050126104,-2.5661475591401,5.2));
#19277=CARTESIAN_POINT('Ctrl Pts',(3.48606143928385,-2.56241679614242,5.2));
#19278=CARTESIAN_POINT('Ctrl Pts',(3.48177554227615,-2.55849690369355,5.2));
#19279=CARTESIAN_POINT('Ctrl Pts',(3.47866533036506,-2.55565229586402,5.2));
#19280=CARTESIAN_POINT('Ctrl Pts',(3.47564434245519,-2.5527135073757,5.2));
#19281=CARTESIAN_POINT('Ctrl Pts',(3.47272197556915,-2.54969075241385,5.2));
#19282=CARTESIAN_POINT('Ctrl Pts',(3.4637769959157,-2.54043849809891,5.2));
#19283=CARTESIAN_POINT('Ctrl Pts',(3.45573629551605,-2.5303863939551,5.2));
#19284=CARTESIAN_POINT('Ctrl Pts',(3.44873891503949,-2.51966547725229,5.2));
#19285=CARTESIAN_POINT('Ctrl Pts',(3.44420807340926,-2.51272362581603,5.2));
#19286=CARTESIAN_POINT('Ctrl Pts',(3.44011549441187,-2.50550078770205,5.2));
#19287=CARTESIAN_POINT('Ctrl Pts',(3.43651065828778,-2.49802988469159,5.2));
#19288=CARTESIAN_POINT('Ctrl Pts',(3.43484392828386,-2.49457564217533,5.2));
#19289=CARTESIAN_POINT('Ctrl Pts',(3.43328559790363,-2.49107645830187,5.2));
#19290=CARTESIAN_POINT('Ctrl Pts',(3.43184079842385,-2.48753928615204,5.2));
#19291=CARTESIAN_POINT('Ctrl Pts',(3.4278386851231,-2.47774127341323,5.2));
#19292=CARTESIAN_POINT('Ctrl Pts',(3.42470153714545,-2.46764377419319,5.2));
#19293=CARTESIAN_POINT('Ctrl Pts',(3.42252346903458,-2.4573201729425,5.2));
#19294=CARTESIAN_POINT('Ctrl Pts',(3.42066967900374,-2.44853358404506,5.2));
#19295=CARTESIAN_POINT('Ctrl Pts',(3.41951138514856,-2.43958272486992,5.2));
#19296=CARTESIAN_POINT('Ctrl Pts',(3.4190359581172,-2.43054589510015,5.2));
#19297=CARTESIAN_POINT('Ctrl Pts',(3.41886681623208,-2.42733087718605,5.2));
#19298=CARTESIAN_POINT('Ctrl Pts',(3.41878446710974,-2.42410641682356,5.2));
#19299=CARTESIAN_POINT('Ctrl Pts',(3.4187879805801,-2.42088574908536,5.2));
#19300=CARTESIAN_POINT('Ctrl Pts',(3.41880075373106,-2.40917707615745,5.2));
#19301=CARTESIAN_POINT('Ctrl Pts',(3.41994281751926,-2.39748218187535,5.2));
#19302=CARTESIAN_POINT('Ctrl Pts',(3.42216878576612,-2.38597338048412,5.2));
#19303=CARTESIAN_POINT('Ctrl Pts',(3.42331180295367,-2.38006370148633,5.2));
#19304=CARTESIAN_POINT('Ctrl Pts',(3.4247413109463,-2.37420327369848,5.2));
#19305=CARTESIAN_POINT('Ctrl Pts',(3.42645509270942,-2.36841769265549,5.2));
#19306=CARTESIAN_POINT('Ctrl Pts',(3.42814232412983,-2.36272174330468,5.2));
#19307=CARTESIAN_POINT('Ctrl Pts',(3.430107844827,-2.35709290248798,5.2));
#19308=CARTESIAN_POINT('Ctrl Pts',(3.43233768211765,-2.35158848883877,5.2));
#19309=CARTESIAN_POINT('Ctrl Pts',(3.43579440103488,-2.34305548471816,5.2));
#19310=CARTESIAN_POINT('Ctrl Pts',(3.4398879741905,-2.33480787202203,5.2));
#19311=CARTESIAN_POINT('Ctrl Pts',(3.44460905895211,-2.32694151527758,5.2));
#19312=CARTESIAN_POINT('Ctrl Pts',(3.44702307993388,-2.32291922989401,5.2));
#19313=CARTESIAN_POINT('Ctrl Pts',(3.44960209197192,-2.31899653386197,5.2));
#19314=CARTESIAN_POINT('Ctrl Pts',(3.45233605539852,-2.31519993624376,5.2));
#19315=CARTESIAN_POINT('Ctrl Pts',(3.45777066118573,-2.30765301327221,5.2));
#19316=CARTESIAN_POINT('Ctrl Pts',(3.46382416246759,-2.30058959612096,5.2));
#19317=CARTESIAN_POINT('Ctrl Pts',(3.47049190863519,-2.29412081302041,5.2));
#19318=CARTESIAN_POINT('Ctrl Pts',(3.47127037804276,-2.29336557285059,5.2));
#19319=CARTESIAN_POINT('Ctrl Pts',(3.472057234472,-2.29261846360327,5.2));
#19320=CARTESIAN_POINT('Ctrl Pts',(3.47285232078577,-2.29187955100915,5.2));
#19321=CARTESIAN_POINT('Origin',(3.6,-2.4,4.7));
#19322=CARTESIAN_POINT('Origin',(3.6,2.4,4.3));
#19323=CARTESIAN_POINT('Ctrl Pts',(3.43648706727485,2.36807695453719,4.3));
#19324=CARTESIAN_POINT('Ctrl Pts',(3.43713128683271,2.3597806326638,4.3));
#19325=CARTESIAN_POINT('Ctrl Pts',(3.43844439010238,2.35157023568352,4.3));
#19326=CARTESIAN_POINT('Ctrl Pts',(3.44036779366958,2.34349709838219,4.3));
#19327=CARTESIAN_POINT('Ctrl Pts',(3.44142971905211,2.33903985936946,4.3));
#19328=CARTESIAN_POINT('Ctrl Pts',(3.44267796535882,2.33462439474099,4.3));
#19329=CARTESIAN_POINT('Ctrl Pts',(3.44410466805123,2.33025917432088,4.3));
#19330=CARTESIAN_POINT('Ctrl Pts',(3.44564438355751,2.32554817349018,4.3));
#19331=CARTESIAN_POINT('Ctrl Pts',(3.44738955334548,2.3209035962062,4.3));
#19332=CARTESIAN_POINT('Ctrl Pts',(3.4493265481332,2.31634215395336,4.3));
#19333=CARTESIAN_POINT('Ctrl Pts',(3.45254731917628,2.30875753823018,4.3));
#19334=CARTESIAN_POINT('Ctrl Pts',(3.45629959311852,2.30139710694769,4.3));
#19335=CARTESIAN_POINT('Ctrl Pts',(3.46054037353588,2.29430908064149,4.3));
#19336=CARTESIAN_POINT('Ctrl Pts',(3.46239353776121,2.29121170810954,4.3));
#19337=CARTESIAN_POINT('Ctrl Pts',(3.46433984867298,2.28816727138872,4.3));
#19338=CARTESIAN_POINT('Ctrl Pts',(3.46636983737831,2.28518826034786,4.3));
#19339=CARTESIAN_POINT('Ctrl Pts',(3.47324583140019,2.27509773026055,4.3));
#19340=CARTESIAN_POINT('Ctrl Pts',(3.48109365784268,2.26572974302294,4.3));
#19341=CARTESIAN_POINT('Ctrl Pts',(3.48977951837809,2.25723278343533,4.3));
#19342=CARTESIAN_POINT('Ctrl Pts',(3.49400932884437,2.25309496330239,4.3));
#19343=CARTESIAN_POINT('Ctrl Pts',(3.49843865454892,2.24916389122995,4.3));
#19344=CARTESIAN_POINT('Ctrl Pts',(3.50305598018317,2.24545876796073,4.3));
#19345=CARTESIAN_POINT('Ctrl Pts',(3.50696193979743,2.24232447269942,4.3));
#19346=CARTESIAN_POINT('Ctrl Pts',(3.51100698863209,2.23934939909905,4.3));
#19347=CARTESIAN_POINT('Ctrl Pts',(3.51515874429581,2.23656266075085,4.3));
#19348=CARTESIAN_POINT('Ctrl Pts',(3.52023402885856,2.23315603202204,4.3));
#19349=CARTESIAN_POINT('Ctrl Pts',(3.52547424287705,2.23002554171617,4.3));
#19350=CARTESIAN_POINT('Ctrl Pts',(3.53086412680946,2.22718930631114,4.3));
#19351=CARTESIAN_POINT('Ctrl Pts',(3.53843721702836,2.22320423596943,4.3));
#19352=CARTESIAN_POINT('Ctrl Pts',(3.54630546669305,2.21979946806346,4.3));
#19353=CARTESIAN_POINT('Ctrl Pts',(3.55440208317939,2.21695927394856,4.3));
#19354=CARTESIAN_POINT('Ctrl Pts',(3.56031223293849,2.21488606564082,4.3));
#19355=CARTESIAN_POINT('Ctrl Pts',(3.56634429400461,2.21311389140606,4.3));
#19356=CARTESIAN_POINT('Ctrl Pts',(3.57247452264395,2.21164027909917,4.3));
#19357=CARTESIAN_POINT('Ctrl Pts',(3.57600246534631,2.21079221614916,4.3));
#19358=CARTESIAN_POINT('Ctrl Pts',(3.57955843058062,2.21004433773534,4.3));
#19359=CARTESIAN_POINT('Ctrl Pts',(3.58312961367547,2.20939690917763,4.3));
#19360=CARTESIAN_POINT('Ctrl Pts',(3.59464652648698,2.20730897975681,4.3));
#19361=CARTESIAN_POINT('Ctrl Pts',(3.60634454881448,2.20625732608158,4.3));
#19362=CARTESIAN_POINT('Ctrl Pts',(3.61806689528204,2.2062086557371,4.3));
#19363=CARTESIAN_POINT('Ctrl Pts',(3.62473122101744,2.20618098593309,4.3));
#19364=CARTESIAN_POINT('Ctrl Pts',(3.63140379711974,2.20647808078856,4.3));
#19365=CARTESIAN_POINT('Ctrl Pts',(3.63805748358195,2.20709863975089,4.3));
#19366=CARTESIAN_POINT('Ctrl Pts',(3.64215439115276,2.20748073961769,4.3));
#19367=CARTESIAN_POINT('Ctrl Pts',(3.64624620849006,2.20798586737994,4.3));
#19368=CARTESIAN_POINT('Ctrl Pts',(3.65032009844121,2.20861337585159,4.3));
#19369=CARTESIAN_POINT('Ctrl Pts',(3.66357602962435,2.2106552103677,4.3));
#19370=CARTESIAN_POINT('Ctrl Pts',(3.67655558408475,2.21397441829708,4.3));
#19371=CARTESIAN_POINT('Ctrl Pts',(3.68904456814691,2.21853837010126,4.3));
#19372=CARTESIAN_POINT('Ctrl Pts',(3.69937753051516,2.22231442922732,4.3));
#19373=CARTESIAN_POINT('Ctrl Pts',(3.7093756794575,2.22694342372598,4.3));
#19374=CARTESIAN_POINT('Ctrl Pts',(3.71891590137671,2.23243384744346,4.3));
#19375=CARTESIAN_POINT('Ctrl Pts',(3.72007018093634,2.23309813847615,4.3));
#19376=CARTESIAN_POINT('Ctrl Pts',(3.72121774557788,2.23377506987061,4.3));
#19377=CARTESIAN_POINT('Ctrl Pts',(3.72235851517116,2.23446447326396,4.3));
#19378=CARTESIAN_POINT('Ctrl Pts',(3.78826275096636,2.31767678198967,4.3));
#19379=CARTESIAN_POINT('Ctrl Pts',(3.79091867322995,2.32572936860323,4.3));
#19380=CARTESIAN_POINT('Ctrl Pts',(3.79302804064853,2.33393960507108,4.3));
#19381=CARTESIAN_POINT('Ctrl Pts',(3.79460323981381,2.34225613442594,4.3));
#19382=CARTESIAN_POINT('Ctrl Pts',(3.79578956453863,2.34851953566168,4.3));
#19383=CARTESIAN_POINT('Ctrl Pts',(3.79667271897105,2.35484328449916,4.3));
#19384=CARTESIAN_POINT('Ctrl Pts',(3.79725488312451,2.36120517356094,4.3));
#19385=CARTESIAN_POINT('Ctrl Pts',(3.7976908683603,2.36596961961323,4.3));
#19386=CARTESIAN_POINT('Ctrl Pts',(3.79795758133253,2.37075408813906,4.3));
#19387=CARTESIAN_POINT('Ctrl Pts',(3.79805590956906,2.3755369878883,4.3));
#19388=CARTESIAN_POINT('Ctrl Pts',(3.79826159173226,2.3855418166282,4.3));
#19389=CARTESIAN_POINT('Ctrl Pts',(3.79773306912215,2.39555473221079,4.3));
#19390=CARTESIAN_POINT('Ctrl Pts',(3.79647804098653,2.40548740413607,4.3));
#19391=CARTESIAN_POINT('Ctrl Pts',(3.79582247707096,2.41067573507037,4.3));
#19392=CARTESIAN_POINT('Ctrl Pts',(3.79496739950913,2.41584508273998,4.3));
#19393=CARTESIAN_POINT('Ctrl Pts',(3.79391843118089,2.42095777287915,4.3));
#19394=CARTESIAN_POINT('Ctrl Pts',(3.79135148096571,2.43346913351755,4.3));
#19395=CARTESIAN_POINT('Ctrl Pts',(3.78762422716575,2.44567369959671,4.3));
#19396=CARTESIAN_POINT('Ctrl Pts',(3.78275033841106,2.45738291584384,4.3));
#19397=CARTESIAN_POINT('Ctrl Pts',(3.78051276867504,2.46275853872441,4.3));
#19398=CARTESIAN_POINT('Ctrl Pts',(3.77803290925375,2.46802940870032,4.3));
#19399=CARTESIAN_POINT('Ctrl Pts',(3.77530915968311,2.47317482247228,4.3));
#19400=CARTESIAN_POINT('Ctrl Pts',(3.7735285304889,2.4765385950002,4.3));
#19401=CARTESIAN_POINT('Ctrl Pts',(3.77164255910733,2.47985045045176,4.3));
#19402=CARTESIAN_POINT('Ctrl Pts',(3.76965384065618,2.48309856403818,4.3));
#19403=CARTESIAN_POINT('Ctrl Pts',(3.76538142018115,2.49007657894212,4.3));
#19404=CARTESIAN_POINT('Ctrl Pts',(3.76065254798511,2.4967339395313,4.3));
#19405=CARTESIAN_POINT('Ctrl Pts',(3.75546934621649,2.50301830246242,4.3));
#19406=CARTESIAN_POINT('Ctrl Pts',(3.7497639943478,2.5099357452696,4.3));
#19407=CARTESIAN_POINT('Ctrl Pts',(3.74350797317419,2.51640155748529,4.3));
#19408=CARTESIAN_POINT('Ctrl Pts',(3.73677354924283,2.52238273959095,4.3));
#19409=CARTESIAN_POINT('Ctrl Pts',(3.73252952287629,2.52615207380843,4.3));
#19410=CARTESIAN_POINT('Ctrl Pts',(3.72809532803267,2.52972869286917,4.3));
#19411=CARTESIAN_POINT('Ctrl Pts',(3.72348818609076,2.53310156466662,4.3));
#19412=CARTESIAN_POINT('Ctrl Pts',(3.72067461067475,2.53516137295782,4.3));
#19413=CARTESIAN_POINT('Ctrl Pts',(3.71779994290363,2.53714246961825,4.3));
#19414=CARTESIAN_POINT('Ctrl Pts',(3.71487521534485,2.53903869288715,4.3));
#19415=CARTESIAN_POINT('Ctrl Pts',(3.70626340571031,2.54462208945595,4.3));
#19416=CARTESIAN_POINT('Ctrl Pts',(3.69720115342902,2.54948407839451,4.3));
#19417=CARTESIAN_POINT('Ctrl Pts',(3.68779739443943,2.55357358531277,4.3));
#19418=CARTESIAN_POINT('Ctrl Pts',(3.67897143105616,2.55741182046492,4.3));
#19419=CARTESIAN_POINT('Ctrl Pts',(3.66984396791867,2.56056952878093,4.3));
#19420=CARTESIAN_POINT('Ctrl Pts',(3.66050457512214,2.56298263453418,4.3));
#19421=CARTESIAN_POINT('Ctrl Pts',(3.657017355811,2.56388365981129,4.3));
#19422=CARTESIAN_POINT('Ctrl Pts',(3.65350912975721,2.56467838913094,4.3));
#19423=CARTESIAN_POINT('Ctrl Pts',(3.64998789179307,2.5653638764114,4.3));
#19424=CARTESIAN_POINT('Ctrl Pts',(3.63890668202576,2.56752108033372,4.3));
#19425=CARTESIAN_POINT('Ctrl Pts',(3.62768560566387,2.56860271836266,4.3));
#19426=CARTESIAN_POINT('Ctrl Pts',(3.61647526972934,2.56851225659508,4.3));
#19427=CARTESIAN_POINT('Ctrl Pts',(3.61029339424358,2.56846237197194,4.3));
#19428=CARTESIAN_POINT('Ctrl Pts',(3.60411488972487,2.56805522437202,4.3));
#19429=CARTESIAN_POINT('Ctrl Pts',(3.59796731823988,2.56726810386747,4.3));
#19430=CARTESIAN_POINT('Ctrl Pts',(3.5968916538024,2.56713037833848,4.3));
#19431=CARTESIAN_POINT('Ctrl Pts',(3.59581694274575,2.56698100748364,4.3));
#19432=CARTESIAN_POINT('Ctrl Pts',(3.59474333802771,2.56682006235004,4.3));
#19433=CARTESIAN_POINT('Origin',(3.6,2.4,5.35459252805377));
#19434=CARTESIAN_POINT('Ctrl Pts',(3.39434265438876,2.4001499379742,5.17959252805377));
#19435=CARTESIAN_POINT('Ctrl Pts',(3.3942608381295,2.40997903394326,5.17905813053169));
#19436=CARTESIAN_POINT('Ctrl Pts',(3.39937061019979,2.4878631610827,5.17481913665734));
#19437=CARTESIAN_POINT('Ctrl Pts',(3.4989044460774,2.62084298387434,5.16687554643073));
#19438=CARTESIAN_POINT('Ctrl Pts',(3.73070050850364,2.60468899581803,5.15576175737391));
#19439=CARTESIAN_POINT('Ctrl Pts',(3.84286218134804,2.40121305191012,5.14464796831713));
#19440=CARTESIAN_POINT('Ctrl Pts',(3.73273070961532,2.19661070737624,5.1335341792603));
#19441=CARTESIAN_POINT('Ctrl Pts',(3.50110863285869,2.17818091869864,5.12242039020352));
#19442=CARTESIAN_POINT('Ctrl Pts',(3.39978420373419,2.31073763553012,5.11443983980133));
#19443=CARTESIAN_POINT('Ctrl Pts',(3.39427096205728,2.38932589106744,5.11016388575141));
#19444=CARTESIAN_POINT('Ctrl Pts',(3.39436118415265,2.39983962587988,5.10959252805377));
#19445=CARTESIAN_POINT('Ctrl Pts',(3.39473291096846,2.39977036782444,5.18540747194623));
#19446=CARTESIAN_POINT('Ctrl Pts',(3.39508769603641,2.44679019469361,5.18286245525962));
#19447=CARTESIAN_POINT('Ctrl Pts',(3.43434460318779,2.56295297845058,5.17661284222074));
#19448=CARTESIAN_POINT('Ctrl Pts',(3.62721323264599,2.64128528195604,5.16665863282959));
#19449=CARTESIAN_POINT('Ctrl Pts',(3.81747536314189,2.50809334538988,5.15554484377278));
#19450=CARTESIAN_POINT('Ctrl Pts',(3.80876232811303,2.27586209318291,5.14443105471598));
#19451=CARTESIAN_POINT('Ctrl Pts',(3.60892557137656,2.15730570431671,5.13331726565918));
#19452=CARTESIAN_POINT('Ctrl Pts',(3.42787436374214,2.24745398081386,5.12364273806926));
#19453=CARTESIAN_POINT('Ctrl Pts',(3.39500774851697,2.35820797614884,5.11767280683161));
#19454=CARTESIAN_POINT('Ctrl Pts',(3.39479089114249,2.40011619889285,5.11540747194623));
#19455=CARTESIAN_POINT('Ctrl Pts',(3.72690708798524,2.50793586530485,5.2));
#19456=CARTESIAN_POINT('Ctrl Pts',(3.76279833110066,2.46573623930395,5.19629540364773));
#19457=CARTESIAN_POINT('Ctrl Pts',(3.78852074717293,2.34341311981147,5.1888862109432));
#19458=CARTESIAN_POINT('Ctrl Pts',(3.65451258117961,2.21065853310285,5.17777242188639));
#19459=CARTESIAN_POINT('Ctrl Pts',(3.47057722493071,2.25164322990955,5.16665863282959));
#19460=CARTESIAN_POINT('Ctrl Pts',(3.405121385579,2.4282098150683,5.15554484377278));
#19461=CARTESIAN_POINT('Ctrl Pts',(3.5180312968317,2.57906042639477,5.14443105471598));
#19462=CARTESIAN_POINT('Ctrl Pts',(3.70597252569269,2.56596270448124,5.13331726565917));
#19463=CARTESIAN_POINT('Ctrl Pts',(3.79691368493775,2.4009835476249,5.12220347660237));
#19464=CARTESIAN_POINT('Ctrl Pts',(3.70761862135009,2.23509110037173,5.11108968754557));
#19465=CARTESIAN_POINT('Ctrl Pts',(3.51981846080671,2.22014814967852,5.09997589848877));
#19466=CARTESIAN_POINT('Ctrl Pts',(3.40540964822557,2.3698223862213,5.08886210943195));
#19467=CARTESIAN_POINT('Ctrl Pts',(3.46911145369901,2.54712015828428,5.07774832037516));
#19468=CARTESIAN_POINT('Ctrl Pts',(3.65261709875363,2.58975637037653,5.06663453131834));
#19469=CARTESIAN_POINT('Ctrl Pts',(3.78796168225801,2.4587068294695,5.05552074226155));
#19470=CARTESIAN_POINT('Ctrl Pts',(3.75126282351006,2.27392205963726,5.04440695320474));
#19471=CARTESIAN_POINT('Ctrl Pts',(3.576111378403,2.20453795937386,5.03329316414794));
#19472=CARTESIAN_POINT('Ctrl Pts',(3.42282546383512,2.31406243118482,5.02217937509113));
#19473=CARTESIAN_POINT('Ctrl Pts',(3.43170940937961,2.50224655949829,5.01106558603433));
#19474=CARTESIAN_POINT('Ctrl Pts',(3.59463164213028,2.59684323978071,4.99995179697753));
#19475=CARTESIAN_POINT('Ctrl Pts',(3.762467593188,2.51126707661319,4.98883800792072));
#19476=CARTESIAN_POINT('Ctrl Pts',(3.78159511395878,2.32384689323348,4.97772421886391));
#19477=CARTESIAN_POINT('Ctrl Pts',(3.63450656736167,2.20613051367693,4.96661042980712));
#19478=CARTESIAN_POINT('Ctrl Pts',(3.45583376839362,2.26586507280002,4.95549664075031));
#19479=CARTESIAN_POINT('Ctrl Pts',(3.40911795613805,2.44837485237297,4.94438285169351));
#19480=CARTESIAN_POINT('Ctrl Pts',(3.53711864339547,2.58660658076597,4.9332690626367));
#19481=CARTESIAN_POINT('Ctrl Pts',(3.72267534946784,2.5540351896186,4.9221552735799));
#19482=CARTESIAN_POINT('Ctrl Pts',(3.79594591694334,2.38047364248689,4.91104148452309));
#19483=CARTESIAN_POINT('Ctrl Pts',(3.6898649644607,2.22478479185514,4.89992769546629));
#19484=CARTESIAN_POINT('Ctrl Pts',(3.5015295908702,2.22947240830188,4.88881390640948));
#19485=CARTESIAN_POINT('Ctrl Pts',(3.40332529948609,2.39024586335038,4.87770011735268));
#19486=CARTESIAN_POINT('Ctrl Pts',(3.48513959192542,2.5599473902907,4.86658632829587));
#19487=CARTESIAN_POINT('Ctrl Pts',(3.67208691848091,2.58324725697266,4.85547253923907));
#19488=CARTESIAN_POINT('Ctrl Pts',(3.79305227102963,2.43881883118157,4.84435875018227));
#19489=CARTESIAN_POINT('Ctrl Pts',(3.73731469054324,2.25885908897487,4.83324496112546));
#19490=CARTESIAN_POINT('Ctrl Pts',(3.55589141654812,2.20808722327608,4.82213117206866));
#19491=CARTESIAN_POINT('Ctrl Pts',(3.41484122921187,2.33297529855171,4.81101738301186));
#19492=CARTESIAN_POINT('Ctrl Pts',(3.44326896462127,2.51921184317472,4.79990359395504));
#19493=CARTESIAN_POINT('Ctrl Pts',(3.61515439416365,2.59633243578568,4.78878980489825));
#19494=CARTESIAN_POINT('Ctrl Pts',(3.77316883486553,2.49374772336074,4.77767601584144));
#19495=CARTESIAN_POINT('Ctrl Pts',(3.77267987714682,2.30535465657222,4.76656222678464));
#19496=CARTESIAN_POINT('Ctrl Pts',(3.61413506955264,2.20359154597435,4.75544843772783));
#19497=CARTESIAN_POINT('Ctrl Pts',(3.44265227249432,2.28160332076952,4.74433464867103));
#19498=CARTESIAN_POINT('Ctrl Pts',(3.41519163486656,2.46798491877402,4.73322085961423));
#19499=CARTESIAN_POINT('Ctrl Pts',(3.55688818971484,2.59213914962324,4.72210707055742));
#19500=CARTESIAN_POINT('Ctrl Pts',(3.73804547343831,2.54042623781615,4.71099328150061));
#19501=CARTESIAN_POINT('Ctrl Pts',(3.79284816978155,2.36017959799409,4.69987949244381));
#19502=CARTESIAN_POINT('Ctrl Pts',(3.67113474927674,2.2163810237221,4.68876570338701));
#19503=CARTESIAN_POINT('Ctrl Pts',(3.48431088603601,2.24065098081811,4.67765191433021));
#19504=CARTESIAN_POINT('Ctrl Pts',(3.4033785808103,2.41077490231207,4.6665381252734));
#19505=CARTESIAN_POINT('Ctrl Pts',(3.50241609040748,2.57103643352413,4.65542433621659));
#19506=CARTESIAN_POINT('Ctrl Pts',(3.69077325913151,2.57474637744638,4.64431054715979));
#19507=CARTESIAN_POINT('Ctrl Pts',(3.79604463433366,2.41850898033344,4.63319675810299));
#19508=CARTESIAN_POINT('Ctrl Pts',(3.72187413243292,2.24533010361481,4.62208296904618));
#19509=CARTESIAN_POINT('Ctrl Pts',(3.5361508549695,2.21372233713422,4.61096917998938));
#19510=CARTESIAN_POINT('Ctrl Pts',(3.40886942405137,2.35261662800557,4.59985539093258));
#19511=CARTESIAN_POINT('Ctrl Pts',(3.45653197686655,2.53488145663037,4.58874160187577));
#19512=CARTESIAN_POINT('Ctrl Pts',(3.63551243829507,2.5936877583357,4.57762781281897));
#19513=CARTESIAN_POINT('Ctrl Pts',(3.78198796221116,2.47520945827968,4.56651402376216));
#19514=CARTESIAN_POINT('Ctrl Pts',(3.76188784043654,2.28789108810318,4.55540023470536));
#19515=CARTESIAN_POINT('Ctrl Pts',(3.5936099423673,2.20318727643507,4.54428644564855));
#19516=CARTESIAN_POINT('Ctrl Pts',(3.43118093653762,2.29862838255851,4.53317265659175));
#19517=CARTESIAN_POINT('Ctrl Pts',(3.42327393399308,2.4868560799498,4.52205886753494));
#19518=CARTESIAN_POINT('Ctrl Pts',(3.57712630395541,2.59558342196495,4.51094507847815));
#19519=CARTESIAN_POINT('Ctrl Pts',(3.75191522715083,2.52529104055601,4.49983128942133));
#19520=CARTESIAN_POINT('Ctrl Pts',(3.78765442042343,2.34031834729253,4.48871750036454));
#19521=CARTESIAN_POINT('Ctrl Pts',(3.65163139388737,2.20997295066536,4.47760371130772));
#19522=CARTESIAN_POINT('Ctrl Pts',(3.4683495682865,2.25356146118509,4.46648992225093));
#19523=CARTESIAN_POINT('Ctrl Pts',(3.40556887324678,2.431186839349,4.45537613319411));
#19524=CARTESIAN_POINT('Ctrl Pts',(3.52075319873735,2.58026652505992,4.44426234413732));
#19525=CARTESIAN_POINT('Ctrl Pts',(3.70847300970163,2.56434626551467,4.43314855508051));
#19526=CARTESIAN_POINT('Ctrl Pts',(3.79690626562936,2.39799790621595,4.4220347660237));
#19527=CARTESIAN_POINT('Ctrl Pts',(3.7051089416811,2.23348228455085,4.4109209769669));
#19528=CARTESIAN_POINT('Ctrl Pts',(3.51710429525804,2.22138181878176,4.3998071879101));
#19529=CARTESIAN_POINT('Ctrl Pts',(3.40497485954275,2.37277339597561,4.38869339885329));
#19530=CARTESIAN_POINT('Ctrl Pts',(3.47135448294965,2.54908419847293,4.37757960979649));
#19531=CARTESIAN_POINT('Ctrl Pts',(3.65548413352142,2.58893973580292,4.36646582073968));
#19532=CARTESIAN_POINT('Ctrl Pts',(3.78882987626983,2.45585019704184,4.35535203168288));
#19533=CARTESIAN_POINT('Ctrl Pts',(3.7493347906086,2.27165314263956,4.34423824262608));
#19534=CARTESIAN_POINT('Ctrl Pts',(3.57315728718835,2.20490778239848,4.33312445356927));
#19535=CARTESIAN_POINT('Ctrl Pts',(3.4215383866044,2.31678389237007,4.32201066451247));
#19536=CARTESIAN_POINT('Ctrl Pts',(3.43328916816391,2.50472575846861,4.31089687545566));
#19537=CARTESIAN_POINT('Ctrl Pts',(3.59758812791782,2.59701775419156,4.29978308639886));
#19538=CARTESIAN_POINT('Ctrl Pts',(3.76418967154123,2.50855366821667,4.28866929734205));
#19539=CARTESIAN_POINT('Ctrl Pts',(3.77483953817107,2.38400982617006,4.28126010463752));
#19540=CARTESIAN_POINT('Ctrl Pts',(3.75264423560529,2.33325198627316,4.27755550828525));
#19541=CARTESIAN_POINT('Ctrl Pts',(3.73677806246588,2.51633123698097,5.20748149723825));
#19542=CARTESIAN_POINT('Ctrl Pts',(3.77546096639785,2.47084927712496,5.20377690088598));
#19543=CARTESIAN_POINT('Ctrl Pts',(3.80318410060701,2.33901172932062,5.19636770818144));
#19544=CARTESIAN_POINT('Ctrl Pts',(3.658752630386,2.19593134317562,5.18525391912464));
#19545=CARTESIAN_POINT('Ctrl Pts',(3.46051057751011,2.24010387529317,5.17414013006783));
#19546=CARTESIAN_POINT('Ctrl Pts',(3.3899635101576,2.43040400586618,5.16302634101103));
#19547=CARTESIAN_POINT('Ctrl Pts',(3.5116556799136,2.59298794555462,5.15191255195423));
#19548=CARTESIAN_POINT('Ctrl Pts',(3.71421518662967,2.57887146826017,5.14079876289742));
#19549=CARTESIAN_POINT('Ctrl Pts',(3.81222985040785,2.40106004905331,5.12968497384063));
#19550=CARTESIAN_POINT('Ctrl Pts',(3.7159893174385,2.22226430270657,5.11857118478381));
#19551=CARTESIAN_POINT('Ctrl Pts',(3.5135818514907,2.20615907268523,5.10745739572702));
#19552=CARTESIAN_POINT('Ctrl Pts',(3.3902741941935,2.36747513785065,5.0963436066702));
#19553=CARTESIAN_POINT('Ctrl Pts',(3.45893079696141,2.55856332785872,5.08522981761341));
#19554=CARTESIAN_POINT('Ctrl Pts',(3.65670971522832,2.60451583195793,5.07411602855659));
#19555=CARTESIAN_POINT('Ctrl Pts',(3.80258155100106,2.46327311197376,5.0630022394998));
#19556=CARTESIAN_POINT('Ctrl Pts',(3.76302821419424,2.26411557718108,5.05188845044299));
#19557=CARTESIAN_POINT('Ctrl Pts',(3.57425329484041,2.18933470441319,5.04077466138619));
#19558=CARTESIAN_POINT('Ctrl Pts',(3.40904463131529,2.30737811148155,5.02966087232938));
#19559=CARTESIAN_POINT('Ctrl Pts',(3.41861958002714,2.51019941063974,5.01854708327258));
#19560=CARTESIAN_POINT('Ctrl Pts',(3.59421408528317,2.61215392594813,5.00743329421578));
#19561=CARTESIAN_POINT('Ctrl Pts',(3.77510450332242,2.51992155361066,4.99631950515897));
#19562=CARTESIAN_POINT('Ctrl Pts',(3.79571978393707,2.31792361987304,4.98520571610216));
#19563=CARTESIAN_POINT('Ctrl Pts',(3.63719052655772,2.19105112936158,4.97409192704537));
#19564=CARTESIAN_POINT('Ctrl Pts',(3.44462035852227,2.25543190894468,4.96297813798855));
#19565=CARTESIAN_POINT('Ctrl Pts',(3.3942709384207,2.4521375022049,4.95186434893175));
#19566=CARTESIAN_POINT('Ctrl Pts',(3.53222766152672,2.6011210482075,4.94075055987495));
#19567=CARTESIAN_POINT('Ctrl Pts',(3.73221717461903,2.56601621802281,4.92963677081814));
#19568=CARTESIAN_POINT('Ctrl Pts',(3.81118680834224,2.37895486067752,4.91852298176134));
#19569=CARTESIAN_POINT('Ctrl Pts',(3.69685476136628,2.21115635804835,4.90740919270453));
#19570=CARTESIAN_POINT('Ctrl Pts',(3.49387045290517,2.21620858251703,4.89629540364774));
#19571=CARTESIAN_POINT('Ctrl Pts',(3.38802772249033,2.38948717575083,4.88518161459092));
#19572=CARTESIAN_POINT('Ctrl Pts',(3.47620562160949,2.57238827624017,4.87406782553412));
#19573=CARTESIAN_POINT('Ctrl Pts',(3.67769391919309,2.59750043247249,4.86295403647732));
#19574=CARTESIAN_POINT('Ctrl Pts',(3.80806809143035,2.44183820305468,4.85184024742052));
#19575=CARTESIAN_POINT('Ctrl Pts',(3.74799517992873,2.24788099190383,4.84072645836371));
#19576=CARTESIAN_POINT('Ctrl Pts',(3.55246060185887,2.19316003401009,4.82961266930691));
#19577=CARTESIAN_POINT('Ctrl Pts',(3.40043937404102,2.32776204271177,4.8184988802501));
#19578=CARTESIAN_POINT('Ctrl Pts',(3.43107825033486,2.52848427295347,4.8073850911933));
#19579=CARTESIAN_POINT('Ctrl Pts',(3.61633311980013,2.61160339105013,4.79627130213649));
#19580=CARTESIAN_POINT('Ctrl Pts',(3.78663809948217,2.50103952557292,4.78515751307969));
#19581=CARTESIAN_POINT('Ctrl Pts',(3.78611111008816,2.29799303647267,4.77404372402288));
#19582=CARTESIAN_POINT('Ctrl Pts',(3.61523451098693,2.18831467792663,4.76292993496608));
#19583=CARTESIAN_POINT('Ctrl Pts',(3.43041359120824,2.27239429534918,4.75181614590927));
#19584=CARTESIAN_POINT('Ctrl Pts',(3.40081703463734,2.47327286138574,4.74070235685248));
#19585=CARTESIAN_POINT('Ctrl Pts',(3.55353490515134,2.60708394642517,4.72958856779567));
#19586=CARTESIAN_POINT('Ctrl Pts',(3.74878280393034,2.55134874680995,4.71847477873887));
#19587=CARTESIAN_POINT('Ctrl Pts',(3.80784811496013,2.35708232282806,4.70736098968206));
#19588=CARTESIAN_POINT('Ctrl Pts',(3.67666768920898,2.2020989354812,4.69624720062525));
#19589=CARTESIAN_POINT('Ctrl Pts',(3.47531245805411,2.22825663683913,4.68513341156846));
#19590=CARTESIAN_POINT('Ctrl Pts',(3.38808514809522,2.41161298620039,4.67401962251165));
#19591=CARTESIAN_POINT('Ctrl Pts',(3.49482590536264,2.58433983759226,4.66290583345484));
#19592=CARTESIAN_POINT('Ctrl Pts',(3.69783370420702,2.58833834507989,4.65179204439804));
#19593=CARTESIAN_POINT('Ctrl Pts',(3.811293204081,2.419948629414,4.64067825534124));
#19594=CARTESIAN_POINT('Ctrl Pts',(3.73135363803182,2.23329970701222,4.62956446628443));
#19595=CARTESIAN_POINT('Ctrl Pts',(3.53118459744037,2.19923345329287,4.61845067722763));
#19596=CARTESIAN_POINT('Ctrl Pts',(3.39400307523184,2.34893109662045,4.60733688817082));
#19597=CARTESIAN_POINT('Ctrl Pts',(3.44537287442694,2.54537268637529,4.59622309911402));
#19598=CARTESIAN_POINT('Ctrl Pts',(3.6382746352513,2.60875300764603,4.58510931005721));
#19599=CARTESIAN_POINT('Ctrl Pts',(3.79614318836354,2.48105933361106,4.57399552100041));
#19600=CARTESIAN_POINT('Ctrl Pts',(3.77447965675701,2.27917113222085,4.56288173194361));
#19601=CARTESIAN_POINT('Ctrl Pts',(3.59311291657604,2.18787896385287,4.5517679428868));
#19602=CARTESIAN_POINT('Ctrl Pts',(3.4180500019796,2.29074358538356,4.54065415383));
#19603=CARTESIAN_POINT('Ctrl Pts',(3.40952798398103,2.4936118424709,4.5295403647732));
#19604=CARTESIAN_POINT('Ctrl Pts',(3.57534716243134,2.61079611810118,4.51842657571639));
#19605=CARTESIAN_POINT('Ctrl Pts',(3.76373136251596,2.53503631706984,4.50731278665959));
#19606=CARTESIAN_POINT('Ctrl Pts',(3.80225038999918,2.33567624195239,4.49619899760278));
#19607=CARTESIAN_POINT('Ctrl Pts',(3.65564734114102,2.19519243537347,4.48508520854597));
#19608=CARTESIAN_POINT('Ctrl Pts',(3.45810965125396,2.24217130873125,4.47397141948918));
#19609=CARTESIAN_POINT('Ctrl Pts',(3.39044580391398,2.4336125864072,4.46285763043236));
#19610=CARTESIAN_POINT('Ctrl Pts',(3.51458929437743,2.59428785591567,4.45174384137557));
#19611=CARTESIAN_POINT('Ctrl Pts',(3.71691016106647,2.57712930087258,4.44063005231875));
#19612=CARTESIAN_POINT('Ctrl Pts',(3.8122218540174,2.39784218113421,4.42951626326196));
#19613=CARTESIAN_POINT('Ctrl Pts',(3.71328443209297,2.22053035140142,4.41840247420515));
#19614=CARTESIAN_POINT('Ctrl Pts',(3.5106565751263,2.2074886979437,4.40728868514835));
#19615=CARTESIAN_POINT('Ctrl Pts',(3.38980558716325,2.3706556804265,4.39617489609155));
#19616=CARTESIAN_POINT('Ctrl Pts',(3.46134829152241,2.56068013327812,4.38506110703473));
#19617=CARTESIAN_POINT('Ctrl Pts',(3.65979975114976,2.60363567863874,4.37394731797794));
#19618=CARTESIAN_POINT('Ctrl Pts',(3.80351727410895,2.46019428749802,4.36283352892113));
#19619=CARTESIAN_POINT('Ctrl Pts',(3.76095021674888,2.26167018129524,4.35171973986433));
#19620=CARTESIAN_POINT('Ctrl Pts',(3.57106943112482,2.18973329268408,4.34060595080752));
#19621=CARTESIAN_POINT('Ctrl Pts',(3.40765744378577,2.31031125094527,4.32949216175072));
#19622=CARTESIAN_POINT('Ctrl Pts',(3.42032221420706,2.51287144446394,4.31837837269392));
#19623=CARTESIAN_POINT('Ctrl Pts',(3.5974005298242,2.61234201428399,4.30726458363711));
#19624=CARTESIAN_POINT('Ctrl Pts',(3.77696052684568,2.51699709329055,4.29615079458031));
#19625=CARTESIAN_POINT('Ctrl Pts',(3.78843875194939,2.38276609266138,4.28874160187577));
#19626=CARTESIAN_POINT('Ctrl Pts',(3.76451707405898,2.328060251512,4.2850370055235));
#19627=CARTESIAN_POINT('Ctrl Pts',(3.74664903694653,2.52472660865709,5.2149629944765));
#19628=CARTESIAN_POINT('Ctrl Pts',(3.78812360169505,2.47596231494597,5.21125839812423));
#19629=CARTESIAN_POINT('Ctrl Pts',(3.81784745404107,2.33461033882977,5.20384920541969));
#19630=CARTESIAN_POINT('Ctrl Pts',(3.66299267959241,2.1812041532484,5.19273541636289));
#19631=CARTESIAN_POINT('Ctrl Pts',(3.4504439300895,2.22856452067679,5.18162162730609));
#19632=CARTESIAN_POINT('Ctrl Pts',(3.3748056347362,2.43259819666406,5.17050783824928));
#19633=CARTESIAN_POINT('Ctrl Pts',(3.5052800629955,2.60691546471448,5.15939404919248));
#19634=CARTESIAN_POINT('Ctrl Pts',(3.72245784756665,2.5917802320391,5.14828026013567));
#19635=CARTESIAN_POINT('Ctrl Pts',(3.82754601587795,2.40113655048171,5.13716647107887));
#19636=CARTESIAN_POINT('Ctrl Pts',(3.72436001352691,2.2094375050414,5.12605268202206));
#19637=CARTESIAN_POINT('Ctrl Pts',(3.5073452421747,2.19216999569193,5.11493889296526));
#19638=CARTESIAN_POINT('Ctrl Pts',(3.37513874016143,2.36512788948001,5.10382510390846));
#19639=CARTESIAN_POINT('Ctrl Pts',(3.44875014022381,2.57000649743315,5.09271131485165));
#19640=CARTESIAN_POINT('Ctrl Pts',(3.660802331703,2.61927529353934,5.08159752579485));
#19641=CARTESIAN_POINT('Ctrl Pts',(3.81720141974412,2.46783939447801,5.07048373673805));
#19642=CARTESIAN_POINT('Ctrl Pts',(3.77479360487843,2.25430909472489,5.05936994768124));
#19643=CARTESIAN_POINT('Ctrl Pts',(3.57239521127782,2.17413144945252,5.04825615862444));
#19644=CARTESIAN_POINT('Ctrl Pts',(3.39526379879546,2.30069379177829,5.03714236956763));
#19645=CARTESIAN_POINT('Ctrl Pts',(3.40552975067466,2.51815226178119,5.02602858051083));
#19646=CARTESIAN_POINT('Ctrl Pts',(3.59379652843607,2.62746461211554,5.01491479145402));
#19647=CARTESIAN_POINT('Ctrl Pts',(3.78774141345684,2.52857603060814,5.00380100239722));
#19648=CARTESIAN_POINT('Ctrl Pts',(3.80984445391536,2.3120003465126,4.99268721334041));
#19649=CARTESIAN_POINT('Ctrl Pts',(3.63987448575377,2.17597174504624,4.98157342428361));
#19650=CARTESIAN_POINT('Ctrl Pts',(3.43340694865093,2.24499874508934,4.9704596352268));
#19651=CARTESIAN_POINT('Ctrl Pts',(3.37942392070334,2.45590015203683,4.95934584617001));
#19652=CARTESIAN_POINT('Ctrl Pts',(3.52733667965797,2.61563551564903,4.94823205711319));
#19653=CARTESIAN_POINT('Ctrl Pts',(3.74175899977021,2.57799724642702,4.9371182680564));
#19654=CARTESIAN_POINT('Ctrl Pts',(3.82642769974115,2.37743607886815,4.92600447899959));
#19655=CARTESIAN_POINT('Ctrl Pts',(3.70384455827186,2.19752792424157,4.91489068994279));
#19656=CARTESIAN_POINT('Ctrl Pts',(3.48621131494014,2.20294475673219,4.90377690088598));
#19657=CARTESIAN_POINT('Ctrl Pts',(3.37273014549458,2.38872848815129,4.89266311182918));
#19658=CARTESIAN_POINT('Ctrl Pts',(3.46727165129357,2.58482916218966,4.88154932277237));
#19659=CARTESIAN_POINT('Ctrl Pts',(3.68330091990526,2.61175360797231,4.87043553371557));
#19660=CARTESIAN_POINT('Ctrl Pts',(3.82308391183106,2.4448575749278,4.85932174465876));
#19661=CARTESIAN_POINT('Ctrl Pts',(3.75867566931422,2.2369028948328,4.84820795560196));
#19662=CARTESIAN_POINT('Ctrl Pts',(3.54902978716961,2.1782328447441,4.83709416654516));
#19663=CARTESIAN_POINT('Ctrl Pts',(3.38603751887018,2.32254878687183,4.82598037748835));
#19664=CARTESIAN_POINT('Ctrl Pts',(3.41888753604845,2.53775670273222,4.81486658843155));
#19665=CARTESIAN_POINT('Ctrl Pts',(3.61751184543661,2.62687434631457,4.80375279937474));
#19666=CARTESIAN_POINT('Ctrl Pts',(3.80010736409881,2.5083313277851,4.79263901031794));
#19667=CARTESIAN_POINT('Ctrl Pts',(3.79954234302951,2.29063141637312,4.78152522126113));
#19668=CARTESIAN_POINT('Ctrl Pts',(3.61633395242122,2.17303780987892,4.77041143220434));
#19669=CARTESIAN_POINT('Ctrl Pts',(3.41817490992216,2.26318526992884,4.75929764314752));
#19670=CARTESIAN_POINT('Ctrl Pts',(3.38644243440813,2.47856080399747,4.74818385409073));
#19671=CARTESIAN_POINT('Ctrl Pts',(3.55018162058784,2.62202874322709,4.73707006503392));
#19672=CARTESIAN_POINT('Ctrl Pts',(3.75952013442236,2.56227125580376,4.72595627597711));
#19673=CARTESIAN_POINT('Ctrl Pts',(3.82284806013872,2.35398504766203,4.71484248692031));
#19674=CARTESIAN_POINT('Ctrl Pts',(3.68220062914122,2.1878168472403,4.7037286978635));
#19675=CARTESIAN_POINT('Ctrl Pts',(3.46631403007222,2.21586229286015,4.6926149088067));
#19676=CARTESIAN_POINT('Ctrl Pts',(3.37279171538014,2.4124510700887,4.6815011197499));
#19677=CARTESIAN_POINT('Ctrl Pts',(3.48723572031781,2.59764324166039,4.67038733069309));
#19678=CARTESIAN_POINT('Ctrl Pts',(3.70489414928252,2.6019303127134,4.65927354163629));
#19679=CARTESIAN_POINT('Ctrl Pts',(3.82654177382834,2.42138827849455,4.64815975257948));
#19680=CARTESIAN_POINT('Ctrl Pts',(3.74083314363071,2.22126931040964,4.63704596352268));
#19681=CARTESIAN_POINT('Ctrl Pts',(3.52621833991124,2.18474456945152,4.62593217446588));
#19682=CARTESIAN_POINT('Ctrl Pts',(3.3791367264123,2.34524556523533,4.61481838540907));
#19683=CARTESIAN_POINT('Ctrl Pts',(3.43421377198734,2.55586391612019,4.60370459635226));
#19684=CARTESIAN_POINT('Ctrl Pts',(3.64103683220752,2.62381825695636,4.59259080729547));
#19685=CARTESIAN_POINT('Ctrl Pts',(3.81029841451592,2.48690920894243,4.58147701823866));
#19686=CARTESIAN_POINT('Ctrl Pts',(3.78707147307748,2.27045117633852,4.57036322918186));
#19687=CARTESIAN_POINT('Ctrl Pts',(3.59261589078479,2.17257065127066,4.55924944012505));
#19688=CARTESIAN_POINT('Ctrl Pts',(3.40491906742157,2.28285878820862,4.54813565106825));
#19689=CARTESIAN_POINT('Ctrl Pts',(3.39578203396899,2.500367604992,4.53702186201145));
#19690=CARTESIAN_POINT('Ctrl Pts',(3.57356802090726,2.62600881423741,4.52590807295463));
#19691=CARTESIAN_POINT('Ctrl Pts',(3.77554749788108,2.54478159358368,4.51479428389784));
#19692=CARTESIAN_POINT('Ctrl Pts',(3.81684635957493,2.33103413661225,4.50368049484102));
#19693=CARTESIAN_POINT('Ctrl Pts',(3.65966328839466,2.18041192008159,4.49256670578423));
#19694=CARTESIAN_POINT('Ctrl Pts',(3.44786973422143,2.23078115627741,4.48145291672742));
#19695=CARTESIAN_POINT('Ctrl Pts',(3.37532273458119,2.43603833346541,4.47033912767062));
#19696=CARTESIAN_POINT('Ctrl Pts',(3.50842539001751,2.60830918677142,4.45922533861381));
#19697=CARTESIAN_POINT('Ctrl Pts',(3.72534731243133,2.58991233623048,4.44811154955701));
#19698=CARTESIAN_POINT('Ctrl Pts',(3.82753744240543,2.39768645605247,4.4369977605002));
#19699=CARTESIAN_POINT('Ctrl Pts',(3.72145992250484,2.20757841825199,4.4258839714434));
#19700=CARTESIAN_POINT('Ctrl Pts',(3.50420885499455,2.19359557710565,4.41477018238659));
#19701=CARTESIAN_POINT('Ctrl Pts',(3.37463631478375,2.36853796487738,4.40365639332979));
#19702=CARTESIAN_POINT('Ctrl Pts',(3.45134210009517,2.57227606808331,4.39254260427299));
#19703=CARTESIAN_POINT('Ctrl Pts',(3.6641153687781,2.61833162147455,4.38142881521619));
#19704=CARTESIAN_POINT('Ctrl Pts',(3.81820467194806,2.46453837795421,4.37031502615938));
#19705=CARTESIAN_POINT('Ctrl Pts',(3.77256564288916,2.25168721995093,4.35920123710258));
#19706=CARTESIAN_POINT('Ctrl Pts',(3.56898157506129,2.17455880296967,4.34808744804577));
#19707=CARTESIAN_POINT('Ctrl Pts',(3.39377650096713,2.30383860952047,4.33697365898897));
#19708=CARTESIAN_POINT('Ctrl Pts',(3.40735526025023,2.52101713045927,4.32585986993216));
#19709=CARTESIAN_POINT('Ctrl Pts',(3.59721293173057,2.62766627437643,4.31474608087536));
#19710=CARTESIAN_POINT('Ctrl Pts',(3.78973138215013,2.52544051836443,4.30363229181856));
#19711=CARTESIAN_POINT('Ctrl Pts',(3.8020379657277,2.3815223591527,4.29622309911402));
#19712=CARTESIAN_POINT('Ctrl Pts',(3.77638991251267,2.32286851675083,4.29251850276175));
#19713=CARTESIAN_POINT('Ctrl Pts',(3.75652001142717,2.53312198033322,5.22244449171475));
#19714=CARTESIAN_POINT('Ctrl Pts',(3.80078623699225,2.48107535276698,5.21873989536248));
#19715=CARTESIAN_POINT('Ctrl Pts',(3.83251080747514,2.33020894833891,5.21133070265794));
#19716=CARTESIAN_POINT('Ctrl Pts',(3.6672327287988,2.16647696332117,5.20021691360114));
#19717=CARTESIAN_POINT('Ctrl Pts',(3.44037728266889,2.21702516606042,5.18910312454433));
#19718=CARTESIAN_POINT('Ctrl Pts',(3.3596477593148,2.43479238746194,5.17798933548753));
#19719=CARTESIAN_POINT('Ctrl Pts',(3.4989044460774,2.62084298387434,5.16687554643073));
#19720=CARTESIAN_POINT('Ctrl Pts',(3.73070050850364,2.60468899581803,5.15576175737391));
#19721=CARTESIAN_POINT('Ctrl Pts',(3.84286218134804,2.40121305191012,5.14464796831713));
#19722=CARTESIAN_POINT('Ctrl Pts',(3.73273070961532,2.19661070737624,5.1335341792603));
#19723=CARTESIAN_POINT('Ctrl Pts',(3.50110863285869,2.17818091869864,5.12242039020352));
#19724=CARTESIAN_POINT('Ctrl Pts',(3.36000328612935,2.36278064110937,5.1113066011467));
#19725=CARTESIAN_POINT('Ctrl Pts',(3.43856948348621,2.58144966700758,5.10019281208991));
#19726=CARTESIAN_POINT('Ctrl Pts',(3.66489494817768,2.63403475512075,5.08907902303309));
#19727=CARTESIAN_POINT('Ctrl Pts',(3.83182128848718,2.47240567698227,5.0779652339763));
#19728=CARTESIAN_POINT('Ctrl Pts',(3.78655899556261,2.24450261226871,5.06685144491949));
#19729=CARTESIAN_POINT('Ctrl Pts',(3.57053712771522,2.15892819449186,5.05573765586269));
#19730=CARTESIAN_POINT('Ctrl Pts',(3.38148296627563,2.29400947207503,5.04462386680588));
#19731=CARTESIAN_POINT('Ctrl Pts',(3.39243992132218,2.52610511292264,5.03351007774908));
#19732=CARTESIAN_POINT('Ctrl Pts',(3.59337897158896,2.64277529828296,5.02239628869227));
#19733=CARTESIAN_POINT('Ctrl Pts',(3.80037832359127,2.53723050760561,5.01128249963547));
#19734=CARTESIAN_POINT('Ctrl Pts',(3.82396912389365,2.30607707315216,5.00016871057866));
#19735=CARTESIAN_POINT('Ctrl Pts',(3.64255844494981,2.16089236073089,4.98905492152186));
#19736=CARTESIAN_POINT('Ctrl Pts',(3.42219353877959,2.234565581234,4.97794113246505));
#19737=CARTESIAN_POINT('Ctrl Pts',(3.36457690298599,2.45966280186876,4.96682734340826));
#19738=CARTESIAN_POINT('Ctrl Pts',(3.52244569778922,2.63014998309056,4.95571355435144));
#19739=CARTESIAN_POINT('Ctrl Pts',(3.7513008249214,2.58997827483123,4.94459976529465));
#19740=CARTESIAN_POINT('Ctrl Pts',(3.84166859114005,2.37591729705878,4.93348597623783));
#19741=CARTESIAN_POINT('Ctrl Pts',(3.71083435517744,2.18389949043478,4.92237218718104));
#19742=CARTESIAN_POINT('Ctrl Pts',(3.47855217697512,2.18968093094735,4.91125839812423));
#19743=CARTESIAN_POINT('Ctrl Pts',(3.35743256849882,2.38796980055174,4.90014460906743));
#19744=CARTESIAN_POINT('Ctrl Pts',(3.45833768097764,2.59727004813914,4.88903082001062));
#19745=CARTESIAN_POINT('Ctrl Pts',(3.68890792061744,2.62600678347214,4.87791703095382));
#19746=CARTESIAN_POINT('Ctrl Pts',(3.83809973223177,2.44787694680091,4.86680324189701));
#19747=CARTESIAN_POINT('Ctrl Pts',(3.76935615869971,2.22592479776177,4.85568945284022));
#19748=CARTESIAN_POINT('Ctrl Pts',(3.54559897248035,2.16330565547811,4.8445756637834));
#19749=CARTESIAN_POINT('Ctrl Pts',(3.37163566369933,2.31733553103189,4.83346187472661));
#19750=CARTESIAN_POINT('Ctrl Pts',(3.40669682176204,2.54702913251096,4.82234808566979));
#19751=CARTESIAN_POINT('Ctrl Pts',(3.61869057107309,2.64214530157901,4.811234296613));
#19752=CARTESIAN_POINT('Ctrl Pts',(3.81357662871545,2.51562312999728,4.80012050755618));
#19753=CARTESIAN_POINT('Ctrl Pts',(3.81297357597085,2.28326979627357,4.78900671849939));
#19754=CARTESIAN_POINT('Ctrl Pts',(3.61743339385551,2.1577609418312,4.77789292944258));
#19755=CARTESIAN_POINT('Ctrl Pts',(3.40593622863608,2.2539762445085,4.76677914038578));
#19756=CARTESIAN_POINT('Ctrl Pts',(3.37206783417891,2.48384874660919,4.75566535132897));
#19757=CARTESIAN_POINT('Ctrl Pts',(3.54682833602434,2.63697354002902,4.74455156227216));
#19758=CARTESIAN_POINT('Ctrl Pts',(3.77025746491439,2.57319376479756,4.73343777321537));
#19759=CARTESIAN_POINT('Ctrl Pts',(3.83784800531731,2.35088777249601,4.72232398415856));
#19760=CARTESIAN_POINT('Ctrl Pts',(3.68773356907346,2.1735347589994,4.71121019510175));
#19761=CARTESIAN_POINT('Ctrl Pts',(3.45731560209032,2.20346794888116,4.70009640604495));
#19762=CARTESIAN_POINT('Ctrl Pts',(3.35749828266505,2.41328915397702,4.68898261698814));
#19763=CARTESIAN_POINT('Ctrl Pts',(3.47964553527297,2.61094664572852,4.67786882793135));
#19764=CARTESIAN_POINT('Ctrl Pts',(3.71195459435803,2.61552228034691,4.66675503887453));
#19765=CARTESIAN_POINT('Ctrl Pts',(3.84179034357568,2.42282792757511,4.65564124981774));
#19766=CARTESIAN_POINT('Ctrl Pts',(3.75031264922961,2.20923891380705,4.64452746076093));
#19767=CARTESIAN_POINT('Ctrl Pts',(3.5212520823821,2.17025568561017,4.63341367170412));
#19768=CARTESIAN_POINT('Ctrl Pts',(3.36427037759277,2.34156003385021,4.62229988264733));
#19769=CARTESIAN_POINT('Ctrl Pts',(3.42305466954774,2.56635514586511,4.61118609359051));
#19770=CARTESIAN_POINT('Ctrl Pts',(3.64379902916374,2.63888350626668,4.60007230453372));
#19771=CARTESIAN_POINT('Ctrl Pts',(3.8244536406683,2.49275908427381,4.5889585154769));
#19772=CARTESIAN_POINT('Ctrl Pts',(3.79966328939795,2.26173122045618,4.57784472642011));
#19773=CARTESIAN_POINT('Ctrl Pts',(3.59211886499353,2.15726233868846,4.56673093736329));
#19774=CARTESIAN_POINT('Ctrl Pts',(3.39178813286355,2.27497399103367,4.55561714830651));
#19775=CARTESIAN_POINT('Ctrl Pts',(3.38203608395695,2.50712336751311,4.54450335924968));
#19776=CARTESIAN_POINT('Ctrl Pts',(3.57178887938318,2.64122151037363,4.5333895701929));
#19777=CARTESIAN_POINT('Ctrl Pts',(3.78736363324621,2.55452687009752,4.52227578113608));
#19778=CARTESIAN_POINT('Ctrl Pts',(3.83144232915068,2.3263920312721,4.51116199207928));
#19779=CARTESIAN_POINT('Ctrl Pts',(3.66367923564831,2.1656314047897,4.50004820302247));
#19780=CARTESIAN_POINT('Ctrl Pts',(3.43762981718889,2.21939100382357,4.48893441396567));
#19781=CARTESIAN_POINT('Ctrl Pts',(3.36019966524839,2.43846408052362,4.47782062490886));
#19782=CARTESIAN_POINT('Ctrl Pts',(3.5022614856576,2.62233051762717,4.46670683585207));
#19783=CARTESIAN_POINT('Ctrl Pts',(3.73378446379617,2.60269537158839,4.45559304679526));
#19784=CARTESIAN_POINT('Ctrl Pts',(3.84285303079348,2.39753073097072,4.44447925773845));
#19785=CARTESIAN_POINT('Ctrl Pts',(3.72963541291671,2.19462648510256,4.43336546868165));
#19786=CARTESIAN_POINT('Ctrl Pts',(3.49776113486282,2.17970245626759,4.42225167962485));
#19787=CARTESIAN_POINT('Ctrl Pts',(3.35946704240424,2.36642024932827,4.41113789056804));
#19788=CARTESIAN_POINT('Ctrl Pts',(3.44133590866794,2.5838720028885,4.40002410151124));
#19789=CARTESIAN_POINT('Ctrl Pts',(3.66843098640644,2.63302756431036,4.38891031245443));
#19790=CARTESIAN_POINT('Ctrl Pts',(3.83289206978718,2.4688824684104,4.37779652339763));
#19791=CARTESIAN_POINT('Ctrl Pts',(3.78418106902943,2.24170425860662,4.36668273434082));
#19792=CARTESIAN_POINT('Ctrl Pts',(3.56689371899776,2.15938431325527,4.35556894528402));
#19793=CARTESIAN_POINT('Ctrl Pts',(3.37989555814849,2.29736596809567,4.34445515622721));
#19794=CARTESIAN_POINT('Ctrl Pts',(3.39438830629339,2.5291628164546,4.33334136717041));
#19795=CARTESIAN_POINT('Ctrl Pts',(3.59702533363695,2.64299053446886,4.32222757811361));
#19796=CARTESIAN_POINT('Ctrl Pts',(3.80250223745458,2.5338839434383,4.3111137890568));
#19797=CARTESIAN_POINT('Ctrl Pts',(3.81563717950601,2.38027862564402,4.30370459635227));
#19798=CARTESIAN_POINT('Ctrl Pts',(3.78826275096636,2.31767678198967,4.3));
#19799=CARTESIAN_POINT('Ctrl Pts',(3.72690708798524,2.50793586530485,5.2));
#19800=CARTESIAN_POINT('Ctrl Pts',(3.7351188943469,2.50027512151453,5.2));
#19801=CARTESIAN_POINT('Ctrl Pts',(3.74243605781657,2.49177396851828,5.2));
#19802=CARTESIAN_POINT('Ctrl Pts',(3.74885415042291,2.48262661237479,5.2));
#19803=CARTESIAN_POINT('Ctrl Pts',(3.75362491760652,2.47582709900174,5.2));
#19804=CARTESIAN_POINT('Ctrl Pts',(3.75789857135109,2.46866923842676,5.2));
#19805=CARTESIAN_POINT('Ctrl Pts',(3.7616631109362,2.46121836915243,5.2));
#19806=CARTESIAN_POINT('Ctrl Pts',(3.76388040997986,2.45682983638691,5.2));
#19807=CARTESIAN_POINT('Ctrl Pts',(3.76592247954252,2.45233444011456,5.2));
#19808=CARTESIAN_POINT('Ctrl Pts',(3.76777440855395,2.44777396604178,5.2));
#19809=CARTESIAN_POINT('Ctrl Pts',(3.77233273486399,2.43654884411541,5.2));
#19810=CARTESIAN_POINT('Ctrl Pts',(3.77575805024602,2.42490557824884,5.2));
#19811=CARTESIAN_POINT('Ctrl Pts',(3.77802226640697,2.41304266545579,5.2));
#19812=CARTESIAN_POINT('Ctrl Pts',(3.7794611438358,2.4055039517268,5.2));
#19813=CARTESIAN_POINT('Ctrl Pts',(3.78043038990374,2.39787565429666,5.2));
#19814=CARTESIAN_POINT('Ctrl Pts',(3.78091323142362,2.39020359559663,5.2));
#19815=CARTESIAN_POINT('Ctrl Pts',(3.78113855699256,2.38662330906275,5.2));
#19816=CARTESIAN_POINT('Ctrl Pts',(3.78125741264451,2.38303694149785,5.2));
#19817=CARTESIAN_POINT('Ctrl Pts',(3.78126865224829,2.37945929304311,5.2));
#19818=CARTESIAN_POINT('Ctrl Pts',(3.7813036985799,2.36830378822358,5.2));
#19819=CARTESIAN_POINT('Ctrl Pts',(3.78029680360483,2.3572059009501,5.2));
#19820=CARTESIAN_POINT('Ctrl Pts',(3.77821424861763,2.34630678216484,5.2));
#19821=CARTESIAN_POINT('Ctrl Pts',(3.77705386628862,2.34023388376937,5.2));
#19822=CARTESIAN_POINT('Ctrl Pts',(3.77555898983988,2.33422245704814,5.2));
#19823=CARTESIAN_POINT('Ctrl Pts',(3.77374834890996,2.32828864283844,5.2));
#19824=CARTESIAN_POINT('Ctrl Pts',(3.7726157055599,2.32457675546527,5.2));
#19825=CARTESIAN_POINT('Ctrl Pts',(3.77135884755536,2.32089372066286,5.2));
#19826=CARTESIAN_POINT('Ctrl Pts',(3.76998347568685,2.31724835341447,5.2));
#19827=CARTESIAN_POINT('Ctrl Pts',(3.76560168937412,2.30563460684914,5.2));
#19828=CARTESIAN_POINT('Ctrl Pts',(3.76005258957863,2.29448378034876,5.2));
#19829=CARTESIAN_POINT('Ctrl Pts',(3.75350159415067,2.28391841534468,5.2));
#19830=CARTESIAN_POINT('Ctrl Pts',(3.74916061754095,2.27691734155978,5.2));
#19831=CARTESIAN_POINT('Ctrl Pts',(3.74437851970176,2.27017319623005,5.2));
#19832=CARTESIAN_POINT('Ctrl Pts',(3.73919188354146,2.26372385230471,5.2));
#19833=CARTESIAN_POINT('Ctrl Pts',(3.73648175856153,2.26035393632525,5.2));
#19834=CARTESIAN_POINT('Ctrl Pts',(3.73365978483958,2.25706319070089,5.2));
#19835=CARTESIAN_POINT('Ctrl Pts',(3.73073434111394,2.25386182215374,5.2));
#19836=CARTESIAN_POINT('Ctrl Pts',(3.72446791350779,2.24700435158764,5.2));
#19837=CARTESIAN_POINT('Ctrl Pts',(3.71775194552741,2.24058263588329,5.2));
#19838=CARTESIAN_POINT('Ctrl Pts',(3.71064052052299,2.23464742809312,5.2));
#19839=CARTESIAN_POINT('Ctrl Pts',(3.70611387191905,2.23086947922341,5.2));
#19840=CARTESIAN_POINT('Ctrl Pts',(3.70142674452504,2.22728872352275,5.2));
#19841=CARTESIAN_POINT('Ctrl Pts',(3.69659089091882,2.22391966825811,5.2));
#19842=CARTESIAN_POINT('Ctrl Pts',(3.69251851777989,2.22108251658222,5.2));
#19843=CARTESIAN_POINT('Ctrl Pts',(3.68834767342073,2.21840053637087,5.2));
#19844=CARTESIAN_POINT('Ctrl Pts',(3.68408917108174,2.21588334611703,5.2));
#19845=CARTESIAN_POINT('Ctrl Pts',(3.67536611602187,2.21072716973562,5.2));
#19846=CARTESIAN_POINT('Ctrl Pts',(3.66627202526677,2.20625880103906,5.2));
#19847=CARTESIAN_POINT('Ctrl Pts',(3.65686566645047,2.20255201748434,5.2));
#19848=CARTESIAN_POINT('Ctrl Pts',(3.65562635833217,2.2020636407339,5.2));
#19849=CARTESIAN_POINT('Ctrl Pts',(3.65438161447105,2.20158850411268,5.2));
#19850=CARTESIAN_POINT('Ctrl Pts',(3.65313162618094,2.20112654952031,5.2));
#19851=CARTESIAN_POINT('Ctrl Pts',(3.43326717741735,2.39986996798437,5.08714803633902));
#19852=CARTESIAN_POINT('Ctrl Pts',(3.43319402496042,2.39134538728232,5.08771939403666));
#19853=CARTESIAN_POINT('Ctrl Pts',(3.43379133263065,2.38283109195966,5.08829075173431));
#19854=CARTESIAN_POINT('Ctrl Pts',(3.43509475123467,2.374426308808,5.08886210943196));
#19855=CARTESIAN_POINT('Ctrl Pts',(3.44354591908595,2.31993097404037,5.09256670578422));
#19856=CARTESIAN_POINT('Ctrl Pts',(3.48168218994633,2.27003956185944,5.0962713021365));
#19857=CARTESIAN_POINT('Ctrl Pts',(3.53205035213375,2.24758434755118,5.09997589848876));
#19858=CARTESIAN_POINT('Ctrl Pts',(3.58241851432117,2.22512913324292,5.10368049484103));
#19859=CARTESIAN_POINT('Ctrl Pts',(3.64501856783563,2.23011011680733,5.1073850911933));
#19860=CARTESIAN_POINT('Ctrl Pts',(3.69120110519081,2.26024934979839,5.11108968754557));
#19861=CARTESIAN_POINT('Ctrl Pts',(3.73738364254598,2.29038858278945,5.11479428389783));
#19862=CARTESIAN_POINT('Ctrl Pts',(3.76714866374187,2.34568606520718,5.1184988802501));
#19863=CARTESIAN_POINT('Ctrl Pts',(3.76687431446563,2.40083133255876,5.12220347660237));
#19864=CARTESIAN_POINT('Ctrl Pts',(3.7665999651894,2.45597659991035,5.12590807295464));
#19865=CARTESIAN_POINT('Ctrl Pts',(3.73628624544104,2.51096965219579,5.12961266930691));
#19866=CARTESIAN_POINT('Ctrl Pts',(3.68980584742337,2.54064913199077,5.13331726565917));
#19867=CARTESIAN_POINT('Ctrl Pts',(3.6433254494057,2.57032861178575,5.13702186201144));
#19868=CARTESIAN_POINT('Ctrl Pts',(3.5806783731187,2.57469451909026,5.14072645836371));
#19869=CARTESIAN_POINT('Ctrl Pts',(3.53053651643308,2.5517357041881,5.14443105471598));
#19870=CARTESIAN_POINT('Ctrl Pts',(3.48039465974747,2.52877688928595,5.14813565106825));
#19871=CARTESIAN_POINT('Ctrl Pts',(3.44275802266323,2.47849335217712,5.15184024742051));
#19872=CARTESIAN_POINT('Ctrl Pts',(3.43484901067973,2.42392381942959,5.15554484377278));
#19873=CARTESIAN_POINT('Ctrl Pts',(3.43370811542309,2.41605202441919,5.15607924129486));
#19874=CARTESIAN_POINT('Ctrl Pts',(3.43318581643692,2.40809104297335,5.15661363881694));
#19875=CARTESIAN_POINT('Ctrl Pts',(3.43325215340634,2.40012157034435,5.15714803633902));
#19876=CARTESIAN_POINT('Ctrl Pts',(3.54698297828114,2.20148256743283,5.2));
#19877=CARTESIAN_POINT('Ctrl Pts',(3.48097120902544,2.21911198848201,5.19629540364773));
#19878=CARTESIAN_POINT('Ctrl Pts',(3.36906718698604,2.32515231990061,5.1888862109432));
#19879=CARTESIAN_POINT('Ctrl Pts',(3.41187706889408,2.55382793971174,5.17777242188639));
#19880=CARTESIAN_POINT('Ctrl Pts',(3.62721323264599,2.64128528195604,5.16665863282959));
#19881=CARTESIAN_POINT('Ctrl Pts',(3.81747536314189,2.50809334538988,5.15554484377278));
#19882=CARTESIAN_POINT('Ctrl Pts',(3.80876232811303,2.27586209318291,5.14443105471598));
#19883=CARTESIAN_POINT('Ctrl Pts',(3.60892557137656,2.15730570431671,5.13331726565918));
#19884=CARTESIAN_POINT('Ctrl Pts',(3.40093971248811,2.26086517215761,5.12220347660237));
#19885=CARTESIAN_POINT('Ctrl Pts',(3.37514571617861,2.4917888042929,5.11108968754557));
#19886=CARTESIAN_POINT('Ctrl Pts',(3.55516852834243,2.63869087044012,5.09997589848876));
#19887=CARTESIAN_POINT('Ctrl Pts',(3.77622353148193,2.56711958879047,5.08886210943196));
#19888=CARTESIAN_POINT('Ctrl Pts',(3.8359804180852,2.34258029751366,5.07774832037515));
#19889=CARTESIAN_POINT('Ctrl Pts',(3.6797411123384,2.17059868763558,5.06663453131835));
#19890=CARTESIAN_POINT('Ctrl Pts',(3.45051418153466,2.2085903127083,5.05552074226155));
#19891=CARTESIAN_POINT('Ctrl Pts',(3.3581131561336,2.4217815890047,5.04440695320474));
#19892=CARTESIAN_POINT('Ctrl Pts',(3.48711398178203,2.61503583311392,5.03329316414794));
#19893=CARTESIAN_POINT('Ctrl Pts',(3.71944062032543,2.61146538882495,5.02217937509113));
#19894=CARTESIAN_POINT('Ctrl Pts',(3.84244192441188,2.41433825182845,5.01106558603433));
#19895=CARTESIAN_POINT('Ctrl Pts',(3.74353337567863,2.20408716238119,4.99995179697753));
#19896=CARTESIAN_POINT('Ctrl Pts',(3.51324710536571,2.17315730898832,4.98883800792072));
#19897=CARTESIAN_POINT('Ctrl Pts',(3.36236674087989,2.34985914625667,4.97772421886392));
#19898=CARTESIAN_POINT('Ctrl Pts',(3.42899479464802,2.5724554740903,4.96661042980711));
#19899=CARTESIAN_POINT('Ctrl Pts',(3.652145851588,2.63720135146115,4.95549664075031));
#19900=CARTESIAN_POINT('Ctrl Pts',(3.82756721950384,2.48483414141864,4.9443828516935));
#19901=CARTESIAN_POINT('Ctrl Pts',(3.79469373046592,2.25481727983819,4.9332690626367));
#19902=CARTESIAN_POINT('Ctrl Pts',(3.58361486203243,2.15768780841241,4.9221552735799));
#19903=CARTESIAN_POINT('Ctrl Pts',(3.38753349616232,2.28234943400059,4.91104148452309));
#19904=CARTESIAN_POINT('Ctrl Pts',(3.38592513080807,2.51469795687288,4.89992769546629));
#19905=CARTESIAN_POINT('Ctrl Pts',(3.58026192098975,2.64206213906777,4.88881390640948));
#19906=CARTESIAN_POINT('Ctrl Pts',(3.79266519873933,2.54786410019675,4.87770011735268));
#19907=CARTESIAN_POINT('Ctrl Pts',(3.82871983510845,2.3183243735256,4.86658632829587));
#19908=CARTESIAN_POINT('Ctrl Pts',(3.65542461254465,2.16354327402962,4.85547253923907));
#19909=CARTESIAN_POINT('Ctrl Pts',(3.43139861356028,2.22519369741672,4.84435875018226));
#19910=CARTESIAN_POINT('Ctrl Pts',(3.36169537565425,2.44684631199623,4.83324496112547));
#19911=CARTESIAN_POINT('Ctrl Pts',(3.51011506296999,2.62561996593247,4.82213117206865));
#19912=CARTESIAN_POINT('Ctrl Pts',(3.74080745251389,2.59788110634618,4.81101738301186));
#19913=CARTESIAN_POINT('Ctrl Pts',(3.84261718390667,2.38901942599691,4.79990359395504));
#19914=CARTESIAN_POINT('Ctrl Pts',(3.72235665540369,2.19020838956081,4.78878980489825));
#19915=CARTESIAN_POINT('Ctrl Pts',(3.49010169259086,2.18342199335841,4.77767601584144));
#19916=CARTESIAN_POINT('Ctrl Pts',(3.35843789688119,2.37487190279669,4.76656222678464));
#19917=CARTESIAN_POINT('Ctrl Pts',(3.44787863365674,2.58932184457717,4.75544843772783));
#19918=CARTESIAN_POINT('Ctrl Pts',(3.67655778221991,2.63048335496042,4.74433464867103));
#19919=CARTESIAN_POINT('Ctrl Pts',(3.8351627244929,2.46068083668937,4.73322085961423));
#19920=CARTESIAN_POINT('Ctrl Pts',(3.77852055811084,2.23533646042905,4.72210707055742));
#19921=CARTESIAN_POINT('Ctrl Pts',(3.55847650032912,2.16071048934957,4.71099328150062));
#19922=CARTESIAN_POINT('Ctrl Pts',(3.37643937270466,2.30510892109605,4.69987949244382));
#19923=CARTESIAN_POINT('Ctrl Pts',(3.39902982259358,2.53636223350135,4.68876570338701));
#19924=CARTESIAN_POINT('Ctrl Pts',(3.60557055501943,2.64280164712995,4.67765191433021));
#19925=CARTESIAN_POINT('Ctrl Pts',(3.80701249526159,2.52700195958257,4.6665381252734));
#19926=CARTESIAN_POINT('Ctrl Pts',(3.81897355090948,2.29495593812904,4.65542433621659));
#19927=CARTESIAN_POINT('Ctrl Pts',(3.63050563208088,2.15905793778677,4.6443105471598));
#19928=CARTESIAN_POINT('Ctrl Pts',(3.41411556225142,2.24369693945694,4.63319675810298));
#19929=CARTESIAN_POINT('Ctrl Pts',(3.3678676263658,2.47140190503977,4.62208296904619));
#19930=CARTESIAN_POINT('Ctrl Pts',(3.53409308462842,2.63375189718637,4.61096917998938));
#19931=CARTESIAN_POINT('Ctrl Pts',(3.76064388996454,2.58214612691277,4.59985539093257));
#19932=CARTESIAN_POINT('Ctrl Pts',(3.84015552099323,2.36381994099575,4.58874160187577));
#19933=CARTESIAN_POINT('Ctrl Pts',(3.6998500801025,2.17860977340027,4.57762781281896));
#19934=CARTESIAN_POINT('Ctrl Pts',(3.46815072852799,2.1960405909371,4.56651402376216));
#19935=CARTESIAN_POINT('Ctrl Pts',(3.3571345103823,2.40015776866696,4.55540023470536));
#19936=CARTESIAN_POINT('Ctrl Pts',(3.46841582920963,2.6041305389052,4.54428644564855));
#19937=CARTESIAN_POINT('Ctrl Pts',(3.70013763173937,2.6212603119689,4.53317265659175));
#19938=CARTESIAN_POINT('Ctrl Pts',(3.84020232447629,2.43586801205837,4.52205886753494));
#19939=CARTESIAN_POINT('Ctrl Pts',(3.76040710518764,2.21764531427324,4.51094507847815));
#19940=CARTESIAN_POINT('Ctrl Pts',(3.53378944408678,2.16633392770918,4.49983128942133));
#19941=CARTESIAN_POINT('Ctrl Pts',(3.36777505427786,2.32889974840269,4.48871750036454));
#19942=CARTESIAN_POINT('Ctrl Pts',(3.4143187937299,2.55654443303944,4.47760371130772));
#19943=CARTESIAN_POINT('Ctrl Pts',(3.63081864137997,2.64090222813732,4.46648992225093));
#19944=CARTESIAN_POINT('Ctrl Pts',(3.81910984841827,2.50475947107891,4.45537613319412));
#19945=CARTESIAN_POINT('Ctrl Pts',(3.80684730359907,2.27272920356226,4.44426234413732));
#19946=CARTESIAN_POINT('Ctrl Pts',(3.60525512148808,2.15719129638054,4.43314855508051));
#19947=CARTESIAN_POINT('Ctrl Pts',(3.39885277598246,2.26389903533996,4.42203476602371));
#19948=CARTESIAN_POINT('Ctrl Pts',(3.3765629481812,2.49518135839549,4.4109209769669));
#19949=CARTESIAN_POINT('Ctrl Pts',(3.55878722266986,2.63934344974957,4.3998071879101));
#19950=CARTESIAN_POINT('Ctrl Pts',(3.77873475080197,2.56443107632444,4.38869339885329));
#19951=CARTESIAN_POINT('Ctrl Pts',(3.8350828706128,2.33901445723046,4.37757960979649));
#19952=CARTESIAN_POINT('Ctrl Pts',(3.67625990394949,2.16941582752504,4.36646582073968));
#19953=CARTESIAN_POINT('Ctrl Pts',(3.44762951395987,2.21087905095695,4.35535203168288));
#19954=CARTESIAN_POINT('Ctrl Pts',(3.35847730739013,2.42543572165447,4.34423824262608));
#19955=CARTESIAN_POINT('Ctrl Pts',(3.49037003538787,2.61673301642169,4.33312445356927));
#19956=CARTESIAN_POINT('Ctrl Pts',(3.72265542052987,2.60960761604941,4.32201066451248));
#19957=CARTESIAN_POINT('Ctrl Pts',(3.84257850979074,2.41071512516748,4.31089687545566));
#19958=CARTESIAN_POINT('Ctrl Pts',(3.7406568756376,2.20183613957205,4.29978308639887));
#19959=CARTESIAN_POINT('Ctrl Pts',(3.50959639242813,2.17470169312488,4.28866929734205));
#19960=CARTESIAN_POINT('Ctrl Pts',(3.41142456563631,2.29356865430551,4.28126010463752));
#19961=CARTESIAN_POINT('Ctrl Pts',(3.39833241385534,2.360627924571,4.27755550828525));
#19962=CARTESIAN_POINT('Ctrl Pts',(3.55032651029123,2.21400211999972,5.20748149723825));
#19963=CARTESIAN_POINT('Ctrl Pts',(3.48847779011663,2.2305197371096,5.20377690088598));
#19964=CARTESIAN_POINT('Ctrl Pts',(3.38363102379655,2.32987260795489,5.19636770818144));
#19965=CARTESIAN_POINT('Ctrl Pts',(3.42374108957258,2.54412674142112,5.18525391912464));
#19966=CARTESIAN_POINT('Ctrl Pts',(3.62549702318155,2.62606856404868,5.17414013006783));
#19967=CARTESIAN_POINT('Ctrl Pts',(3.8037602238433,2.50127641096634,5.16302634101103));
#19968=CARTESIAN_POINT('Ctrl Pts',(3.79559667859298,2.28369088196908,5.15191255195422));
#19969=CARTESIAN_POINT('Ctrl Pts',(3.60836267793897,2.1726112820345,5.14079876289743));
#19970=CARTESIAN_POINT('Ctrl Pts',(3.41349350034069,2.269639745597,5.12968497384062));
#19971=CARTESIAN_POINT('Ctrl Pts',(3.38932620899373,2.48600011991624,5.11857118478381));
#19972=CARTESIAN_POINT('Ctrl Pts',(3.55799583654811,2.62363776975738,5.10745739572701));
#19973=CARTESIAN_POINT('Ctrl Pts',(3.76510994947867,2.55658014925731,5.0963436066702));
#19974=CARTESIAN_POINT('Ctrl Pts',(3.82109825277221,2.34620148571036,5.08522981761341));
#19975=CARTESIAN_POINT('Ctrl Pts',(3.67471221873066,2.18506593996663,5.0741160285566));
#19976=CARTESIAN_POINT('Ctrl Pts',(3.45994154284032,2.22066161350478,5.0630022394998));
#19977=CARTESIAN_POINT('Ctrl Pts',(3.37336781169642,2.42040792753322,5.05188845044299));
#19978=CARTESIAN_POINT('Ctrl Pts',(3.49423316734106,2.60147454339935,5.04077466138619));
#19979=CARTESIAN_POINT('Ctrl Pts',(3.71190806711109,2.59812927009101,5.02966087232938));
#19980=CARTESIAN_POINT('Ctrl Pts',(3.82715226255275,2.41343400631629,5.01854708327258));
#19981=CARTESIAN_POINT('Ctrl Pts',(3.73448140669699,2.21644245550271,5.00743329421577));
#19982=CARTESIAN_POINT('Ctrl Pts',(3.51871819881407,2.18746320121053,4.99631950515897));
#19983=CARTESIAN_POINT('Ctrl Pts',(3.37735314303472,2.35302129199909,4.98520571610216));
#19984=CARTESIAN_POINT('Ctrl Pts',(3.43977928158165,2.56157952558844,4.97409192704536));
#19985=CARTESIAN_POINT('Ctrl Pts',(3.64885726014462,2.62224218767309,4.96297813798855));
#19986=CARTESIAN_POINT('Ctrl Pts',(3.81321563470729,2.47948405463168,4.95186434893176));
#19987=CARTESIAN_POINT('Ctrl Pts',(3.78241532064824,2.26397326515074,4.94075055987495));
#19988=CARTESIAN_POINT('Ctrl Pts',(3.58464819494153,2.17296928863785,4.92963677081815));
#19989=CARTESIAN_POINT('Ctrl Pts',(3.40093275047013,2.28976909698186,4.91852298176134));
#19990=CARTESIAN_POINT('Ctrl Pts',(3.39942581708757,2.50746450093999,4.90740919270454));
#19991=CARTESIAN_POINT('Ctrl Pts',(3.58150670798172,2.62679642846834,4.89629540364773));
#19992=CARTESIAN_POINT('Ctrl Pts',(3.78051471879288,2.53853901296773,4.88518161459093));
#19993=CARTESIAN_POINT('Ctrl Pts',(3.81429556031454,2.32347526776122,4.87406782553412));
#19994=CARTESIAN_POINT('Ctrl Pts',(3.65192924520447,2.17845547782099,4.86295403647733));
#19995=CARTESIAN_POINT('Ctrl Pts',(3.4420315030405,2.23621790151766,4.85184024742051));
#19996=CARTESIAN_POINT('Ctrl Pts',(3.37672411762845,2.4438919373702,4.84072645836372));
#19997=CARTESIAN_POINT('Ctrl Pts',(3.51578367947165,2.61139118517954,4.8296126693069));
#19998=CARTESIAN_POINT('Ctrl Pts',(3.73192739457257,2.58540168385487,4.81849888025011));
#19999=CARTESIAN_POINT('Ctrl Pts',(3.82731646926276,2.38971191869978,4.8073850911933));
#20000=CARTESIAN_POINT('Ctrl Pts',(3.71464020169267,2.20343895103354,4.7962713021365));
#20001=CARTESIAN_POINT('Ctrl Pts',(3.49703245740495,2.19708054064022,4.78515751307969));
#20002=CARTESIAN_POINT('Ctrl Pts',(3.37367207258585,2.37645661266209,4.77404372402289));
#20003=CARTESIAN_POINT('Ctrl Pts',(3.45747220646219,2.57738221411453,4.76292993496608));
#20004=CARTESIAN_POINT('Ctrl Pts',(3.6717296461388,2.6159478633368,4.75181614590928));
#20005=CARTESIAN_POINT('Ctrl Pts',(3.82033212723505,2.45685398423157,4.74070235685248));
#20006=CARTESIAN_POINT('Ctrl Pts',(3.7672621135368,2.24572100859114,4.72958856779567));
#20007=CARTESIAN_POINT('Ctrl Pts',(3.56109519043692,2.17580134343001,4.71847477873887));
#20008=CARTESIAN_POINT('Ctrl Pts',(3.39053828074069,2.31109325121307,4.70736098968206));
#20009=CARTESIAN_POINT('Ctrl Pts',(3.41170405813995,2.52776251443194,4.69624720062526));
#20010=CARTESIAN_POINT('Ctrl Pts',(3.60521924654496,2.62748929926577,4.68513341156846));
#20011=CARTESIAN_POINT('Ctrl Pts',(3.79395719939706,2.51899254857754,4.67401962251165));
#20012=CARTESIAN_POINT('Ctrl Pts',(3.80516392801682,2.30158056870897,4.66290583345484));
#20013=CARTESIAN_POINT('Ctrl Pts',(3.62858178660552,2.17425301045342,4.65179204439804));
#20014=CARTESIAN_POINT('Ctrl Pts',(3.42583841177484,2.25355423187469,4.64067825534123));
#20015=CARTESIAN_POINT('Ctrl Pts',(3.38250711377307,2.46689892566933,4.62956446628444));
#20016=CARTESIAN_POINT('Ctrl Pts',(3.53824952107254,2.61901027411281,4.61845067722762));
#20017=CARTESIAN_POINT('Ctrl Pts',(3.7505128420311,2.57065903491661,4.60733688817083));
#20018=CARTESIAN_POINT('Ctrl Pts',(3.82501005174943,2.36610164565372,4.59622309911402));
#20019=CARTESIAN_POINT('Ctrl Pts',(3.69355300930883,2.19257180456232,4.58510931005721));
#20020=CARTESIAN_POINT('Ctrl Pts',(3.47646583649485,2.20890334314105,4.57399552100041));
#20021=CARTESIAN_POINT('Ctrl Pts',(3.37245088448926,2.4001478189457,4.5628817319436));
#20022=CARTESIAN_POINT('Ctrl Pts',(3.47671421853432,2.59125699435405,4.55176794288681));
#20023=CARTESIAN_POINT('Ctrl Pts',(3.69382242642831,2.60730647390622,4.54065415382999));
#20024=CARTESIAN_POINT('Ctrl Pts',(3.82505390355888,2.43360598672071,4.5295403647732));
#20025=CARTESIAN_POINT('Ctrl Pts',(3.75029099014661,2.22914555908425,4.51842657571639));
#20026=CARTESIAN_POINT('Ctrl Pts',(3.53796502969918,2.18107013821379,4.50731278665959));
#20027=CARTESIAN_POINT('Ctrl Pts',(3.3824203797675,2.33338370392177,4.49619899760278));
#20028=CARTESIAN_POINT('Ctrl Pts',(3.42602882640825,2.54667191840358,4.48508520854598));
#20029=CARTESIAN_POINT('Ctrl Pts',(3.62887505589326,2.62570966761684,4.47397141948917));
#20030=CARTESIAN_POINT('Ctrl Pts',(3.80529162988842,2.49815278828994,4.46285763043237));
#20031=CARTESIAN_POINT('Ctrl Pts',(3.79380242558891,2.28075556883219,4.45174384137556));
#20032=CARTESIAN_POINT('Ctrl Pts',(3.60492370590979,2.17250408926403,4.44063005231877));
#20033=CARTESIAN_POINT('Ctrl Pts',(3.41153817701856,2.2724822774232,4.42951626326195));
#20034=CARTESIAN_POINT('Ctrl Pts',(3.39065406289825,2.48917872172821,4.41840247420516));
#20035=CARTESIAN_POINT('Ctrl Pts',(3.56138631699392,2.62424919398607,4.40728868514835));
#20036=CARTESIAN_POINT('Ctrl Pts',(3.76746279811117,2.55406118851634,4.39617489609155));
#20037=CARTESIAN_POINT('Ctrl Pts',(3.82025730936029,2.342860526055,4.38506110703474));
#20038=CARTESIAN_POINT('Ctrl Pts',(3.67145055363756,2.18395767723095,4.37394731797794));
#20039=CARTESIAN_POINT('Ctrl Pts',(3.4572387975626,2.22280601189145,4.36283352892113));
#20040=CARTESIAN_POINT('Ctrl Pts',(3.37370899766098,2.42383161137452,4.35171973986432));
#20041=CARTESIAN_POINT('Ctrl Pts',(3.49728387709496,2.60306469340852,4.34060595080753));
#20042=CARTESIAN_POINT('Ctrl Pts',(3.71492012511989,2.59638865822985,4.32949216175072));
#20043=CARTESIAN_POINT('Ctrl Pts',(3.82728023413982,2.4100393730632,4.31837837269392));
#20044=CARTESIAN_POINT('Ctrl Pts',(3.73178631386543,2.21433339402172,4.30726458363711));
#20045=CARTESIAN_POINT('Ctrl Pts',(3.51529771901994,2.18891018836724,4.29615079458031));
#20046=CARTESIAN_POINT('Ctrl Pts',(3.42331712354828,2.30028077429395,4.28874160187577));
#20047=CARTESIAN_POINT('Ctrl Pts',(3.41105063166184,2.36311093455973,4.2850370055235));
#20048=CARTESIAN_POINT('Ctrl Pts',(3.55367004230132,2.22652167256662,5.2149629944765));
#20049=CARTESIAN_POINT('Ctrl Pts',(3.49598437120782,2.24192748573719,5.21125839812423));
#20050=CARTESIAN_POINT('Ctrl Pts',(3.39819486060706,2.33459289600918,5.20384920541969));
#20051=CARTESIAN_POINT('Ctrl Pts',(3.43560511025108,2.5344255431305,5.19273541636289));
#20052=CARTESIAN_POINT('Ctrl Pts',(3.62378081371712,2.61085184614133,5.18162162730608));
#20053=CARTESIAN_POINT('Ctrl Pts',(3.79004508454469,2.4944594765428,5.17050783824928));
#20054=CARTESIAN_POINT('Ctrl Pts',(3.78243102907294,2.29151967075525,5.15939404919247));
#20055=CARTESIAN_POINT('Ctrl Pts',(3.60779978450139,2.18791685975229,5.14828026013568));
#20056=CARTESIAN_POINT('Ctrl Pts',(3.42604728819327,2.27841431903638,5.13716647107886));
#20057=CARTESIAN_POINT('Ctrl Pts',(3.40350670180884,2.48021143553957,5.12605268202207));
#20058=CARTESIAN_POINT('Ctrl Pts',(3.56082314475379,2.60858466907463,5.11493889296526));
#20059=CARTESIAN_POINT('Ctrl Pts',(3.75399636747541,2.54604070972415,5.10382510390846));
#20060=CARTESIAN_POINT('Ctrl Pts',(3.80621608745921,2.34982267390707,5.09271131485165));
#20061=CARTESIAN_POINT('Ctrl Pts',(3.66968332512291,2.19953319229768,5.08159752579485));
#20062=CARTESIAN_POINT('Ctrl Pts',(3.46936890414598,2.23273291430124,5.07048373673804));
#20063=CARTESIAN_POINT('Ctrl Pts',(3.38862246725923,2.41903426606174,5.05936994768124));
#20064=CARTESIAN_POINT('Ctrl Pts',(3.50135235290009,2.58791325368478,5.04825615862443));
#20065=CARTESIAN_POINT('Ctrl Pts',(3.70437551389675,2.58479315135706,5.03714236956764));
#20066=CARTESIAN_POINT('Ctrl Pts',(3.81186260069363,2.41252976080414,5.02602858051082));
#20067=CARTESIAN_POINT('Ctrl Pts',(3.72542943771535,2.22879774862422,5.01491479145403));
#20068=CARTESIAN_POINT('Ctrl Pts',(3.52418929226243,2.20176909343275,5.00380100239722));
#20069=CARTESIAN_POINT('Ctrl Pts',(3.39233954518956,2.35618343774151,4.99268721334042));
#20070=CARTESIAN_POINT('Ctrl Pts',(3.45056376851527,2.55070357708658,4.98157342428361));
#20071=CARTESIAN_POINT('Ctrl Pts',(3.64556866870124,2.60728302388504,4.9704596352268));
#20072=CARTESIAN_POINT('Ctrl Pts',(3.79886404991074,2.47413396784473,4.95934584617));
#20073=CARTESIAN_POINT('Ctrl Pts',(3.77013691083056,2.27312925046329,4.9482320571132));
#20074=CARTESIAN_POINT('Ctrl Pts',(3.58568152785062,2.18825076886329,4.93711826805639));
#20075=CARTESIAN_POINT('Ctrl Pts',(3.41433200477794,2.29718875996312,4.92600447899959));
#20076=CARTESIAN_POINT('Ctrl Pts',(3.41292650336706,2.5002310450071,4.91489068994278));
#20077=CARTESIAN_POINT('Ctrl Pts',(3.58275149497368,2.61153071786889,4.90377690088598));
#20078=CARTESIAN_POINT('Ctrl Pts',(3.76836423884643,2.52921392573871,4.89266311182918));
#20079=CARTESIAN_POINT('Ctrl Pts',(3.79987128552062,2.32862616199684,4.88154932277237));
#20080=CARTESIAN_POINT('Ctrl Pts',(3.64843387786428,2.19336768161237,4.87043553371557));
#20081=CARTESIAN_POINT('Ctrl Pts',(3.45266439252072,2.24724210561861,4.85932174465876));
#20082=CARTESIAN_POINT('Ctrl Pts',(3.39175285960263,2.44093756274417,4.84820795560197));
#20083=CARTESIAN_POINT('Ctrl Pts',(3.52145229597333,2.59716240442661,4.83709416654515));
#20084=CARTESIAN_POINT('Ctrl Pts',(3.72304733663125,2.57292226136356,4.82598037748836));
#20085=CARTESIAN_POINT('Ctrl Pts',(3.81201575461885,2.39040441140265,4.81486658843155));
#20086=CARTESIAN_POINT('Ctrl Pts',(3.70692374798164,2.21666951250626,4.80375279937475));
#20087=CARTESIAN_POINT('Ctrl Pts',(3.50396322221905,2.21073908792203,4.79263901031794));
#20088=CARTESIAN_POINT('Ctrl Pts',(3.3889062482905,2.37804132252749,4.78152522126113));
#20089=CARTESIAN_POINT('Ctrl Pts',(3.46706577926762,2.56544258365188,4.77041143220433));
#20090=CARTESIAN_POINT('Ctrl Pts',(3.66690151005769,2.60141237171319,4.75929764314753));
#20091=CARTESIAN_POINT('Ctrl Pts',(3.80550152997722,2.45302713177377,4.74818385409072));
#20092=CARTESIAN_POINT('Ctrl Pts',(3.75600366896275,2.25610555675324,4.73707006503392));
#20093=CARTESIAN_POINT('Ctrl Pts',(3.56371388054473,2.19089219751045,4.72595627597711));
#20094=CARTESIAN_POINT('Ctrl Pts',(3.40463718877671,2.31707758133011,4.71484248692031));
#20095=CARTESIAN_POINT('Ctrl Pts',(3.42437829368633,2.51916279536252,4.7037286978635));
#20096=CARTESIAN_POINT('Ctrl Pts',(3.60486793807048,2.61217695140159,4.69261490880671));
#20097=CARTESIAN_POINT('Ctrl Pts',(3.78090190353252,2.51098313757252,4.6815011197499));
#20098=CARTESIAN_POINT('Ctrl Pts',(3.79135430512417,2.3082051992889,4.67038733069309));
#20099=CARTESIAN_POINT('Ctrl Pts',(3.62665794113017,2.18944808312007,4.65927354163629));
#20100=CARTESIAN_POINT('Ctrl Pts',(3.43756126129826,2.26341152429244,4.64815975257949));
#20101=CARTESIAN_POINT('Ctrl Pts',(3.39714660118035,2.46239594629889,4.63704596352268));
#20102=CARTESIAN_POINT('Ctrl Pts',(3.54240595751667,2.60426865103925,4.62593217446588));
#20103=CARTESIAN_POINT('Ctrl Pts',(3.74038179409766,2.55917194292045,4.61481838540907));
#20104=CARTESIAN_POINT('Ctrl Pts',(3.80986458250562,2.36838335031169,4.60370459635227));
#20105=CARTESIAN_POINT('Ctrl Pts',(3.68725593851517,2.20653383572437,4.59259080729547));
#20106=CARTESIAN_POINT('Ctrl Pts',(3.48478094446172,2.221766095345,4.58147701823866));
#20107=CARTESIAN_POINT('Ctrl Pts',(3.38776725859624,2.40013786922444,4.57036322918186));
#20108=CARTESIAN_POINT('Ctrl Pts',(3.48501260785902,2.57838344980291,4.55924944012505));
#20109=CARTESIAN_POINT('Ctrl Pts',(3.68750722111726,2.59335263584353,4.54813565106824));
#20110=CARTESIAN_POINT('Ctrl Pts',(3.80990548264146,2.43134396138305,4.53702186201145));
#20111=CARTESIAN_POINT('Ctrl Pts',(3.74017487510557,2.24064580389526,4.52590807295464));
#20112=CARTESIAN_POINT('Ctrl Pts',(3.54214061531159,2.19580634871841,4.51479428389784));
#20113=CARTESIAN_POINT('Ctrl Pts',(3.39706570525713,2.33786765944084,4.50368049484103));
#20114=CARTESIAN_POINT('Ctrl Pts',(3.4377388590866,2.53679940376773,4.49256670578423));
#20115=CARTESIAN_POINT('Ctrl Pts',(3.62693147040654,2.61051710709635,4.48145291672742));
#20116=CARTESIAN_POINT('Ctrl Pts',(3.79147341135858,2.49154610550097,4.47033912767062));
#20117=CARTESIAN_POINT('Ctrl Pts',(3.78075754757875,2.28878193410212,4.45922533861381));
#20118=CARTESIAN_POINT('Ctrl Pts',(3.60459229033149,2.18781688214753,4.44811154955701));
#20119=CARTESIAN_POINT('Ctrl Pts',(3.42422357805467,2.28106551950643,4.43699776050021));
#20120=CARTESIAN_POINT('Ctrl Pts',(3.4047451776153,2.48317608506094,4.4258839714434));
#20121=CARTESIAN_POINT('Ctrl Pts',(3.56398541131798,2.60915493822257,4.4147701823866));
#20122=CARTESIAN_POINT('Ctrl Pts',(3.75619084542037,2.54369130070823,4.40365639332979));
#20123=CARTESIAN_POINT('Ctrl Pts',(3.80543174810779,2.34670659487954,4.39254260427299));
#20124=CARTESIAN_POINT('Ctrl Pts',(3.66664120332562,2.19849952693685,4.38142881521618));
#20125=CARTESIAN_POINT('Ctrl Pts',(3.46684808116532,2.23473297282595,4.37031502615938));
#20126=CARTESIAN_POINT('Ctrl Pts',(3.38894068793183,2.42222750109457,4.35920123710257));
#20127=CARTESIAN_POINT('Ctrl Pts',(3.50419771880206,2.58939637039535,4.34808744804578));
#20128=CARTESIAN_POINT('Ctrl Pts',(3.70718482970991,2.5831697004103,4.33697365898896));
#20129=CARTESIAN_POINT('Ctrl Pts',(3.81198195848891,2.40936362095891,4.32585986993217));
#20130=CARTESIAN_POINT('Ctrl Pts',(3.72291575209325,2.22683064847139,4.31474608087536));
#20131=CARTESIAN_POINT('Ctrl Pts',(3.52099904561175,2.2031186836096,4.30363229181856));
#20132=CARTESIAN_POINT('Ctrl Pts',(3.43520968146025,2.30699289428239,4.29622309911402));
#20133=CARTESIAN_POINT('Ctrl Pts',(3.42376884946835,2.36559394454846,4.29251850276175));
#20134=CARTESIAN_POINT('Ctrl Pts',(3.55701357431141,2.23904122513352,5.22244449171475));
#20135=CARTESIAN_POINT('Ctrl Pts',(3.50349095229901,2.25333523436478,5.21873989536248));
#20136=CARTESIAN_POINT('Ctrl Pts',(3.41275869741756,2.33931318406347,5.21133070265794));
#20137=CARTESIAN_POINT('Ctrl Pts',(3.44746913092958,2.52472434483988,5.20021691360114));
#20138=CARTESIAN_POINT('Ctrl Pts',(3.62206460425269,2.59563512823397,5.18910312454433));
#20139=CARTESIAN_POINT('Ctrl Pts',(3.77632994524609,2.48764254211926,5.17798933548754));
#20140=CARTESIAN_POINT('Ctrl Pts',(3.76926537955289,2.29934845954141,5.16687554643072));
#20141=CARTESIAN_POINT('Ctrl Pts',(3.60723689106381,2.20322243747008,5.15576175737393));
#20142=CARTESIAN_POINT('Ctrl Pts',(3.43860107604584,2.28718889247577,5.14464796831712));
#20143=CARTESIAN_POINT('Ctrl Pts',(3.41768719462395,2.47442275116291,5.13353417926031));
#20144=CARTESIAN_POINT('Ctrl Pts',(3.56365045295948,2.59353156839189,5.12242039020351));
#20145=CARTESIAN_POINT('Ctrl Pts',(3.74288278547214,2.53550127019098,5.1113066011467));
#20146=CARTESIAN_POINT('Ctrl Pts',(3.79133392214622,2.35344386210378,5.1001928120899));
#20147=CARTESIAN_POINT('Ctrl Pts',(3.66465443151516,2.21400044462873,5.0890790230331));
#20148=CARTESIAN_POINT('Ctrl Pts',(3.47879626545164,2.24480421509772,5.0779652339763));
#20149=CARTESIAN_POINT('Ctrl Pts',(3.40387712282204,2.41766060459026,5.06685144491948));
#20150=CARTESIAN_POINT('Ctrl Pts',(3.50847153845911,2.57435196397021,5.05573765586269));
#20151=CARTESIAN_POINT('Ctrl Pts',(3.69684296068241,2.57145703262312,5.04462386680587));
#20152=CARTESIAN_POINT('Ctrl Pts',(3.7965729388345,2.41162551529198,5.03351007774909));
#20153=CARTESIAN_POINT('Ctrl Pts',(3.71637746873371,2.24115304174574,5.02239628869227));
#20154=CARTESIAN_POINT('Ctrl Pts',(3.5296603857108,2.21607498565497,5.01128249963547));
#20155=CARTESIAN_POINT('Ctrl Pts',(3.40732594734439,2.35934558348393,5.00016871057866));
#20156=CARTESIAN_POINT('Ctrl Pts',(3.46134825544889,2.53982762858472,4.98905492152187));
#20157=CARTESIAN_POINT('Ctrl Pts',(3.64228007725786,2.59232386009698,4.97794113246505));
#20158=CARTESIAN_POINT('Ctrl Pts',(3.7845124651142,2.46878388105777,4.96682734340826));
#20159=CARTESIAN_POINT('Ctrl Pts',(3.75785850101288,2.28228523577585,4.95571355435144));
#20160=CARTESIAN_POINT('Ctrl Pts',(3.58671486075972,2.20353224908873,4.94459976529465));
#20161=CARTESIAN_POINT('Ctrl Pts',(3.42773125908574,2.30460842294439,4.93348597623783));
#20162=CARTESIAN_POINT('Ctrl Pts',(3.42642718964655,2.4929975890742,4.92237218718104));
#20163=CARTESIAN_POINT('Ctrl Pts',(3.58399628196565,2.59626500726946,4.91125839812423));
#20164=CARTESIAN_POINT('Ctrl Pts',(3.75621375889998,2.51988883850969,4.90014460906743));
#20165=CARTESIAN_POINT('Ctrl Pts',(3.7854470107267,2.33377705623246,4.88903082001062));
#20166=CARTESIAN_POINT('Ctrl Pts',(3.6449385105241,2.20827988540375,4.87791703095382));
#20167=CARTESIAN_POINT('Ctrl Pts',(3.46329728200094,2.25826630971955,4.86680324189701));
#20168=CARTESIAN_POINT('Ctrl Pts',(3.40678160157682,2.43798318811813,4.85568945284022));
#20169=CARTESIAN_POINT('Ctrl Pts',(3.527120912475,2.58293362367368,4.8445756637834));
#20170=CARTESIAN_POINT('Ctrl Pts',(3.71416727868993,2.56044283887224,4.8334618747266));
#20171=CARTESIAN_POINT('Ctrl Pts',(3.79671503997494,2.39109690410553,4.82234808566979));
#20172=CARTESIAN_POINT('Ctrl Pts',(3.69920729427062,2.22990007397898,4.811234296613));
#20173=CARTESIAN_POINT('Ctrl Pts',(3.51089398703315,2.22439763520385,4.80012050755619));
#20174=CARTESIAN_POINT('Ctrl Pts',(3.40414042399517,2.37962603239289,4.78900671849938));
#20175=CARTESIAN_POINT('Ctrl Pts',(3.47665935207306,2.55350295318923,4.77789292944258));
#20176=CARTESIAN_POINT('Ctrl Pts',(3.66207337397658,2.58687688008957,4.76677914038578));
#20177=CARTESIAN_POINT('Ctrl Pts',(3.79067093271938,2.44920027931597,4.75566535132897));
#20178=CARTESIAN_POINT('Ctrl Pts',(3.7447452243887,2.26649010491534,4.74455156227217));
#20179=CARTESIAN_POINT('Ctrl Pts',(3.56633257065254,2.20598305159089,4.73343777321536));
#20180=CARTESIAN_POINT('Ctrl Pts',(3.41873609681274,2.32306191144714,4.72232398415856));
#20181=CARTESIAN_POINT('Ctrl Pts',(3.4370525292327,2.5105630762931,4.71121019510175));
#20182=CARTESIAN_POINT('Ctrl Pts',(3.604516629596,2.59686460353741,4.70009640604495));
#20183=CARTESIAN_POINT('Ctrl Pts',(3.76784660766799,2.50297372656749,4.68898261698814));
#20184=CARTESIAN_POINT('Ctrl Pts',(3.77754468223151,2.31482982986883,4.67786882793134));
#20185=CARTESIAN_POINT('Ctrl Pts',(3.62473409565482,2.20464315578672,4.66675503887454));
#20186=CARTESIAN_POINT('Ctrl Pts',(3.44928411082169,2.27326881671019,4.65564124981774));
#20187=CARTESIAN_POINT('Ctrl Pts',(3.41178608858762,2.45789296692846,4.64452746076093));
#20188=CARTESIAN_POINT('Ctrl Pts',(3.5465623939608,2.58952702796569,4.63341367170412));
#20189=CARTESIAN_POINT('Ctrl Pts',(3.73025074616421,2.54768485092428,4.62229988264732));
#20190=CARTESIAN_POINT('Ctrl Pts',(3.79471911326182,2.37066505496967,4.61118609359052));
#20191=CARTESIAN_POINT('Ctrl Pts',(3.6809588677215,2.22049586688641,4.60007230453371));
#20192=CARTESIAN_POINT('Ctrl Pts',(3.49309605242859,2.23462884754895,4.58895851547691));
#20193=CARTESIAN_POINT('Ctrl Pts',(3.4030836327032,2.40012791950318,4.5778447264201));
#20194=CARTESIAN_POINT('Ctrl Pts',(3.49331099718372,2.56550990525176,4.56673093736331));
#20195=CARTESIAN_POINT('Ctrl Pts',(3.6811920158062,2.57939879778085,4.55561714830649));
#20196=CARTESIAN_POINT('Ctrl Pts',(3.79475706172405,2.42908193604538,4.5445033592497));
#20197=CARTESIAN_POINT('Ctrl Pts',(3.73005876006454,2.25214604870627,4.53338957019289));
#20198=CARTESIAN_POINT('Ctrl Pts',(3.54631620092399,2.21054255922302,4.52227578113609));
#20199=CARTESIAN_POINT('Ctrl Pts',(3.41171103074677,2.34235161495991,4.51116199207928));
#20200=CARTESIAN_POINT('Ctrl Pts',(3.44944889176494,2.52692688913187,4.50004820302248));
#20201=CARTESIAN_POINT('Ctrl Pts',(3.62498788491984,2.59532454657587,4.48893441396567));
#20202=CARTESIAN_POINT('Ctrl Pts',(3.77765519282873,2.484939422712,4.47782062490886));
#20203=CARTESIAN_POINT('Ctrl Pts',(3.76771266956859,2.29680829937205,4.46670683585207));
#20204=CARTESIAN_POINT('Ctrl Pts',(3.6042608747532,2.20312967503102,4.45559304679526));
#20205=CARTESIAN_POINT('Ctrl Pts',(3.43690897909078,2.28964876158967,4.44447925773845));
#20206=CARTESIAN_POINT('Ctrl Pts',(3.41883629233234,2.47717344839367,4.43336546868165));
#20207=CARTESIAN_POINT('Ctrl Pts',(3.56658450564204,2.59406068245907,4.42225167962485));
#20208=CARTESIAN_POINT('Ctrl Pts',(3.74491889272957,2.53332141290012,4.41113789056804));
#20209=CARTESIAN_POINT('Ctrl Pts',(3.7906061868553,2.35055266370407,4.40002410151124));
#20210=CARTESIAN_POINT('Ctrl Pts',(3.66183185301368,2.21304137664276,4.38891031245443));
#20211=CARTESIAN_POINT('Ctrl Pts',(3.47645736476805,2.24665993376045,4.37779652339763));
#20212=CARTESIAN_POINT('Ctrl Pts',(3.40417237820268,2.42062339081462,4.36668273434083));
#20213=CARTESIAN_POINT('Ctrl Pts',(3.51111156050916,2.57572804738218,4.35556894528402));
#20214=CARTESIAN_POINT('Ctrl Pts',(3.69944953429992,2.56995074259074,4.34445515622722));
#20215=CARTESIAN_POINT('Ctrl Pts',(3.796683682838,2.40868786885462,4.33334136717041));
#20216=CARTESIAN_POINT('Ctrl Pts',(3.71404519032108,2.23932790292106,4.32222757811361));
#20217=CARTESIAN_POINT('Ctrl Pts',(3.52670037220356,2.21732717885196,4.3111137890568));
#20218=CARTESIAN_POINT('Ctrl Pts',(3.44710223937223,2.31370501427082,4.30370459635227));
#20219=CARTESIAN_POINT('Ctrl Pts',(3.43648706727485,2.36807695453719,4.3));
#20220=CARTESIAN_POINT('Ctrl Pts',(3.43361558566414,2.40009421455432,5.13785196366098));
#20221=CARTESIAN_POINT('Ctrl Pts',(3.43350387426567,2.42168271797136,5.13641270219409));
#20222=CARTESIAN_POINT('Ctrl Pts',(3.43740295903752,2.4432325339629,5.1349734407272));
#20223=CARTESIAN_POINT('Ctrl Pts',(3.44550005125019,2.46306857758655,5.13353417926031));
#20224=CARTESIAN_POINT('Ctrl Pts',(3.46634161406913,2.51412569023923,5.12982958290805));
#20225=CARTESIAN_POINT('Ctrl Pts',(3.5149960335143,2.55382862931556,5.12612498655578));
#20226=CARTESIAN_POINT('Ctrl Pts',(3.56919529865567,2.56400838248691,5.12242039020351));
#20227=CARTESIAN_POINT('Ctrl Pts',(3.62339456379703,2.57418813565826,5.11871579385124));
#20228=CARTESIAN_POINT('Ctrl Pts',(3.68313867463459,2.55484470292462,5.11501119749897));
#20229=CARTESIAN_POINT('Ctrl Pts',(3.72108591949905,2.51483008520994,5.1113066011467));
#20230=CARTESIAN_POINT('Ctrl Pts',(3.7590331643635,2.47481546749525,5.10760200479444));
#20231=CARTESIAN_POINT('Ctrl Pts',(3.77518354325486,2.41412966479952,5.10389740844217));
#20232=CARTESIAN_POINT('Ctrl Pts',(3.76214548426203,2.36054619387247,5.1001928120899));
#20233=CARTESIAN_POINT('Ctrl Pts',(3.7491074252692,2.30696272294543,5.09648821573763));
#20234=CARTESIAN_POINT('Ctrl Pts',(3.70688092839218,2.26048158378708,5.09278361938537));
#20235=CARTESIAN_POINT('Ctrl Pts',(3.65479131894308,2.24237497595273,5.0890790230331));
#20236=CARTESIAN_POINT('Ctrl Pts',(3.60270170949399,2.22426836811839,5.08537442668083));
#20237=CARTESIAN_POINT('Ctrl Pts',(3.54074898747281,2.23453629160805,5.08166983032856));
#20238=CARTESIAN_POINT('Ctrl Pts',(3.49728610269062,2.26847965160164,5.0779652339763));
#20239=CARTESIAN_POINT('Ctrl Pts',(3.45773596364813,2.29936726097326,5.07459414387119));
#20240=CARTESIAN_POINT('Ctrl Pts',(3.43349641790554,2.34985942255505,5.07122305376608));
#20241=CARTESIAN_POINT('Ctrl Pts',(3.43317938608394,2.40008640134203,5.06785196366098));
#20242=CARTESIAN_POINT('Ctrl Pts',(3.54698297828114,2.20148256743283,5.2));
#20243=CARTESIAN_POINT('Ctrl Pts',(3.5345795220974,2.20607510740599,5.2));
#20244=CARTESIAN_POINT('Ctrl Pts',(3.52273022202852,2.21193437307052,5.2));
#20245=CARTESIAN_POINT('Ctrl Pts',(3.51155282869243,2.21889712518446,5.2));
#20246=CARTESIAN_POINT('Ctrl Pts',(3.50588663673039,2.22242677551307,5.2));
#20247=CARTESIAN_POINT('Ctrl Pts',(3.50039354941666,2.2262407482932,5.2));
#20248=CARTESIAN_POINT('Ctrl Pts',(3.49509234222245,2.23032135431632,5.2));
#20249=CARTESIAN_POINT('Ctrl Pts',(3.49050523644823,2.2338522805309,5.2));
#20250=CARTESIAN_POINT('Ctrl Pts',(3.48606182302158,2.23758289719759,5.2));
#20251=CARTESIAN_POINT('Ctrl Pts',(3.48177607353762,2.24150262969935,5.2));
#20252=CARTESIAN_POINT('Ctrl Pts',(3.4786657164721,2.24434735212827,5.2));
#20253=CARTESIAN_POINT('Ctrl Pts',(3.47564458925343,2.24728626535177,5.2));
#20254=CARTESIAN_POINT('Ctrl Pts',(3.47272209234032,2.25030915184069,5.2));
#20255=CARTESIAN_POINT('Ctrl Pts',(3.4637771038367,2.25956140622969,5.2));
#20256=CARTESIAN_POINT('Ctrl Pts',(3.45573639448352,2.26961351156597,5.2));
#20257=CARTESIAN_POINT('Ctrl Pts',(3.44873900472013,2.28033442966861,5.2));
#20258=CARTESIAN_POINT('Ctrl Pts',(3.44420815653473,2.28727628284152,5.2));
#20259=CARTESIAN_POINT('Ctrl Pts',(3.44011557094646,2.29449912284867,5.2));
#20260=CARTESIAN_POINT('Ctrl Pts',(3.43651072814608,2.30197002765831,5.2));
#20261=CARTESIAN_POINT('Ctrl Pts',(3.43484397915084,2.30542430396786,5.2));
#20262=CARTESIAN_POINT('Ctrl Pts',(3.43328563163244,2.30892352292903,5.2));
#20263=CARTESIAN_POINT('Ctrl Pts',(3.43184081732517,2.31246073059787,5.2));
#20264=CARTESIAN_POINT('Ctrl Pts',(3.42783869836044,2.3222587550377,5.2));
#20265=CARTESIAN_POINT('Ctrl Pts',(3.42470154623616,2.33235626573064,5.2));
#20266=CARTESIAN_POINT('Ctrl Pts',(3.42252347569321,2.34267987754179,5.2));
#20267=CARTESIAN_POINT('Ctrl Pts',(3.42066968522458,2.35146646769115,5.2));
#20268=CARTESIAN_POINT('Ctrl Pts',(3.41951139095334,2.36041732716722,5.2));
#20269=CARTESIAN_POINT('Ctrl Pts',(3.41903596356978,2.36945415649734,5.2));
#20270=CARTESIAN_POINT('Ctrl Pts',(3.41886682155969,2.37266917424891,5.2));
#20271=CARTESIAN_POINT('Ctrl Pts',(3.41878447232058,2.37589363434567,5.2));
#20272=CARTESIAN_POINT('Ctrl Pts',(3.41878798568376,2.3791143017356,5.2));
#20273=CARTESIAN_POINT('Ctrl Pts',(3.41880075844281,2.39082297128446,5.2));
#20274=CARTESIAN_POINT('Ctrl Pts',(3.41994282155898,2.40251786108517,5.2));
#20275=CARTESIAN_POINT('Ctrl Pts',(3.42216878897262,2.41402665747967,5.2));
#20276=CARTESIAN_POINT('Ctrl Pts',(3.42331180168116,2.41993631296624,5.2));
#20277=CARTESIAN_POINT('Ctrl Pts',(3.42474130312271,2.42579671745434,5.2));
#20278=CARTESIAN_POINT('Ctrl Pts',(3.4264550762976,2.43158227576526,5.2));
#20279=CARTESIAN_POINT('Ctrl Pts',(3.42814231216907,2.43727824630656,5.2));
#20280=CARTESIAN_POINT('Ctrl Pts',(3.43010783958643,2.44290710782216,5.2));
#20281=CARTESIAN_POINT('Ctrl Pts',(3.43233768577066,2.4484115412056,5.2));
#20282=CARTESIAN_POINT('Ctrl Pts',(3.43579440729991,2.4569445483329,5.2));
#20283=CARTESIAN_POINT('Ctrl Pts',(3.43988798414899,2.46519216359733,5.2));
#20284=CARTESIAN_POINT('Ctrl Pts',(3.44460907372922,2.4730585225122,5.2));
#20285=CARTESIAN_POINT('Ctrl Pts',(3.44702309019998,2.47708079738387,5.2));
#20286=CARTESIAN_POINT('Ctrl Pts',(3.44960209705083,2.48100348334585,5.2));
#20287=CARTESIAN_POINT('Ctrl Pts',(3.45233605468006,2.48480007154667,5.2));
#20288=CARTESIAN_POINT('Ctrl Pts',(3.45777065901345,2.49234698978257,5.2));
#20289=CARTESIAN_POINT('Ctrl Pts',(3.46382415870923,2.499410402925,5.2));
#20290=CARTESIAN_POINT('Ctrl Pts',(3.47049190322584,2.5058791831385,5.2));
#20291=CARTESIAN_POINT('Ctrl Pts',(3.47127037259775,2.50663442312367,5.2));
#20292=CARTESIAN_POINT('Ctrl Pts',(3.47205722899383,2.5073815321984,5.2));
#20293=CARTESIAN_POINT('Ctrl Pts',(3.47285231527688,2.50812044463164,5.2));
#20294=CARTESIAN_POINT('Origin',(3.6,2.4,4.7));
#20295=CARTESIAN_POINT('Origin',(3.6,-2.4,4.2));
#20296=CARTESIAN_POINT('Origin',(-3.6,-2.4,4.2));
#20297=CARTESIAN_POINT('Origin',(-3.6,2.4,4.2));
#20298=CARTESIAN_POINT('Origin',(3.6,2.4,4.2));
#20299=CARTESIAN_POINT('Origin',(-4.6,0.,0.3));
#20300=CARTESIAN_POINT('',(-4.9,3.67394039744206E-17,0.6));
#20301=CARTESIAN_POINT('Origin',(-4.6,0.,0.6));
#20302=CARTESIAN_POINT('',(-4.9,3.67394039744206E-17,0.));
#20303=CARTESIAN_POINT('',(-4.9,3.67394039744206E-17,0.3));
#20304=CARTESIAN_POINT('Origin',(-4.6,0.,0.));
#20305=CARTESIAN_POINT('Origin',(4.6,0.,0.3));
#20306=CARTESIAN_POINT('',(4.3,3.67394039744206E-17,0.6));
#20307=CARTESIAN_POINT('Origin',(4.6,0.,0.6));
#20308=CARTESIAN_POINT('',(4.3,3.67394039744206E-17,0.));
#20309=CARTESIAN_POINT('',(4.3,3.67394039744206E-17,0.3));
#20310=CARTESIAN_POINT('Origin',(4.6,0.,0.));
#20311=CARTESIAN_POINT('Origin',(5.2,1.,0.));
#20312=CARTESIAN_POINT('',(5.2,1.,0.));
#20313=CARTESIAN_POINT('',(4.,1.,0.));
#20314=CARTESIAN_POINT('',(5.2,1.,0.));
#20315=CARTESIAN_POINT('',(4.,1.,0.6));
#20316=CARTESIAN_POINT('',(4.,1.,0.));
#20317=CARTESIAN_POINT('',(5.2,1.,0.6));
#20318=CARTESIAN_POINT('',(5.2,1.,0.6));
#20319=CARTESIAN_POINT('',(5.2,1.,0.));
#20320=CARTESIAN_POINT('Origin',(5.2,-1.,0.));
#20321=CARTESIAN_POINT('',(5.2,-1.,0.));
#20322=CARTESIAN_POINT('',(5.2,-1.,0.));
#20323=CARTESIAN_POINT('',(5.2,-1.,0.6));
#20324=CARTESIAN_POINT('',(5.2,-1.,0.6));
#20325=CARTESIAN_POINT('',(5.2,-1.,0.));
#20326=CARTESIAN_POINT('Origin',(4.,-1.,0.));
#20327=CARTESIAN_POINT('',(4.,-1.,0.));
#20328=CARTESIAN_POINT('',(4.,-1.,0.));
#20329=CARTESIAN_POINT('',(4.,-1.,0.6));
#20330=CARTESIAN_POINT('',(4.,-1.,0.6));
#20331=CARTESIAN_POINT('',(4.,-1.,0.));
#20332=CARTESIAN_POINT('Origin',(4.6,0.,0.6));
#20333=CARTESIAN_POINT('',(4.,-1.4,0.6));
#20334=CARTESIAN_POINT('Origin',(-4.,1.,0.));
#20335=CARTESIAN_POINT('',(-4.,1.,0.));
#20336=CARTESIAN_POINT('',(-5.2,1.,0.));
#20337=CARTESIAN_POINT('',(-4.,1.,0.));
#20338=CARTESIAN_POINT('',(-5.2,1.,0.6));
#20339=CARTESIAN_POINT('',(-5.2,1.,0.));
#20340=CARTESIAN_POINT('',(-4.,1.,0.6));
#20341=CARTESIAN_POINT('',(-4.,1.,0.6));
#20342=CARTESIAN_POINT('',(-4.,1.,0.));
#20343=CARTESIAN_POINT('Origin',(-5.2,-1.,0.));
#20344=CARTESIAN_POINT('',(-5.2,-1.,0.));
#20345=CARTESIAN_POINT('',(-4.,-1.,0.));
#20346=CARTESIAN_POINT('',(-5.2,-1.,0.));
#20347=CARTESIAN_POINT('',(-4.,-1.,0.6));
#20348=CARTESIAN_POINT('',(-4.,-1.,0.));
#20349=CARTESIAN_POINT('',(-5.2,-1.,0.6));
#20350=CARTESIAN_POINT('',(-5.2,-1.,0.6));
#20351=CARTESIAN_POINT('',(-5.2,-1.,0.));
#20352=CARTESIAN_POINT('Origin',(-5.2,1.,0.));
#20353=CARTESIAN_POINT('',(-5.2,1.,0.));
#20354=CARTESIAN_POINT('',(-5.2,1.,0.6));
#20355=CARTESIAN_POINT('Origin',(-4.6,0.,0.6));
#20356=CARTESIAN_POINT('',(-4.,1.4,0.6));
#20357=CARTESIAN_POINT('Origin',(0.,0.,0.8));
#20358=CARTESIAN_POINT('',(-0.65,-7.9602041944578E-17,1.6));
#20359=CARTESIAN_POINT('Origin',(0.,0.,1.6));
#20360=CARTESIAN_POINT('',(-0.65,-7.9602041944578E-17,0.8));
#20361=CARTESIAN_POINT('',(-0.65,-7.9602041944578E-17,0.8));
#20362=CARTESIAN_POINT('Origin',(0.,0.,0.8));
#20363=CARTESIAN_POINT('Origin',(0.,0.,0.8));
#20364=CARTESIAN_POINT('',(-0.8,-9.79717439317883E-17,1.6));
#20365=CARTESIAN_POINT('Origin',(0.,0.,1.6));
#20366=CARTESIAN_POINT('',(-0.8,-9.79717439317883E-17,0.8));
#20367=CARTESIAN_POINT('Origin',(0.,0.,1.6));
#20368=CARTESIAN_POINT('Origin',(-3.2,-2.,5.2));
#20369=CARTESIAN_POINT('',(-3.2,-1.,5.2));
#20370=CARTESIAN_POINT('Origin',(0.,0.,0.8));
#20371=CARTESIAN_POINT('Origin',(4.,2.8,0.));
#20372=CARTESIAN_POINT('',(4.,2.8,0.));
#20373=CARTESIAN_POINT('',(-4.,2.8,0.));
#20374=CARTESIAN_POINT('',(4.,2.8,0.));
#20375=CARTESIAN_POINT('',(-4.,2.8,5.2));
#20376=CARTESIAN_POINT('',(-4.,2.8,0.));
#20377=CARTESIAN_POINT('',(4.,2.8,5.2));
#20378=CARTESIAN_POINT('',(4.,2.8,5.2));
#20379=CARTESIAN_POINT('',(4.,2.8,0.));
#20380=CARTESIAN_POINT('Origin',(4.,-2.8,0.));
#20381=CARTESIAN_POINT('',(4.,-2.8,0.));
#20382=CARTESIAN_POINT('',(4.,-2.8,5.2));
#20383=CARTESIAN_POINT('',(4.,-2.8,5.2));
#20384=CARTESIAN_POINT('',(4.,-2.8,0.));
#20385=CARTESIAN_POINT('',(4.,-2.8,0.));
#20386=CARTESIAN_POINT('',(4.,-2.8,0.));
#20387=CARTESIAN_POINT('Origin',(-4.,-2.8,0.));
#20388=CARTESIAN_POINT('',(-4.,-2.8,0.));
#20389=CARTESIAN_POINT('',(-4.,-2.8,0.));
#20390=CARTESIAN_POINT('',(-4.,-2.8,5.2));
#20391=CARTESIAN_POINT('',(-4.,-2.8,5.2));
#20392=CARTESIAN_POINT('',(-4.,-2.8,0.));
#20393=CARTESIAN_POINT('Origin',(-4.,2.8,0.));
#20394=CARTESIAN_POINT('',(-4.,2.8,0.));
#20395=CARTESIAN_POINT('',(-4.,2.8,5.2));
#20396=CARTESIAN_POINT('',(-4.,2.8,0.));
#20397=CARTESIAN_POINT('Origin',(0.,0.,5.2));
#20398=CARTESIAN_POINT('Origin',(0.,0.,0.));
#20399=CARTESIAN_POINT('',(0.,0.,0.));
#20400=CARTESIAN_POINT('Origin',(3.6,-2.4,5.5));
#20401=CARTESIAN_POINT('',(3.35,-2.4,5.8));
#20402=CARTESIAN_POINT('Origin',(3.6,-2.4,5.8));
#20403=CARTESIAN_POINT('',(3.35,-2.4,5.2));
#20404=CARTESIAN_POINT('',(3.35,-2.4,5.5));
#20405=CARTESIAN_POINT('Origin',(3.6,-2.4,5.2));
#20406=CARTESIAN_POINT('Origin',(-3.6,-2.4,5.5));
#20407=CARTESIAN_POINT('',(-3.85,-2.4,5.8));
#20408=CARTESIAN_POINT('Origin',(-3.6,-2.4,5.8));
#20409=CARTESIAN_POINT('',(-3.85,-2.4,5.2));
#20410=CARTESIAN_POINT('',(-3.85,-2.4,5.5));
#20411=CARTESIAN_POINT('Origin',(-3.6,-2.4,5.2));
#20412=CARTESIAN_POINT('Origin',(-3.6,2.4,5.5));
#20413=CARTESIAN_POINT('',(-3.85,2.4,5.8));
#20414=CARTESIAN_POINT('Origin',(-3.6,2.4,5.8));
#20415=CARTESIAN_POINT('',(-3.85,2.4,5.2));
#20416=CARTESIAN_POINT('',(-3.85,2.4,5.5));
#20417=CARTESIAN_POINT('Origin',(-3.6,2.4,5.2));
#20418=CARTESIAN_POINT('Origin',(3.6,2.4,5.5));
#20419=CARTESIAN_POINT('',(3.35,2.4,5.8));
#20420=CARTESIAN_POINT('Origin',(3.6,2.4,5.8));
#20421=CARTESIAN_POINT('',(3.35,2.4,5.2));
#20422=CARTESIAN_POINT('',(3.35,2.4,5.5));
#20423=CARTESIAN_POINT('Origin',(3.6,2.4,5.2));
#20424=CARTESIAN_POINT('Origin',(0.,0.,5.5));
#20425=CARTESIAN_POINT('',(-0.6,7.34788079488412E-17,5.8));
#20426=CARTESIAN_POINT('Origin',(0.,0.,5.8));
#20427=CARTESIAN_POINT('',(-0.6,7.34788079488412E-17,5.2));
#20428=CARTESIAN_POINT('',(-0.6,7.34788079488412E-17,5.5));
#20429=CARTESIAN_POINT('Origin',(0.,0.,5.2));
#20430=CARTESIAN_POINT('Origin',(4.,2.8,5.2));
#20431=CARTESIAN_POINT('',(4.,2.8,5.2));
#20432=CARTESIAN_POINT('',(-4.,2.8,5.2));
#20433=CARTESIAN_POINT('',(4.,2.8,5.2));
#20434=CARTESIAN_POINT('',(-4.,2.8,5.8));
#20435=CARTESIAN_POINT('',(-4.,2.8,5.2));
#20436=CARTESIAN_POINT('',(4.,2.8,5.8));
#20437=CARTESIAN_POINT('',(4.,2.8,5.8));
#20438=CARTESIAN_POINT('',(4.,2.8,5.2));
#20439=CARTESIAN_POINT('Origin',(4.,-2.8,5.2));
#20440=CARTESIAN_POINT('',(4.,-2.8,5.2));
#20441=CARTESIAN_POINT('',(4.,-2.8,5.2));
#20442=CARTESIAN_POINT('',(4.,-2.8,5.8));
#20443=CARTESIAN_POINT('',(4.,-2.8,5.8));
#20444=CARTESIAN_POINT('',(4.,-2.8,5.2));
#20445=CARTESIAN_POINT('Origin',(-4.,-2.8,5.2));
#20446=CARTESIAN_POINT('',(-4.,-2.8,5.2));
#20447=CARTESIAN_POINT('',(-4.,-2.8,5.2));
#20448=CARTESIAN_POINT('',(-4.,-2.8,5.8));
#20449=CARTESIAN_POINT('',(-4.,-2.8,5.8));
#20450=CARTESIAN_POINT('',(-4.,-2.8,5.2));
#20451=CARTESIAN_POINT('Origin',(-4.,2.8,5.2));
#20452=CARTESIAN_POINT('',(-4.,2.8,5.2));
#20453=CARTESIAN_POINT('',(-4.,2.8,5.8));
#20454=CARTESIAN_POINT('Origin',(0.,0.,5.8));
#20455=CARTESIAN_POINT('Origin',(0.,0.,5.2));
#20456=CARTESIAN_POINT('',(0.,0.,0.));
#20457=CARTESIAN_POINT('Origin',(0.,0.,0.));
#20458=CARTESIAN_POINT('',(-0.8,-9.79717439317883E-17,0.));
#20459=CARTESIAN_POINT('Origin',(0.,0.,0.));
#20460=CARTESIAN_POINT('',(-0.6,-7.34788079488412E-17,0.));
#20461=CARTESIAN_POINT('Origin',(0.,0.,0.));
#20462=CARTESIAN_POINT('Origin',(0.,0.,-0.2));
#20463=CARTESIAN_POINT('',(-0.8,-9.79717439317883E-17,-0.2));
#20464=CARTESIAN_POINT('',(-0.8,-9.79717439317883E-17,-0.2));
#20465=CARTESIAN_POINT('Origin',(0.,0.,-0.2));
#20466=CARTESIAN_POINT('Origin',(0.,0.,-0.2));
#20467=CARTESIAN_POINT('',(-0.4,-4.89858719658941E-17,-0.2));
#20468=CARTESIAN_POINT('Origin',(0.,0.,-0.2));
#20469=CARTESIAN_POINT('Origin',(0.,0.,0.));
#20470=CARTESIAN_POINT('',(-0.4,-4.89858719658941E-17,0.8));
#20471=CARTESIAN_POINT('Origin',(0.,0.,0.8));
#20472=CARTESIAN_POINT('',(-0.4,-4.89858719658941E-17,0.));
#20473=CARTESIAN_POINT('Origin',(0.,0.,0.));
#20474=CARTESIAN_POINT('',(-0.6,-7.34788079488412E-17,0.8));
#20475=CARTESIAN_POINT('Origin',(0.,0.,0.8));
#20476=CARTESIAN_POINT('',(-0.6,-7.34788079488412E-17,0.));
#20477=CARTESIAN_POINT('Origin',(0.,0.,0.8));
#20478=CARTESIAN_POINT('',(0.,0.,0.));
#20479=CARTESIAN_POINT('Origin',(0.6,1.,2.15));
#20480=CARTESIAN_POINT('',(0.473748222256554,0.999995809921948,2.01934196736194));
#20481=CARTESIAN_POINT('',(0.473622351265484,0.999839631194249,2.00565803263806));
#20482=CARTESIAN_POINT('',(0.47355,1.,2.15));
#20483=CARTESIAN_POINT('',(0.504188384727762,1.08252112989365,2.));
#20484=CARTESIAN_POINT('Ctrl Pts',(0.473622351265484,0.999839631194249,
2.00565803263806));
#20485=CARTESIAN_POINT('Ctrl Pts',(0.473885391482026,1.02975027328269,2.00377202175871));
#20486=CARTESIAN_POINT('Ctrl Pts',(0.484630619730662,1.05981347843636,2.00188601087935));
#20487=CARTESIAN_POINT('Ctrl Pts',(0.504188384727762,1.08252112989365,2.));
#20488=CARTESIAN_POINT('',(0.695988975197609,1.08263517233072,2.));
#20489=CARTESIAN_POINT('Origin',(0.6,1.,2.));
#20490=CARTESIAN_POINT('Ctrl Pts',(0.69598984030289,1.08263572859344,2.));
#20491=CARTESIAN_POINT('Ctrl Pts',(0.670163701400848,1.11242100165145,2.0024908160387));
#20492=CARTESIAN_POINT('Ctrl Pts',(0.629259702670384,1.12936970915052,2.0049816320774));
#20493=CARTESIAN_POINT('Ctrl Pts',(0.589969605604523,1.12624206673302,2.0074724481161));
#20494=CARTESIAN_POINT('Ctrl Pts',(0.548691445154515,1.12295616684523,2.01008929846199));
#20495=CARTESIAN_POINT('Ctrl Pts',(0.509194644046665,1.09751080441727,2.01270614880789));
#20496=CARTESIAN_POINT('Ctrl Pts',(0.489166147389288,1.06128256435802,2.01532299915378));
#20497=CARTESIAN_POINT('Ctrl Pts',(0.478912868232585,1.04273607706854,2.01666265522317));
#20498=CARTESIAN_POINT('Ctrl Pts',(0.473761783314308,1.02136364588323,2.01800231129256));
#20499=CARTESIAN_POINT('Ctrl Pts',(0.473748222256554,0.999995809921948,
2.01934196736194));
#20500=CARTESIAN_POINT('Origin',(0.6,1.,2.15));
#20501=CARTESIAN_POINT('',(0.473418004372097,0.999922226677399,2.06934196736194));
#20502=CARTESIAN_POINT('',(0.473391518308752,1.00006258785156,2.05565803263806));
#20503=CARTESIAN_POINT('',(0.47355,1.,2.15));
#20504=CARTESIAN_POINT('Ctrl Pts',(0.473391518308752,1.00006258785156,2.05565803263806));
#20505=CARTESIAN_POINT('Ctrl Pts',(0.473368951434719,1.00377931266751,2.05542330751329));
#20506=CARTESIAN_POINT('Ctrl Pts',(0.473518765465857,1.00749417831325,2.05518858238852));
#20507=CARTESIAN_POINT('Ctrl Pts',(0.473846950690071,1.01119320034366,2.05495385726375));
#20508=CARTESIAN_POINT('Ctrl Pts',(0.477505747839885,1.05243201995956,2.05233700691785));
#20509=CARTESIAN_POINT('Ctrl Pts',(0.503334424526069,1.09170162561774,2.04972015657196));
#20510=CARTESIAN_POINT('Ctrl Pts',(0.539751219345993,1.1113984538297,2.04710330622607));
#20511=CARTESIAN_POINT('Ctrl Pts',(0.576168014165918,1.13109528204167,2.04448645588018));
#20512=CARTESIAN_POINT('Ctrl Pts',(0.623172927119585,1.13121933280741,2.04186960553428));
#20513=CARTESIAN_POINT('Ctrl Pts',(0.659688152943108,1.11170438100077,2.03925275518839));
#20514=CARTESIAN_POINT('Ctrl Pts',(0.69620337876663,1.09218942919414,2.0366359048425));
#20515=CARTESIAN_POINT('Ctrl Pts',(0.722228917460009,1.05303547481514,2.0340190544966));
#20516=CARTESIAN_POINT('Ctrl Pts',(0.726095080681017,1.01182045619333,2.03140220415071));
#20517=CARTESIAN_POINT('Ctrl Pts',(0.729961243902025,0.970605437571516,
2.02878535380482));
#20518=CARTESIAN_POINT('Ctrl Pts',(0.711668031650661,0.927329354706896,
2.02616850345893));
#20519=CARTESIAN_POINT('Ctrl Pts',(0.679417475504429,0.901356588462624,
2.02355165311304));
#20520=CARTESIAN_POINT('Ctrl Pts',(0.647166919358198,0.875383822218351,
2.02093480276714));
#20521=CARTESIAN_POINT('Ctrl Pts',(0.600959019317099,0.866714372594425,
2.01831795242125));
#20522=CARTESIAN_POINT('Ctrl Pts',(0.561514908627169,0.879318620323889,
2.01570110207536));
#20523=CARTESIAN_POINT('Ctrl Pts',(0.522070797937238,0.891922868053354,
2.01308425172946));
#20524=CARTESIAN_POINT('Ctrl Pts',(0.489390476598475,0.925800813136209,
2.01046740138357));
#20525=CARTESIAN_POINT('Ctrl Pts',(0.47813574698779,0.965573631142046,2.00785055103768));
#20526=CARTESIAN_POINT('Ctrl Pts',(0.474992502439002,0.976681467377235,
2.00711971157114));
#20527=CARTESIAN_POINT('Ctrl Pts',(0.473520421751905,0.988249094815541,
2.0063888721046));
#20528=CARTESIAN_POINT('Ctrl Pts',(0.473622351265484,0.999839631194249,
2.00565803263806));
#20529=CARTESIAN_POINT('Ctrl Pts',(0.473748222256554,0.999995809921948,
2.01934196736194));
#20530=CARTESIAN_POINT('Ctrl Pts',(0.473735293486444,0.979624254554346,
2.02061916163845));
#20531=CARTESIAN_POINT('Ctrl Pts',(0.478391980488661,0.959256875893503,
2.02189635591496));
#20532=CARTESIAN_POINT('Ctrl Pts',(0.487748897958052,0.941346462457022,
2.02317355019146));
#20533=CARTESIAN_POINT('Ctrl Pts',(0.5069203373911,0.904649718305799,2.02579040053735));
#20534=CARTESIAN_POINT('Ctrl Pts',(0.545823408464101,0.878267347693885,
2.02840725088324));
#20535=CARTESIAN_POINT('Ctrl Pts',(0.587007341569528,0.874020924816605,
2.03102410122914));
#20536=CARTESIAN_POINT('Ctrl Pts',(0.628191274674955,0.869774501939324,
2.03364095157503));
#20537=CARTESIAN_POINT('Ctrl Pts',(0.671656069812808,0.887664026796678,
2.03625780192092));
#20538=CARTESIAN_POINT('Ctrl Pts',(0.697914735578316,0.919671996193035,
2.03887465226682));
#20539=CARTESIAN_POINT('Ctrl Pts',(0.724173401343824,0.951679965589392,
2.04149150261271));
#20540=CARTESIAN_POINT('Ctrl Pts',(0.733225937736988,0.997806379524751,
2.0441083529586));
#20541=CARTESIAN_POINT('Ctrl Pts',(0.72101148240133,1.03736538090912,2.04672520330449));
#20542=CARTESIAN_POINT('Ctrl Pts',(0.708797027065672,1.07692438229349,2.04934205365039));
#20543=CARTESIAN_POINT('Ctrl Pts',(0.675315580001192,1.10991597112687,2.05195890399628));
#20544=CARTESIAN_POINT('Ctrl Pts',(0.635581432895856,1.12154745886576,2.05457575434217));
#20545=CARTESIAN_POINT('Ctrl Pts',(0.59584728579052,1.13317894660465,2.05719260468807));
#20546=CARTESIAN_POINT('Ctrl Pts',(0.549860438644329,1.12345033324905,2.05980945503396));
#20547=CARTESIAN_POINT('Ctrl Pts',(0.518241526751132,1.09672346863534,2.06242630537985));
#20548=CARTESIAN_POINT('Ctrl Pts',(0.490387977892526,1.07317939375162,2.06473152604054));
#20549=CARTESIAN_POINT('Ctrl Pts',(0.473684088301786,1.03644450847376,2.06703674670124));
#20550=CARTESIAN_POINT('Ctrl Pts',(0.473418004372097,0.999922226677399,
2.06934196736194));
#20551=CARTESIAN_POINT('Origin',(0.6,1.,2.15));
#20552=CARTESIAN_POINT('',(0.473569322058917,1.00010891293128,2.11934196736194));
#20553=CARTESIAN_POINT('',(0.473740555540666,1.00002674768131,2.10565803263806));
#20554=CARTESIAN_POINT('',(0.47355,1.,2.15));
#20555=CARTESIAN_POINT('Ctrl Pts',(0.473740555540666,1.00002674768131,2.10565803263806));
#20556=CARTESIAN_POINT('Ctrl Pts',(0.473703568953707,1.01916777914625,2.10445774292198));
#20557=CARTESIAN_POINT('Ctrl Pts',(0.477794964495735,1.03829380542625,2.10325745320589));
#20558=CARTESIAN_POINT('Ctrl Pts',(0.486097635636878,1.0553725521712,2.10205716348981));
#20559=CARTESIAN_POINT('Ctrl Pts',(0.504198971969625,1.09260733284801,2.09944031314392));
#20560=CARTESIAN_POINT('Ctrl Pts',(0.542317321105284,1.12011099531618,2.09682346279803));
#20561=CARTESIAN_POINT('Ctrl Pts',(0.583359964347627,1.12555066422426,2.09420661245214));
#20562=CARTESIAN_POINT('Ctrl Pts',(0.62440260758997,1.13099033313234,2.09158976210624));
#20563=CARTESIAN_POINT('Ctrl Pts',(0.668369544938998,1.11436600848032,2.08897291176035));
#20564=CARTESIAN_POINT('Ctrl Pts',(0.695545474812698,1.08313205071709,2.08635606141446));
#20565=CARTESIAN_POINT('Ctrl Pts',(0.722721404686398,1.05189809295385,2.08373921106856));
#20566=CARTESIAN_POINT('Ctrl Pts',(0.733106327084771,1.00605450207939,2.08112236072267));
#20567=CARTESIAN_POINT('Ctrl Pts',(0.722043527705466,0.966158451314527,
2.07850551037678));
#20568=CARTESIAN_POINT('Ctrl Pts',(0.71098072832616,0.926262400549665,2.07588866003089));
#20569=CARTESIAN_POINT('Ctrl Pts',(0.678470207169174,0.892313889894401,
2.073271809685));
#20570=CARTESIAN_POINT('Ctrl Pts',(0.639090051974211,0.87953512362367,2.0706549593391));
#20571=CARTESIAN_POINT('Ctrl Pts',(0.599709896779248,0.86675635735294,2.06803810899321));
#20572=CARTESIAN_POINT('Ctrl Pts',(0.553460107546307,0.875147335466744,
2.06542125864732));
#20573=CARTESIAN_POINT('Ctrl Pts',(0.52107967173656,0.900946841310449,2.06280440830142));
#20574=CARTESIAN_POINT('Ctrl Pts',(0.491603682429651,0.924432194096951,
2.0604222830803));
#20575=CARTESIAN_POINT('Ctrl Pts',(0.473620539892396,0.962343132242784,
2.05804015785918));
#20576=CARTESIAN_POINT('Ctrl Pts',(0.473391518308752,1.00006258785156,2.05565803263806));
#20577=CARTESIAN_POINT('Ctrl Pts',(0.473418004372097,0.999922226677399,
2.06934196736194));
#20578=CARTESIAN_POINT('Ctrl Pts',(0.473382033997262,0.994984986883897,
2.06965359704714));
#20579=CARTESIAN_POINT('Ctrl Pts',(0.473646461235087,0.990051632376521,
2.06996522673233));
#20580=CARTESIAN_POINT('Ctrl Pts',(0.474224350273596,0.985155275839,2.07027685641753));
#20581=CARTESIAN_POINT('Ctrl Pts',(0.47907706232946,0.944039063528183,2.07289370676342));
#20582=CARTESIAN_POINT('Ctrl Pts',(0.50603346308139,0.905531754778367,2.07551055710931));
#20583=CARTESIAN_POINT('Ctrl Pts',(0.543005874916624,0.886900335416373,
2.0781274074552));
#20584=CARTESIAN_POINT('Ctrl Pts',(0.579978286751859,0.868268916054378,
2.0807442578011));
#20585=CARTESIAN_POINT('Ctrl Pts',(0.626966709670398,0.869513386080205,
2.08336110814699));
#20586=CARTESIAN_POINT('Ctrl Pts',(0.662901030784248,0.890075786233013,
2.08597795849288));
#20587=CARTESIAN_POINT('Ctrl Pts',(0.698835351898097,0.910638186385821,
2.08859480883878));
#20588=CARTESIAN_POINT('Ctrl Pts',(0.723715571207256,0.95051851666561,2.09121165918467));
#20589=CARTESIAN_POINT('Ctrl Pts',(0.726385074899299,0.991833924307951,
2.09382850953056));
#20590=CARTESIAN_POINT('Ctrl Pts',(0.729054578591342,1.03314933195029,2.09644535987645));
#20591=CARTESIAN_POINT('Ctrl Pts',(0.709513366666269,1.07589981695519,2.09906221022235));
#20592=CARTESIAN_POINT('Ctrl Pts',(0.676523964943026,1.10091557332887,2.10167906056824));
#20593=CARTESIAN_POINT('Ctrl Pts',(0.643534563219784,1.12593132970255,2.10429591091413));
#20594=CARTESIAN_POINT('Ctrl Pts',(0.597096971698373,1.13321235744502,2.10691276126002));
#20595=CARTESIAN_POINT('Ctrl Pts',(0.558034351233094,1.1194937471697,2.10952961160592));
#20596=CARTESIAN_POINT('Ctrl Pts',(0.518971730767816,1.10577513689439,2.11214646195181));
#20597=CARTESIAN_POINT('Ctrl Pts',(0.48728408135867,1.0710568886013,2.1147633122977));
#20598=CARTESIAN_POINT('Ctrl Pts',(0.477180525319141,1.0309070826023,2.11738016264359));
#20599=CARTESIAN_POINT('Ctrl Pts',(0.474655708422174,1.02087389149615,2.11803409754971));
#20600=CARTESIAN_POINT('Ctrl Pts',(0.473478752433508,1.01050151615012,2.11868803245583));
#20601=CARTESIAN_POINT('Ctrl Pts',(0.473569322058917,1.00010891293128,2.11934196736194));
#20602=CARTESIAN_POINT('Origin',(0.6,1.,2.15));
#20603=CARTESIAN_POINT('',(0.473701319324768,0.999928563934628,2.16934196736194));
#20604=CARTESIAN_POINT('',(0.473475969746711,0.999901036847401,2.15565803263806));
#20605=CARTESIAN_POINT('',(0.47355,1.,2.15));
#20606=CARTESIAN_POINT('Ctrl Pts',(0.473475969746711,0.999901036847401,
2.15565803263806));
#20607=CARTESIAN_POINT('Ctrl Pts',(0.473771376261924,1.03425627771038,2.15349217833067));
#20608=CARTESIAN_POINT('Ctrl Pts',(0.488302943448428,1.0688317671636,2.15132632402327));
#20609=CARTESIAN_POINT('Ctrl Pts',(0.513274800541643,1.09229629753053,2.14916046971588));
#20610=CARTESIAN_POINT('Ctrl Pts',(0.543446549698046,1.12064684917997,2.14654361936999));
#20611=CARTESIAN_POINT('Ctrl Pts',(0.588859242361366,1.13277740107318,2.1439267690241));
#20612=CARTESIAN_POINT('Ctrl Pts',(0.629149287366476,1.12324847117969,2.1413099186782));
#20613=CARTESIAN_POINT('Ctrl Pts',(0.669439332371586,1.11371954128621,2.13869306833231));
#20614=CARTESIAN_POINT('Ctrl Pts',(0.704606729718486,1.08253112960603,2.13607621798642));
#20615=CARTESIAN_POINT('Ctrl Pts',(0.718882000334445,1.04366848746118,2.13345936764053));
#20616=CARTESIAN_POINT('Ctrl Pts',(0.733157270950405,1.00480584531632,2.13084251729463));
#20617=CARTESIAN_POINT('Ctrl Pts',(0.726540414835423,0.958268972706794,
2.12822566694874));
#20618=CARTESIAN_POINT('Ctrl Pts',(0.701998509069979,0.924925562785253,
2.12560881660285));
#20619=CARTESIAN_POINT('Ctrl Pts',(0.677456603304535,0.891582152863712,
2.12299196625696));
#20620=CARTESIAN_POINT('Ctrl Pts',(0.634989647888627,0.871432205630162,
2.12037511591106));
#20621=CARTESIAN_POINT('Ctrl Pts',(0.59364033014263,0.873511184567866,2.11775826556517));
#20622=CARTESIAN_POINT('Ctrl Pts',(0.552291012396633,0.87559016350557,2.11514141521928));
#20623=CARTESIAN_POINT('Ctrl Pts',(0.512059332320547,0.899898068614528,
2.11252456487339));
#20624=CARTESIAN_POINT('Ctrl Pts',(0.490985654047422,0.935534970611733,
2.10990771452749));
#20625=CARTESIAN_POINT('Ctrl Pts',(0.479577992537903,0.954826036459998,
2.10849115389768));
#20626=CARTESIAN_POINT('Ctrl Pts',(0.473784206454455,0.977436841907783,
2.10707459326787));
#20627=CARTESIAN_POINT('Ctrl Pts',(0.473740555540666,1.00002674768131,2.10565803263806));
#20628=CARTESIAN_POINT('Ctrl Pts',(0.473569322058917,1.00010891293128,2.11934196736194));
#20629=CARTESIAN_POINT('Ctrl Pts',(0.473841184769449,0.968913451231703,
2.12130488280172));
#20630=CARTESIAN_POINT('Ctrl Pts',(0.485533699168036,0.937535732473691,
2.1232677982415));
#20631=CARTESIAN_POINT('Ctrl Pts',(0.506474126044697,0.914602214201428,
2.12523071368127));
#20632=CARTESIAN_POINT('Ctrl Pts',(0.534390745479694,0.884028515504489,
2.12784756402717));
#20633=CARTESIAN_POINT('Ctrl Pts',(0.578743447019601,0.868462481815532,
2.13046441437306));
#20634=CARTESIAN_POINT('Ctrl Pts',(0.619643953027205,0.874884108988649,
2.13308126471895));
#20635=CARTESIAN_POINT('Ctrl Pts',(0.660544459034809,0.881305736161766,
2.13569811506484));
#20636=CARTESIAN_POINT('Ctrl Pts',(0.697992769510109,0.909715024196956,
2.13831496541074));
#20637=CARTESIAN_POINT('Ctrl Pts',(0.715196616413391,0.947372909972802,
2.14093181575663));
#20638=CARTESIAN_POINT('Ctrl Pts',(0.732400463316672,0.985030795748647,
2.14354866610252));
#20639=CARTESIAN_POINT('Ctrl Pts',(0.729359846647935,1.03193727926515,2.14616551644841));
#20640=CARTESIAN_POINT('Ctrl Pts',(0.707438215309595,1.0670589360858,2.14878236679431));
#20641=CARTESIAN_POINT('Ctrl Pts',(0.685516583971256,1.10218059290645,2.1513992171402));
#20642=CARTESIAN_POINT('Ctrl Pts',(0.644713937963314,1.12551742303125,2.15401606748609));
#20643=CARTESIAN_POINT('Ctrl Pts',(0.603326668644815,1.12660491425775,2.15663291783199));
#20644=CARTESIAN_POINT('Ctrl Pts',(0.561939399326316,1.12769240548424,2.15924976817788));
#20645=CARTESIAN_POINT('Ctrl Pts',(0.51996750669726,1.10653055781244,2.16186661852377));
#20646=CARTESIAN_POINT('Ctrl Pts',(0.496231686388225,1.07260859537424,2.16448346886966));
#20647=CARTESIAN_POINT('Ctrl Pts',(0.481542214702607,1.05161518961582,2.16610296836709));
#20648=CARTESIAN_POINT('Ctrl Pts',(0.473837240540682,1.02573460264732,2.16772246786452));
#20649=CARTESIAN_POINT('Ctrl Pts',(0.473701319324768,0.999928563934628,
2.16934196736194));
#20650=CARTESIAN_POINT('Origin',(0.6,1.,2.15));
#20651=CARTESIAN_POINT('',(0.473352235667534,0.999991049382066,2.21934196736194));
#20652=CARTESIAN_POINT('',(0.473504867419963,1.00010483506638,2.20565803263806));
#20653=CARTESIAN_POINT('',(0.47355,1.,2.15));
#20654=CARTESIAN_POINT('Ctrl Pts',(0.473504867419963,1.00010483506638,2.20565803263806));
#20655=CARTESIAN_POINT('Ctrl Pts',(0.473432601452696,1.00827186028206,2.20514346408525));
#20656=CARTESIAN_POINT('Ctrl Pts',(0.474157534286366,1.01642611923938,2.20462889553244));
#20657=CARTESIAN_POINT('Ctrl Pts',(0.475726914006531,1.02441447959464,2.20411432697963));
#20658=CARTESIAN_POINT('Ctrl Pts',(0.48370803108242,1.0650394720171,2.20149747663373));
#20659=CARTESIAN_POINT('Ctrl Pts',(0.513528695332623,1.10137390406913,2.19888062628784));
#20660=CARTESIAN_POINT('Ctrl Pts',(0.551816966436341,1.11712498450026,2.19626377594195));
#20661=CARTESIAN_POINT('Ctrl Pts',(0.59010523754006,1.1328760649314,2.19364692559606));
#20662=CARTESIAN_POINT('Ctrl Pts',(0.636861115497294,1.12804379374164,2.19103007525016));
#20663=CARTESIAN_POINT('Ctrl Pts',(0.671118708852879,1.10479501880275,2.18841322490427));
#20664=CARTESIAN_POINT('Ctrl Pts',(0.705376302208464,1.08154624386386,2.18579637455838));
#20665=CARTESIAN_POINT('Ctrl Pts',(0.7271356109624,1.03988096517584,2.18317952421248));
#20666=CARTESIAN_POINT('Ctrl Pts',(0.726639502419725,0.998482388913484,
2.18056267386659));
#20667=CARTESIAN_POINT('Ctrl Pts',(0.726143393877049,0.95708381265113,2.1779458235207));
#20668=CARTESIAN_POINT('Ctrl Pts',(0.703391868037763,0.915951938814441,
2.17532897317481));
#20669=CARTESIAN_POINT('Ctrl Pts',(0.668586979533722,0.893530788668923,
2.17271212282892));
#20670=CARTESIAN_POINT('Ctrl Pts',(0.63378209102968,0.871109638523405,2.17009527248302));
#20671=CARTESIAN_POINT('Ctrl Pts',(0.586923839860883,0.867399212069058,
2.16747842213713));
#20672=CARTESIAN_POINT('Ctrl Pts',(0.549024022842182,0.88406330841772,2.16486157179124));
#20673=CARTESIAN_POINT('Ctrl Pts',(0.511124205823482,0.900727404766382,
2.16224472144534));
#20674=CARTESIAN_POINT('Ctrl Pts',(0.482182822954877,0.937766023918054,
2.15962787109945));
#20675=CARTESIAN_POINT('Ctrl Pts',(0.475177534345317,0.978570609196729,
2.15701102075356));
#20676=CARTESIAN_POINT('Ctrl Pts',(0.473970221356853,0.985602996945691,
2.15656002471506));
#20677=CARTESIAN_POINT('Ctrl Pts',(0.473414457221305,0.992747241932372,
2.15610902867656));
#20678=CARTESIAN_POINT('Ctrl Pts',(0.473475969746711,0.999901036847401,
2.15565803263806));
#20679=CARTESIAN_POINT('Ctrl Pts',(0.473701319324768,0.999928563934628,
2.16934196736194));
#20680=CARTESIAN_POINT('Ctrl Pts',(0.473617613747686,0.984036200493609,
2.17033931821041));
#20681=CARTESIAN_POINT('Ctrl Pts',(0.476404528994482,0.968172110044866,
2.17133666905888));
#20682=CARTESIAN_POINT('Ctrl Pts',(0.482198594761734,0.953495162034513,
2.17233401990734));
#20683=CARTESIAN_POINT('Ctrl Pts',(0.497401071433289,0.914985768337587,
2.17495087025323));
#20684=CARTESIAN_POINT('Ctrl Pts',(0.533305772765409,0.884649058148337,
2.17756772059913));
#20685=CARTESIAN_POINT('Ctrl Pts',(0.573812603904437,0.876088372947374,
2.18018457094502));
#20686=CARTESIAN_POINT('Ctrl Pts',(0.614319435043466,0.86752768774641,2.18280142129091));
#20687=CARTESIAN_POINT('Ctrl Pts',(0.659428395989404,0.880743027533735,
2.1854182716368));
#20688=CARTESIAN_POINT('Ctrl Pts',(0.688912092443748,0.909808476845009,
2.1880351219827));
#20689=CARTESIAN_POINT('Ctrl Pts',(0.718395788898092,0.938873926156282,
2.19065197232859));
#20690=CARTESIAN_POINT('Ctrl Pts',(0.732254220860843,0.983789484991505,
2.19326882267448));
#20691=CARTESIAN_POINT('Ctrl Pts',(0.724273102711297,1.02441448287903,2.19588567302037));
#20692=CARTESIAN_POINT('Ctrl Pts',(0.716291984561752,1.06503948076655,2.19850252336627));
#20693=CARTESIAN_POINT('Ctrl Pts',(0.686471316299909,1.10137391770637,2.20111937371216));
#20694=CARTESIAN_POINT('Ctrl Pts',(0.648183040045466,1.11712500025644,2.20373622405805));
#20695=CARTESIAN_POINT('Ctrl Pts',(0.609894763791023,1.13287608280652,2.20635307440395));
#20696=CARTESIAN_POINT('Ctrl Pts',(0.563138879543981,1.12804381096685,2.20896992474984));
#20697=CARTESIAN_POINT('Ctrl Pts',(0.528881281579892,1.10479503290036,2.21158677509573));
#20698=CARTESIAN_POINT('Ctrl Pts',(0.49503980248944,1.0818286521973,2.21417183918447));
#20699=CARTESIAN_POINT('Ctrl Pts',(0.473394826320348,1.04089044984514,2.2167569032732));
#20700=CARTESIAN_POINT('Ctrl Pts',(0.473352235667534,0.999991049382066,
2.21934196736194));
#20701=CARTESIAN_POINT('Origin',(0.6,1.,2.15));
#20702=CARTESIAN_POINT('',(0.473682079464411,1.00008273769678,2.26934196736194));
#20703=CARTESIAN_POINT('',(0.473732170341016,0.999958186567598,2.25565803263806));
#20704=CARTESIAN_POINT('',(0.47355,1.,2.15));
#20705=CARTESIAN_POINT('Ctrl Pts',(0.473732170341016,0.999958186567598,
2.25565803263806));
#20706=CARTESIAN_POINT('Ctrl Pts',(0.47380378639699,1.0235579489136,2.25417789949394));
#20707=CARTESIAN_POINT('Ctrl Pts',(0.480162569358453,1.04719354904427,2.25269776634982));
#20708=CARTESIAN_POINT('Ctrl Pts',(0.492561799143745,1.06705892706426,2.25121763320569));
#20709=CARTESIAN_POINT('Ctrl Pts',(0.514483427533268,1.1021805791598,2.2486007828598));
#20710=CARTESIAN_POINT('Ctrl Pts',(0.555286068051798,1.12551740614607,2.24598393251391));
#20711=CARTESIAN_POINT('Ctrl Pts',(0.596673331802579,1.12660489722647,2.24336708216802));
#20712=CARTESIAN_POINT('Ctrl Pts',(0.63806059555336,1.12769238830687,2.24075023182212));
#20713=CARTESIAN_POINT('Ctrl Pts',(0.680032482536391,1.10653054348142,2.23813338147623));
#20714=CARTESIAN_POINT('Ctrl Pts',(0.703768299652422,1.07260858560646,2.23551653113034));
#20715=CARTESIAN_POINT('Ctrl Pts',(0.727504116768454,1.0386866277315,2.23289968078445));
#20716=CARTESIAN_POINT('Ctrl Pts',(0.733003864017485,0.992004556807043,
2.23028283043855));
#20717=CARTESIAN_POINT('Ctrl Pts',(0.717801389391014,0.953495168290641,
2.22766598009266));
#20718=CARTESIAN_POINT('Ctrl Pts',(0.702598914764542,0.914985779774238,
2.22504912974677));
#20719=CARTESIAN_POINT('Ctrl Pts',(0.666694218262566,0.884649073665893,
2.22243227940087));
#20720=CARTESIAN_POINT('Ctrl Pts',(0.626187392572728,0.876088389616529,
2.21981542905498));
#20721=CARTESIAN_POINT('Ctrl Pts',(0.58568056688289,0.867527705567165,2.21719857870909));
#20722=CARTESIAN_POINT('Ctrl Pts',(0.540571612005191,0.880743043576783,
2.2145817283632));
#20723=CARTESIAN_POINT('Ctrl Pts',(0.511087919517129,0.909808488978038,
2.21196487801731));
#20724=CARTESIAN_POINT('Ctrl Pts',(0.487401800053794,0.933158604039368,
2.20986259622422));
#20725=CARTESIAN_POINT('Ctrl Pts',(0.473800111710378,0.966738263555599,
2.20776031443114));
#20726=CARTESIAN_POINT('Ctrl Pts',(0.473504867419963,1.00010483506638,2.20565803263806));
#20727=CARTESIAN_POINT('Ctrl Pts',(0.473352235667534,0.999991049382066,
2.21934196736194));
#20728=CARTESIAN_POINT('Ctrl Pts',(0.473351711967774,0.99948814546325,2.2193737536191));
#20729=CARTESIAN_POINT('Ctrl Pts',(0.473354454431116,0.998985247411069,
2.21940553987625));
#20730=CARTESIAN_POINT('Ctrl Pts',(0.473360480544096,0.998482388709186,
2.21943732613341));
#20731=CARTESIAN_POINT('Ctrl Pts',(0.473856589153524,0.95708380687781,2.2220541764793));
#20732=CARTESIAN_POINT('Ctrl Pts',(0.496608118053516,0.915951927508368,
2.22467102682519));
#20733=CARTESIAN_POINT('Ctrl Pts',(0.531413011239654,0.893530774346426,
2.22728787717109));
#20734=CARTESIAN_POINT('Ctrl Pts',(0.566217904425792,0.871109621184485,
2.22990472751698));
#20735=CARTESIAN_POINT('Ctrl Pts',(0.613076161898077,0.867399194230046,
2.23252157786287));
#20736=CARTESIAN_POINT('Ctrl Pts',(0.650975984015301,0.88406329282086,2.23513842820876));
#20737=CARTESIAN_POINT('Ctrl Pts',(0.688875806132525,0.900727391411673,
2.23775527855466));
#20738=CARTESIAN_POINT('Ctrl Pts',(0.717817192894688,0.93776601554774,2.24037212890055));
#20739=CARTESIAN_POINT('Ctrl Pts',(0.724822482446523,0.978570606314872,
2.24298897924644));
#20740=CARTESIAN_POINT('Ctrl Pts',(0.731827771998358,1.019375197082,2.24560582959233));
#20741=CARTESIAN_POINT('Ctrl Pts',(0.716896964339864,1.0639457544802,2.24822267993823));
#20742=CARTESIAN_POINT('Ctrl Pts',(0.686725211124828,1.09229630994494,2.25083953028412));
#20743=CARTESIAN_POINT('Ctrl Pts',(0.656553457909791,1.12064686540969,2.25345638063001));
#20744=CARTESIAN_POINT('Ctrl Pts',(0.611140759138212,1.13277741894098,2.25607323097591));
#20745=CARTESIAN_POINT('Ctrl Pts',(0.570850708712658,1.12324848776292,2.2586900813218));
#20746=CARTESIAN_POINT('Ctrl Pts',(0.530560658287105,1.11371955658487,2.26130693166769));
#20747=CARTESIAN_POINT('Ctrl Pts',(0.495393256207577,1.08253114069748,2.26392378201358));
#20748=CARTESIAN_POINT('Ctrl Pts',(0.481117983672093,1.04366849332961,2.26654063235948));
#20749=CARTESIAN_POINT('Ctrl Pts',(0.476024096576591,1.02980102162761,2.26747441069363));
#20750=CARTESIAN_POINT('Ctrl Pts',(0.473590398662461,1.01495639211521,2.26840818902779));
#20751=CARTESIAN_POINT('Ctrl Pts',(0.473682079464411,1.00008273769678,2.26934196736194));
#20752=CARTESIAN_POINT('Origin',(0.6,1.,2.15));
#20753=CARTESIAN_POINT('',(0.473597863174539,0.999893075682974,2.31934196736194));
#20754=CARTESIAN_POINT('',(0.473373733146151,0.999953562449677,2.30565803263806));
#20755=CARTESIAN_POINT('',(0.47355,1.,2.15));
#20756=CARTESIAN_POINT('Ctrl Pts',(0.473373733146151,0.999953562449677,
2.30565803263806));
#20757=CARTESIAN_POINT('Ctrl Pts',(0.473559114374899,1.03866557284283,2.30321233490263));
#20758=CARTESIAN_POINT('Ctrl Pts',(0.492644288253083,1.07753593829701,2.3007666371672));
#20759=CARTESIAN_POINT('Ctrl Pts',(0.523476045360312,1.10091555973398,2.29832093943176));
#20760=CARTESIAN_POINT('Ctrl Pts',(0.556465442652399,1.12593131272659,2.29570408908587));
#20761=CARTESIAN_POINT('Ctrl Pts',(0.602903027909946,1.1332123395264,2.29308723873998));
#20762=CARTESIAN_POINT('Ctrl Pts',(0.641965643116553,1.11949373110512,2.29047038839408));
#20763=CARTESIAN_POINT('Ctrl Pts',(0.681028258323161,1.10577512268384,2.28785353804819));
#20764=CARTESIAN_POINT('Ctrl Pts',(0.712715903478828,1.07105687904148,2.2852366877023));
#20765=CARTESIAN_POINT('Ctrl Pts',(0.722819458161278,1.03090707843903,2.28261983735641));
#20766=CARTESIAN_POINT('Ctrl Pts',(0.732923012843728,0.990757277836576,
2.28000298701051));
#20767=CARTESIAN_POINT('Ctrl Pts',(0.72144247705296,0.945175920274039,2.27738613666462));
#20768=CARTESIAN_POINT('Ctrl Pts',(0.693525861372284,0.914602225692484,
2.27476928631873));
#20769=CARTESIAN_POINT('Ctrl Pts',(0.665609245691608,0.88402853111093,2.27215243597284));
#20770=CARTESIAN_POINT('Ctrl Pts',(0.621256550121025,0.868462499510358,
2.26953558562694));
#20771=CARTESIAN_POINT('Ctrl Pts',(0.580356049616192,0.874884125818288,
2.26691873528105));
#20772=CARTESIAN_POINT('Ctrl Pts',(0.539455549111359,0.881305752126219,
2.26430188493516));
#20773=CARTESIAN_POINT('Ctrl Pts',(0.502007243672275,0.909715036342652,
2.26168503458927));
#20774=CARTESIAN_POINT('Ctrl Pts',(0.484803399082991,0.947372917053277,
2.25906818424337));
#20775=CARTESIAN_POINT('Ctrl Pts',(0.477330328981013,0.963730887562828,
2.2579314670416));
#20776=CARTESIAN_POINT('Ctrl Pts',(0.473677170422209,0.981833968538321,
2.25679474983983));
#20777=CARTESIAN_POINT('Ctrl Pts',(0.473732170341016,0.999958186567598,
2.25565803263806));
#20778=CARTESIAN_POINT('Ctrl Pts',(0.473682079464411,1.00008273769678,2.26934196736194));
#20779=CARTESIAN_POINT('Ctrl Pts',(0.473847327881654,0.973273986038867,
2.27102503937368));
#20780=CARTESIAN_POINT('Ctrl Pts',(0.4822169290695,0.946370939387992,2.27270811138542));
#20781=CARTESIAN_POINT('Ctrl Pts',(0.498001477210419,0.924925552697152,
2.27439118339715));
#20782=CARTESIAN_POINT('Ctrl Pts',(0.522543386275672,0.891582138280912,
2.27700803374305));
#20783=CARTESIAN_POINT('Ctrl Pts',(0.565010347397619,0.871432188296782,
2.27962488408894));
#20784=CARTESIAN_POINT('Ctrl Pts',(0.606359670709474,0.873511167531032,
2.28224173443483));
#20785=CARTESIAN_POINT('Ctrl Pts',(0.64770899402133,0.875590146765282,2.28485858478073));
#20786=CARTESIAN_POINT('Ctrl Pts',(0.687940679523094,0.899898055217912,
2.28747543512662));
#20787=CARTESIAN_POINT('Ctrl Pts',(0.709014360624521,0.935534961978321,
2.29009228547251));
#20788=CARTESIAN_POINT('Ctrl Pts',(0.730088041725949,0.971171868738729,
2.2927091358184));
#20789=CARTESIAN_POINT('Ctrl Pts',(0.73200371842704,1.01813777380691,2.2953259861643));
#20790=CARTESIAN_POINT('Ctrl Pts',(0.713902379672349,1.05537255954882,2.29794283651019));
#20791=CARTESIAN_POINT('Ctrl Pts',(0.695801040917658,1.09260734529072,2.30055968685608));
#20792=CARTESIAN_POINT('Ctrl Pts',(0.657682686707185,1.12011101170634,2.30317653720197));
#20793=CARTESIAN_POINT('Ctrl Pts',(0.616640037917562,1.12555068124487,2.30579338754787));
#20794=CARTESIAN_POINT('Ctrl Pts',(0.57559738912794,1.1309903507834,2.30841023789376));
#20795=CARTESIAN_POINT('Ctrl Pts',(0.531630445759169,1.11436602344484,2.31102708823965));
#20796=CARTESIAN_POINT('Ctrl Pts',(0.504454512281174,1.08313206166147,2.31364393858554));
#20797=CARTESIAN_POINT('Ctrl Pts',(0.484729877635794,1.06046205898416,2.31554328151101));
#20798=CARTESIAN_POINT('Ctrl Pts',(0.473850812735054,1.03009564368688,2.31744262443648));
#20799=CARTESIAN_POINT('Ctrl Pts',(0.473597863174539,0.999893075682974,
2.31934196736194));
#20800=CARTESIAN_POINT('Origin',(0.6,1.,2.15));
#20801=CARTESIAN_POINT('',(0.473395817154925,1.00006080538999,2.36934196736194));
#20802=CARTESIAN_POINT('',(0.473630671680838,1.00010094048498,2.35565803263806));
#20803=CARTESIAN_POINT('',(0.47355,1.,2.15));
#20804=CARTESIAN_POINT('',(0.695811615272236,1.08252112989365,2.4));
#20805=CARTESIAN_POINT('Ctrl Pts',(0.473395817154925,1.00006080538999,2.36934196736194));
#20806=CARTESIAN_POINT('Ctrl Pts',(0.473632259557073,0.962556436040281,
2.37171076053695));
#20807=CARTESIAN_POINT('Ctrl Pts',(0.491389033274771,0.924867297705602,
2.37407955371196));
#20808=CARTESIAN_POINT('Ctrl Pts',(0.520582501482215,0.901356555443706,
2.37644834688697));
#20809=CARTESIAN_POINT('Ctrl Pts',(0.552833074551427,0.875383796542954,
2.37906519723286));
#20810=CARTESIAN_POINT('Ctrl Pts',(0.59904103097391,0.866714403531687,2.38168204757875));
#20811=CARTESIAN_POINT('Ctrl Pts',(0.638485120164714,0.879318631335514,
2.38429889792465));
#20812=CARTESIAN_POINT('Ctrl Pts',(0.677929209355517,0.891922859139342,
2.38691574827054));
#20813=CARTESIAN_POINT('Ctrl Pts',(0.710609431314642,0.925800707758264,
2.38953259861643));
#20814=CARTESIAN_POINT('Ctrl Pts',(0.721864159102138,0.965573527992604,
2.39214944896232));
#20815=CARTESIAN_POINT('Ctrl Pts',(0.733118886889633,1.00534634822694,2.39476629930821));
#20816=CARTESIAN_POINT('Ctrl Pts',(0.7229481205055,1.0510141400767,2.39738314965411));
#20817=CARTESIAN_POINT('Ctrl Pts',(0.695811615272236,1.08252112989365,2.4));
#20818=CARTESIAN_POINT('',(0.50401104110406,1.08263520219401,2.4));
#20819=CARTESIAN_POINT('Origin',(0.6,1.,2.4));
#20820=CARTESIAN_POINT('Ctrl Pts',(0.504010178078501,1.08263575731581,2.4));
#20821=CARTESIAN_POINT('Ctrl Pts',(0.529836321312633,1.11242104812743,2.3975091839613));
#20822=CARTESIAN_POINT('Ctrl Pts',(0.57074030629072,1.12936968375571,2.3950183679226));
#20823=CARTESIAN_POINT('Ctrl Pts',(0.610030393987409,1.12624202648756,2.3925275518839));
#20824=CARTESIAN_POINT('Ctrl Pts',(0.651308544594168,1.12295611099769,2.389910701538));
#20825=CARTESIAN_POINT('Ctrl Pts',(0.690805340696773,1.09751079590418,2.38729385119211));
#20826=CARTESIAN_POINT('Ctrl Pts',(0.710833835900798,1.0612825699207,2.38467700084622));
#20827=CARTESIAN_POINT('Ctrl Pts',(0.730862331104824,1.02505434393722,2.38206015050033));
#20828=CARTESIAN_POINT('Ctrl Pts',(0.73142252541027,0.978043207063774,2.37944330015443));
#20829=CARTESIAN_POINT('Ctrl Pts',(0.712251088485857,0.941346462423258,
2.37682644980854));
#20830=CARTESIAN_POINT('Ctrl Pts',(0.693079651561443,0.904649717782742,
2.37420959946265));
#20831=CARTESIAN_POINT('Ctrl Pts',(0.654176583407171,0.878267365375156,
2.37159274911676));
#20832=CARTESIAN_POINT('Ctrl Pts',(0.612992655582392,0.874020946237636,
2.36897589877086));
#20833=CARTESIAN_POINT('Ctrl Pts',(0.571808727757614,0.869774527100117,
2.36635904842497));
#20834=CARTESIAN_POINT('Ctrl Pts',(0.52834394026233,0.887664041232664,2.36374219807908));
#20835=CARTESIAN_POINT('Ctrl Pts',(0.502085278312862,0.919672004499943,
2.36112534773319));
#20836=CARTESIAN_POINT('Ctrl Pts',(0.483798106092066,0.941963130294246,
2.35930290936814));
#20837=CARTESIAN_POINT('Ctrl Pts',(0.473856023642611,0.971101801466951,
2.3574804710031));
#20838=CARTESIAN_POINT('Ctrl Pts',(0.473630671680838,1.00010094048498,2.35565803263806));
#20839=CARTESIAN_POINT('Origin',(-0.6,1.,2.15));
#20840=CARTESIAN_POINT('',(-0.726251764241557,0.999995816438242,2.01934196736194));
#20841=CARTESIAN_POINT('',(-0.726377624507173,0.999839605165841,2.00565803263806));
#20842=CARTESIAN_POINT('',(-0.72645,1.,2.15));
#20843=CARTESIAN_POINT('',(-0.695811615272238,1.08252112989365,2.));
#20844=CARTESIAN_POINT('Ctrl Pts',(-0.726377624507173,0.999839605165841,
2.00565803263806));
#20845=CARTESIAN_POINT('Ctrl Pts',(-0.726114592834244,1.02975025674996,
2.00377202175871));
#20846=CARTESIAN_POINT('Ctrl Pts',(-0.715369380269338,1.05981347843636,
2.00188601087935));
#20847=CARTESIAN_POINT('Ctrl Pts',(-0.695811615272238,1.08252112989365,
2.));
#20848=CARTESIAN_POINT('',(-0.504011038081522,1.08263519664064,2.));
#20849=CARTESIAN_POINT('Origin',(-0.6,1.,2.));
#20850=CARTESIAN_POINT('Ctrl Pts',(-0.504010174669748,1.08263575197435,
2.));
#20851=CARTESIAN_POINT('Ctrl Pts',(-0.529836317100857,1.11242103949754,
2.0024908160387));
#20852=CARTESIAN_POINT('Ctrl Pts',(-0.570740304630068,1.12936968846467,
2.0049816320774));
#20853=CARTESIAN_POINT('Ctrl Pts',(-0.610030394063595,1.12624203395227,
2.0074724481161));
#20854=CARTESIAN_POINT('Ctrl Pts',(-0.651308546495077,1.12295612135759,
2.010089298462));
#20855=CARTESIAN_POINT('Ctrl Pts',(-0.690805343523631,1.09751079747805,
2.01270614880789));
#20856=CARTESIAN_POINT('Ctrl Pts',(-0.710833838996196,1.06128256888394,
2.01532299915378));
#20857=CARTESIAN_POINT('Ctrl Pts',(-0.721087117546352,1.04273608746385,
2.01666265522317));
#20858=CARTESIAN_POINT('Ctrl Pts',(-0.72623820261666,1.02136365505003,2.01800231129255));
#20859=CARTESIAN_POINT('Ctrl Pts',(-0.726251764241557,0.999995816438242,
2.01934196736194));
#20860=CARTESIAN_POINT('Origin',(-0.6,1.,2.15));
#20861=CARTESIAN_POINT('',(-0.7265819818033,0.99992222657182,2.06934196736194));
#20862=CARTESIAN_POINT('',(-0.726608486751216,1.0000625869776,2.05565803263806));
#20863=CARTESIAN_POINT('',(-0.72645,1.,2.15));
#20864=CARTESIAN_POINT('Ctrl Pts',(-0.726608486751216,1.0000625869776,2.05565803263806));
#20865=CARTESIAN_POINT('Ctrl Pts',(-0.726631053637245,1.00377931196893,
2.05542330751329));
#20866=CARTESIAN_POINT('Ctrl Pts',(-0.726481239616099,1.00749417780353,
2.05518858238852));
#20867=CARTESIAN_POINT('Ctrl Pts',(-0.726153054400444,1.01119320003794,
2.05495385726375));
#20868=CARTESIAN_POINT('Ctrl Pts',(-0.722494257346049,1.0524320219281,2.05233700691785));
#20869=CARTESIAN_POINT('Ctrl Pts',(-0.696665580577272,1.09170163174089,
2.04972015657196));
#20870=CARTESIAN_POINT('Ctrl Pts',(-0.660248783717448,1.1113984599152,2.04710330622607));
#20871=CARTESIAN_POINT('Ctrl Pts',(-0.623831986857623,1.13109528808951,
2.04448645588018));
#20872=CARTESIAN_POINT('Ctrl Pts',(-0.576827069906751,1.13121933462535,
2.04186960553428));
#20873=CARTESIAN_POINT('Ctrl Pts',(-0.540311843519016,1.11170438339395,
2.03925275518839));
#20874=CARTESIAN_POINT('Ctrl Pts',(-0.503796617131281,1.09218943216256,
2.0366359048425));
#20875=CARTESIAN_POINT('Ctrl Pts',(-0.477771081306684,1.05303548316395,
2.03401905449661));
#20876=CARTESIAN_POINT('Ctrl Pts',(-0.473904915961309,1.01182046061616,
2.03140220415071));
#20877=CARTESIAN_POINT('Ctrl Pts',(-0.470038750615934,0.970605438068375,
2.02878535380482));
#20878=CARTESIAN_POINT('Ctrl Pts',(-0.48833195574978,0.927329341971419,
2.02616850345893));
#20879=CARTESIAN_POINT('Ctrl Pts',(-0.520582517234745,0.901356578046236,
2.02355165311303));
#20880=CARTESIAN_POINT('Ctrl Pts',(-0.55283307871971,0.875383814121054,
2.02093480276714));
#20881=CARTESIAN_POINT('Ctrl Pts',(-0.599040996555793,0.866714382367644,
2.01831795242125));
#20882=CARTESIAN_POINT('Ctrl Pts',(-0.63848510046728,0.879318623815634,
2.01570110207536));
#20883=CARTESIAN_POINT('Ctrl Pts',(-0.677929204378768,0.891922865263625,
2.01308425172946));
#20884=CARTESIAN_POINT('Ctrl Pts',(-0.710609494365659,0.925800779913016,
2.01046740138357));
#20885=CARTESIAN_POINT('Ctrl Pts',(-0.721864223397342,0.965573598616285,
2.00785055103768));
#20886=CARTESIAN_POINT('Ctrl Pts',(-0.725007467784426,0.976681435046254,
2.00711971157114));
#20887=CARTESIAN_POINT('Ctrl Pts',(-0.726479550710055,0.988249065107503,
2.0063888721046));
#20888=CARTESIAN_POINT('Ctrl Pts',(-0.726377624507173,0.999839605165841,
2.00565803263806));
#20889=CARTESIAN_POINT('Ctrl Pts',(-0.726251764241557,0.999995816438242,
2.01934196736194));
#20890=CARTESIAN_POINT('Ctrl Pts',(-0.726264693552367,0.979624258543708,
2.02061916163845));
#20891=CARTESIAN_POINT('Ctrl Pts',(-0.721608007468156,0.959256876063438,
2.02189635591495));
#20892=CARTESIAN_POINT('Ctrl Pts',(-0.712251090996448,0.941346462433457,
2.02317355019146));
#20893=CARTESIAN_POINT('Ctrl Pts',(-0.693079653607559,0.904649717885772,
2.02579040053735));
#20894=CARTESIAN_POINT('Ctrl Pts',(-0.654176584913204,0.878267362099087,
2.02840725088324));
#20895=CARTESIAN_POINT('Ctrl Pts',(-0.612992656110291,0.874020942267452,
2.03102410122914));
#20896=CARTESIAN_POINT('Ctrl Pts',(-0.571808727307379,0.869774522435818,
2.03364095157503));
#20897=CARTESIAN_POINT('Ctrl Pts',(-0.528343938395909,0.887664038559235,
2.03625780192092));
#20898=CARTESIAN_POINT('Ctrl Pts',(-0.502085275739541,0.919672002962672,
2.03887465226682));
#20899=CARTESIAN_POINT('Ctrl Pts',(-0.475826613083173,0.951679967366109,
2.04149150261271));
#20900=CARTESIAN_POINT('Ctrl Pts',(-0.466774076681907,0.997806380049565,
2.0441083529586));
#20901=CARTESIAN_POINT('Ctrl Pts',(-0.478988530498336,1.03736537794115,
2.04672520330449));
#20902=CARTESIAN_POINT('Ctrl Pts',(-0.491202984314765,1.07692437583273,
2.04934205365039));
#20903=CARTESIAN_POINT('Ctrl Pts',(-0.52468442834889,1.10991595893243,2.05195890399628));
#20904=CARTESIAN_POINT('Ctrl Pts',(-0.564418571222927,1.12154744492272,
2.05457575434217));
#20905=CARTESIAN_POINT('Ctrl Pts',(-0.604152714096964,1.13317893091301,
2.05719260468806));
#20906=CARTESIAN_POINT('Ctrl Pts',(-0.650139555810913,1.12345031979389,
2.05980945503396));
#20907=CARTESIAN_POINT('Ctrl Pts',(-0.681758464159146,1.09672345837341,
2.06242630537985));
#20908=CARTESIAN_POINT('Ctrl Pts',(-0.709612009894941,1.07317938630266,
2.06473152604055));
#20909=CARTESIAN_POINT('Ctrl Pts',(-0.726315897827418,1.03644450458023,
2.06703674670125));
#20910=CARTESIAN_POINT('Ctrl Pts',(-0.7265819818033,0.99992222657182,2.06934196736194));
#20911=CARTESIAN_POINT('Origin',(-0.6,1.,2.15));
#20912=CARTESIAN_POINT('',(-0.726430664085926,1.00010891291408,2.11934196736194));
#20913=CARTESIAN_POINT('',(-0.726259449807842,1.00002674766465,2.10565803263806));
#20914=CARTESIAN_POINT('',(-0.72645,1.,2.15));
#20915=CARTESIAN_POINT('Ctrl Pts',(-0.726259449807842,1.00002674766465,
2.10565803263806));
#20916=CARTESIAN_POINT('Ctrl Pts',(-0.726296436394794,1.01916777993272,
2.10445774292198));
#20917=CARTESIAN_POINT('Ctrl Pts',(-0.722205040678573,1.0382938070189,2.1032574532059));
#20918=CARTESIAN_POINT('Ctrl Pts',(-0.713902369187372,1.05537255449598,
2.10205716348981));
#20919=CARTESIAN_POINT('Ctrl Pts',(-0.695801032091435,1.09260733676896,
2.09944031314392));
#20920=CARTESIAN_POINT('Ctrl Pts',(-0.657682681356665,1.12011100048129,
2.09682346279803));
#20921=CARTESIAN_POINT('Ctrl Pts',(-0.616640036366223,1.12555066958795,
2.09420661245214));
#20922=CARTESIAN_POINT('Ctrl Pts',(-0.57559739137578,1.13099033869461,2.09158976210624));
#20923=CARTESIAN_POINT('Ctrl Pts',(-0.531630452129665,1.1143660131956,2.08897291176035));
#20924=CARTESIAN_POINT('Ctrl Pts',(-0.504454521120231,1.08313205416568,
2.08635606141446));
#20925=CARTESIAN_POINT('Ctrl Pts',(-0.477278590110797,1.05189809513576,
2.08373921106857));
#20926=CARTESIAN_POINT('Ctrl Pts',(-0.466893667338043,1.00605450257494,
2.08112236072267));
#20927=CARTESIAN_POINT('Ctrl Pts',(-0.477956467154043,0.966158450016923,
2.07850551037678));
#20928=CARTESIAN_POINT('Ctrl Pts',(-0.489019266970043,0.926262397458909,
2.07588866003089));
#20929=CARTESIAN_POINT('Ctrl Pts',(-0.521529789374798,0.892313884903708,
2.07327180968499));
#20930=CARTESIAN_POINT('Ctrl Pts',(-0.560909946303062,0.879535118270141,
2.0706549593391));
#20931=CARTESIAN_POINT('Ctrl Pts',(-0.600290103231324,0.866756351636574,
2.06803810899321));
#20932=CARTESIAN_POINT('Ctrl Pts',(-0.646539894683095,0.875147330924641,
2.06542125864732));
#20933=CARTESIAN_POINT('Ctrl Pts',(-0.678920331738974,0.900946837552442,
2.06280440830142));
#20934=CARTESIAN_POINT('Ctrl Pts',(-0.708396322180238,0.924432191052708,
2.0604222830803));
#20935=CARTESIAN_POINT('Ctrl Pts',(-0.726379465045821,0.962343129588992,
2.05804015785918));
#20936=CARTESIAN_POINT('Ctrl Pts',(-0.726608486751216,1.0000625869776,2.05565803263806));
#20937=CARTESIAN_POINT('Ctrl Pts',(-0.7265819818033,0.99992222657182,2.06934196736194));
#20938=CARTESIAN_POINT('Ctrl Pts',(-0.726617952184381,0.99498498729039,
2.06965359704714));
#20939=CARTESIAN_POINT('Ctrl Pts',(-0.726353524983949,0.990051633299336,
2.06996522673233));
#20940=CARTESIAN_POINT('Ctrl Pts',(-0.725775636014574,0.985155277281126,
2.07027685641753));
#20941=CARTESIAN_POINT('Ctrl Pts',(-0.720922924539255,0.944039069331128,
2.07289370676342));
#20942=CARTESIAN_POINT('Ctrl Pts',(-0.693966526606102,0.905531765152948,
2.07551055710931));
#20943=CARTESIAN_POINT('Ctrl Pts',(-0.656994118794319,0.886900347913169,
2.0781274074552));
#20944=CARTESIAN_POINT('Ctrl Pts',(-0.620021710982536,0.868268930673389,
2.0807442578011));
#20945=CARTESIAN_POINT('Ctrl Pts',(-0.573033293292122,0.86951340037201,
2.08336110814699));
#20946=CARTESIAN_POINT('Ctrl Pts',(-0.537098976133817,0.890075798227289,
2.08597795849288));
#20947=CARTESIAN_POINT('Ctrl Pts',(-0.501164658975514,0.910638196082568,
2.08859480883878));
#20948=CARTESIAN_POINT('Ctrl Pts',(-0.476284442349319,0.950518522094504,
2.09121165918467));
#20949=CARTESIAN_POINT('Ctrl Pts',(-0.473614938940181,0.991833925232179,
2.09382850953056));
#20950=CARTESIAN_POINT('Ctrl Pts',(-0.470945435531044,1.03314932836985,
2.09644535987645));
#20951=CARTESIAN_POINT('Ctrl Pts',(-0.490486645338963,1.07589980863327,
2.09906221022235));
#20952=CARTESIAN_POINT('Ctrl Pts',(-0.523476043451828,1.10091556225217,
2.10167906056824));
#20953=CARTESIAN_POINT('Ctrl Pts',(-0.556465441564692,1.12593131587107,
2.10429591091413));
#20954=CARTESIAN_POINT('Ctrl Pts',(-0.6029030279825,1.13321234284545,2.10691276126002));
#20955=CARTESIAN_POINT('Ctrl Pts',(-0.64196564416317,1.11949373408075,2.10952961160592));
#20956=CARTESIAN_POINT('Ctrl Pts',(-0.68102826034384,1.10577512531604,2.11214646195181));
#20957=CARTESIAN_POINT('Ctrl Pts',(-0.712715906287371,1.07105688081224,
2.1147633122977));
#20958=CARTESIAN_POINT('Ctrl Pts',(-0.722819461221189,1.03090707921019,
2.1173801626436));
#20959=CARTESIAN_POINT('Ctrl Pts',(-0.725344277841846,1.02087388920281,
2.11803409754971));
#20960=CARTESIAN_POINT('Ctrl Pts',(-0.72652123370157,1.01050151499351,2.11868803245583));
#20961=CARTESIAN_POINT('Ctrl Pts',(-0.726430664085926,1.00010891291408,
2.11934196736194));
#20962=CARTESIAN_POINT('Origin',(-0.6,1.,2.15));
#20963=CARTESIAN_POINT('',(-0.726298666832045,0.999928563942421,2.16934196736194));
#20964=CARTESIAN_POINT('',(-0.72652403561687,0.999901036843312,2.15565803263806));
#20965=CARTESIAN_POINT('',(-0.72645,1.,2.15));
#20966=CARTESIAN_POINT('Ctrl Pts',(-0.72652403561687,0.999901036843312,
2.15565803263806));
#20967=CARTESIAN_POINT('Ctrl Pts',(-0.726228629089082,1.03425627916229,
2.15349217833067));
#20968=CARTESIAN_POINT('Ctrl Pts',(-0.711697061286474,1.06883177008057,
2.15132632402327));
#20969=CARTESIAN_POINT('Ctrl Pts',(-0.686725203134716,1.09229630144258,
2.14916046971588));
#20970=CARTESIAN_POINT('Ctrl Pts',(-0.65655345269935,1.12064685429431,2.14654361936999));
#20971=CARTESIAN_POINT('Ctrl Pts',(-0.611140758111187,1.13277740670372,
2.1439267690241));
#20972=CARTESIAN_POINT('Ctrl Pts',(-0.570850711397976,1.12324847640543,
2.1413099186782));
#20973=CARTESIAN_POINT('Ctrl Pts',(-0.530560664684765,1.11371954610715,
2.13869306833231));
#20974=CARTESIAN_POINT('Ctrl Pts',(-0.495393265846508,1.08253113310118,
2.13607621798642));
#20975=CARTESIAN_POINT('Ctrl Pts',(-0.481117994625666,1.04366848931044,
2.13345936764053));
#20976=CARTESIAN_POINT('Ctrl Pts',(-0.466842723404823,1.00480584551971,
2.13084251729463));
#20977=CARTESIAN_POINT('Ctrl Pts',(-0.473459579801396,0.958268970944215,
2.12822566694874));
#20978=CARTESIAN_POINT('Ctrl Pts',(-0.498001486606679,0.924925559606287,
2.12560881660285));
#20979=CARTESIAN_POINT('Ctrl Pts',(-0.522543393411961,0.89158214826836,
2.12299196625695));
#20980=CARTESIAN_POINT('Ctrl Pts',(-0.565010350625955,0.871432200167998,
2.12037511591106));
#20981=CARTESIAN_POINT('Ctrl Pts',(-0.606359670125879,0.873511179199166,
2.11775826556517));
#20982=CARTESIAN_POINT('Ctrl Pts',(-0.647708989625804,0.875590158230334,
2.11514141521928));
#20983=CARTESIAN_POINT('Ctrl Pts',(-0.687940671411661,0.899898064393031,
2.11252456487338));
#20984=CARTESIAN_POINT('Ctrl Pts',(-0.709014350576037,0.935534967891196,
2.10990771452749));
#20985=CARTESIAN_POINT('Ctrl Pts',(-0.72042201256801,0.954826034551965,
2.10849115389768));
#20986=CARTESIAN_POINT('Ctrl Pts',(-0.726215798894061,0.977436840943303,
2.10707459326787));
#20987=CARTESIAN_POINT('Ctrl Pts',(-0.726259449807842,1.00002674766465,
2.10565803263806));
#20988=CARTESIAN_POINT('Ctrl Pts',(-0.726430664085926,1.00010891291408,
2.11934196736194));
#20989=CARTESIAN_POINT('Ctrl Pts',(-0.726158801404701,0.968913454634673,
2.12130488280172));
#20990=CARTESIAN_POINT('Ctrl Pts',(-0.714466288285182,0.937535739321086,
2.1232677982415));
#20991=CARTESIAN_POINT('Ctrl Pts',(-0.693525863703029,0.914602223563998,
2.12523071368127));
#20992=CARTESIAN_POINT('Ctrl Pts',(-0.665609247326942,0.884028528220152,
2.12784756402716));
#20993=CARTESIAN_POINT('Ctrl Pts',(-0.621256550650662,0.868462496232756,
2.13046441437306));
#20994=CARTESIAN_POINT('Ctrl Pts',(-0.580356049126553,0.874884122700947,
2.13308126471895));
#20995=CARTESIAN_POINT('Ctrl Pts',(-0.539455547602445,0.881305749169137,
2.13569811506484));
#20996=CARTESIAN_POINT('Ctrl Pts',(-0.502007241230509,0.909715034092914,
2.13831496541074));
#20997=CARTESIAN_POINT('Ctrl Pts',(-0.484803396212605,0.947372915741768,
2.14093181575663));
#20998=CARTESIAN_POINT('Ctrl Pts',(-0.467599551194702,0.985030797390621,
2.14354866610252));
#20999=CARTESIAN_POINT('Ctrl Pts',(-0.470640167530832,1.03193727576455,
2.14616551644841));
#21000=CARTESIAN_POINT('Ctrl Pts',(-0.492561796466562,1.06705892873532,
2.14878236679431));
#21001=CARTESIAN_POINT('Ctrl Pts',(-0.514483425402293,1.10218058170609,
2.1513992171402));
#21002=CARTESIAN_POINT('Ctrl Pts',(-0.555286066937625,1.1255174092737,2.15401606748609));
#21003=CARTESIAN_POINT('Ctrl Pts',(-0.596673331719711,1.12660490038116,
2.15663291783198));
#21004=CARTESIAN_POINT('Ctrl Pts',(-0.638060596501796,1.12769239148863,
2.15924976817788));
#21005=CARTESIAN_POINT('Ctrl Pts',(-0.680032484530636,1.10653054613594,
2.16186661852377));
#21006=CARTESIAN_POINT('Ctrl Pts',(-0.703768302238105,1.07260858741574,
2.16448346886966));
#21007=CARTESIAN_POINT('Ctrl Pts',(-0.718457772313683,1.05161518395829,
2.16610296836709));
#21008=CARTESIAN_POINT('Ctrl Pts',(-0.726162745631061,1.02573459982654,
2.16772246786452));
#21009=CARTESIAN_POINT('Ctrl Pts',(-0.726298666832045,0.999928563942421,
2.16934196736194));
#21010=CARTESIAN_POINT('Origin',(-0.6,1.,2.15));
#21011=CARTESIAN_POINT('',(-0.726647750450984,0.999991049383163,2.21934196736194));
#21012=CARTESIAN_POINT('',(-0.726495137942383,1.00010483507083,2.20565803263806));
#21013=CARTESIAN_POINT('',(-0.72645,1.,2.15));
#21014=CARTESIAN_POINT('Ctrl Pts',(-0.726495137942383,1.00010483507083,
2.20565803263806));
#21015=CARTESIAN_POINT('Ctrl Pts',(-0.726567403912713,1.00827186063272,
2.20514346408525));
#21016=CARTESIAN_POINT('Ctrl Pts',(-0.725842471048314,1.01642611993573,
2.20462889553244));
#21017=CARTESIAN_POINT('Ctrl Pts',(-0.72427309126162,1.02441448062962,2.20411432697963));
#21018=CARTESIAN_POINT('Ctrl Pts',(-0.716291973847398,1.06503947477424,
2.20149747663373));
#21019=CARTESIAN_POINT('Ctrl Pts',(-0.686471308333041,1.10137390836652,
2.19888062628784));
#21020=CARTESIAN_POINT('Ctrl Pts',(-0.648183035606218,1.11712498946538,
2.19626377594195));
#21021=CARTESIAN_POINT('Ctrl Pts',(-0.609894762879395,1.13287607056424,
2.19364692559606));
#21022=CARTESIAN_POINT('Ctrl Pts',(-0.563138882940105,1.12804379916968,
2.19103007525017));
#21023=CARTESIAN_POINT('Ctrl Pts',(-0.52888128813228,1.10479502324521,2.18841322490427));
#21024=CARTESIAN_POINT('Ctrl Pts',(-0.494623693324455,1.08154624732075,
2.18579637455838));
#21025=CARTESIAN_POINT('Ctrl Pts',(-0.472864383648094,1.03988096686638,
2.18317952421249));
#21026=CARTESIAN_POINT('Ctrl Pts',(-0.473360492211805,0.998482388849106,
2.18056267386659));
#21027=CARTESIAN_POINT('Ctrl Pts',(-0.473856600775515,0.957083810831832,
2.1779458235207));
#21028=CARTESIAN_POINT('Ctrl Pts',(-0.496608127579297,0.915951935251654,
2.17532897317481));
#21029=CARTESIAN_POINT('Ctrl Pts',(-0.531413017558768,0.893530784155595,
2.17271212282892));
#21030=CARTESIAN_POINT('Ctrl Pts',(-0.56621790753824,0.871109633059536,
2.17009527248302));
#21031=CARTESIAN_POINT('Ctrl Pts',(-0.613076160693402,0.867399206447596,
2.16747842213713));
#21032=CARTESIAN_POINT('Ctrl Pts',(-0.650975979318758,0.884063303502809,
2.16486157179124));
#21033=CARTESIAN_POINT('Ctrl Pts',(-0.688875797944115,0.900727400558021,
2.16224472144534));
#21034=CARTESIAN_POINT('Ctrl Pts',(-0.717817182039666,0.937766021280388,
2.15962787109945));
#21035=CARTESIAN_POINT('Ctrl Pts',(-0.724822470946157,0.978570608288594,
2.15701102075356));
#21036=CARTESIAN_POINT('Ctrl Pts',(-0.726029783985795,0.985602996335628,
2.15656002471506));
#21037=CARTESIAN_POINT('Ctrl Pts',(-0.726585548144894,0.9927472416251,2.15610902867656));
#21038=CARTESIAN_POINT('Ctrl Pts',(-0.72652403561687,0.999901036843312,
2.15565803263806));
#21039=CARTESIAN_POINT('Ctrl Pts',(-0.726298666832045,0.999928563942421,
2.16934196736194));
#21040=CARTESIAN_POINT('Ctrl Pts',(-0.726382372399933,0.984036202243351,
2.17033931821041));
#21041=CARTESIAN_POINT('Ctrl Pts',(-0.723595457458582,0.968172113533461,
2.17133666905888));
#21042=CARTESIAN_POINT('Ctrl Pts',(-0.71780139232639,0.95349516713182,2.17233401990734));
#21043=CARTESIAN_POINT('Ctrl Pts',(-0.702598917321108,0.914985777655832,
2.17495087025323));
#21044=CARTESIAN_POINT('Ctrl Pts',(-0.666694219924447,0.884649070791584,
2.17756772059913));
#21045=CARTESIAN_POINT('Ctrl Pts',(-0.626187393225259,0.876088386528911,
2.18018457094502));
#21046=CARTESIAN_POINT('Ctrl Pts',(-0.58568056652607,0.867527702266238,
2.18280142129091));
#21047=CARTESIAN_POINT('Ctrl Pts',(-0.540571610524354,0.880743040605142,
2.1854182716368));
#21048=CARTESIAN_POINT('Ctrl Pts',(-0.511087917301621,0.909808486730647,
2.1880351219827));
#21049=CARTESIAN_POINT('Ctrl Pts',(-0.481604224078888,0.938873932856152,
2.19065197232859));
#21050=CARTESIAN_POINT('Ctrl Pts',(-0.467745793635136,0.983789486768259,
2.19326882267448));
#21051=CARTESIAN_POINT('Ctrl Pts',(-0.475726910909899,1.02441448020301,
2.19588567302037));
#21052=CARTESIAN_POINT('Ctrl Pts',(-0.483708028184661,1.06503947363776,
2.19850252336627));
#21053=CARTESIAN_POINT('Ctrl Pts',(-0.513528693177939,1.10137390659515,
2.20111937371216));
#21054=CARTESIAN_POINT('Ctrl Pts',(-0.551816965235723,1.11712498741877,
2.20373622405805));
#21055=CARTESIAN_POINT('Ctrl Pts',(-0.590105237293507,1.1328760682424,2.20635307440395));
#21056=CARTESIAN_POINT('Ctrl Pts',(-0.636861116415798,1.12804379693225,
2.20896992474984));
#21057=CARTESIAN_POINT('Ctrl Pts',(-0.671118710625013,1.10479502141404,
2.21158677509573));
#21058=CARTESIAN_POINT('Ctrl Pts',(-0.704960186006201,1.0818286432283,2.21417183918447));
#21059=CARTESIAN_POINT('Ctrl Pts',(-0.726605159802828,1.04089044536347,
2.21675690327321));
#21060=CARTESIAN_POINT('Ctrl Pts',(-0.726647750450984,0.999991049383163,
2.21934196736194));
#21061=CARTESIAN_POINT('Origin',(-0.6,1.,2.15));
#21062=CARTESIAN_POINT('',(-0.726317906690824,1.0000827376849,2.26934196736194));
#21063=CARTESIAN_POINT('',(-0.726267835011577,0.999958186565595,2.25565803263806));
#21064=CARTESIAN_POINT('',(-0.72645,1.,2.15));
#21065=CARTESIAN_POINT('Ctrl Pts',(-0.726267835011577,0.999958186565595,
2.25565803263806));
#21066=CARTESIAN_POINT('Ctrl Pts',(-0.726196218952626,1.02355794991214,
2.25417789949394));
#21067=CARTESIAN_POINT('Ctrl Pts',(-0.719837435721701,1.04719355104496,
2.25269776634982));
#21068=CARTESIAN_POINT('Ctrl Pts',(-0.707438205410818,1.06705892990714,
2.25121763320569));
#21069=CARTESIAN_POINT('Ctrl Pts',(-0.685516576092059,1.10218058349167,
2.2486007828598));
#21070=CARTESIAN_POINT('Ctrl Pts',(-0.644713933843695,1.12551741146695,
2.24598393251391));
#21071=CARTESIAN_POINT('Ctrl Pts',(-0.603326668338405,1.12660490259339,
2.24336708216802));
#21072=CARTESIAN_POINT('Ctrl Pts',(-0.561939402833115,1.12769239371984,
2.24075023182213));
#21073=CARTESIAN_POINT('Ctrl Pts',(-0.519967514070899,1.10653054799744,
2.23813338147623));
#21074=CARTESIAN_POINT('Ctrl Pts',(-0.496231695948683,1.0726085886845,2.23551653113034));
#21075=CARTESIAN_POINT('Ctrl Pts',(-0.472495877826467,1.03868662937157,
2.23289968078445));
#21076=CARTESIAN_POINT('Ctrl Pts',(-0.466996130344251,0.992004556468098,
2.23028283043855));
#21077=CARTESIAN_POINT('Ctrl Pts',(-0.482198605615172,0.9534951663192,2.22766598009266));
#21078=CARTESIAN_POINT('Ctrl Pts',(-0.497401080886093,0.914985776170301,
2.22504912974677));
#21079=CARTESIAN_POINT('Ctrl Pts',(-0.533305778910153,0.884649068775973,
2.22243227940087));
#21080=CARTESIAN_POINT('Ctrl Pts',(-0.573812606317149,0.876088384363716,
2.21981542905498));
#21081=CARTESIAN_POINT('Ctrl Pts',(-0.614319433724146,0.867527699951458,
2.21719857870909));
#21082=CARTESIAN_POINT('Ctrl Pts',(-0.659428390514079,0.88074303852127,
2.2145817283632));
#21083=CARTESIAN_POINT('Ctrl Pts',(-0.688912084252003,0.909808485154657,
2.21196487801731));
#21084=CARTESIAN_POINT('Ctrl Pts',(-0.712598204719431,0.933158601205837,
2.20986259622422));
#21085=CARTESIAN_POINT('Ctrl Pts',(-0.72619989363945,0.96673826214558,2.20776031443114));
#21086=CARTESIAN_POINT('Ctrl Pts',(-0.726495137942383,1.00010483507083,
2.20565803263806));
#21087=CARTESIAN_POINT('Ctrl Pts',(-0.726647750450984,0.999991049383163,
2.21934196736194));
#21088=CARTESIAN_POINT('Ctrl Pts',(-0.726648274150687,0.999488145519468,
2.2193737536191));
#21089=CARTESIAN_POINT('Ctrl Pts',(-0.726645531687645,0.998985247522407,
2.21940553987625));
#21090=CARTESIAN_POINT('Ctrl Pts',(-0.726639505575326,0.99848238887564,
2.21943732613341));
#21091=CARTESIAN_POINT('Ctrl Pts',(-0.726143397020285,0.957083811581739,
2.2220541764793));
#21092=CARTESIAN_POINT('Ctrl Pts',(-0.703391870614066,0.915951936720223,
2.22467102682519));
#21093=CARTESIAN_POINT('Ctrl Pts',(-0.668586981242762,0.893530786015975,
2.22728787717108));
#21094=CARTESIAN_POINT('Ctrl Pts',(-0.633782091871458,0.871109635311727,
2.22990472751698));
#21095=CARTESIAN_POINT('Ctrl Pts',(-0.586923839535069,0.867399208764748,
2.23252157786287));
#21096=CARTESIAN_POINT('Ctrl Pts',(-0.549024021571972,0.884063305528724,
2.23513842820877));
#21097=CARTESIAN_POINT('Ctrl Pts',(-0.511124203608875,0.9007274022927,2.23775527855466));
#21098=CARTESIAN_POINT('Ctrl Pts',(-0.48218282001907,0.93776602236763,2.24037212890055));
#21099=CARTESIAN_POINT('Ctrl Pts',(-0.475177531234974,0.978570608662929,
2.24298897924644));
#21100=CARTESIAN_POINT('Ctrl Pts',(-0.468172242450878,1.01937519495823,
2.24560582959233));
#21101=CARTESIAN_POINT('Ctrl Pts',(-0.483103048472492,1.06394574747389,
2.24822267993823));
#21102=CARTESIAN_POINT('Ctrl Pts',(-0.513274798380673,1.09229629983004,
2.25083953028412));
#21103=CARTESIAN_POINT('Ctrl Pts',(-0.543446548288854,1.12064685218619,
2.25345638063001));
#21104=CARTESIAN_POINT('Ctrl Pts',(-0.588859242083601,1.13277740438282,
2.25607323097591));
#21105=CARTESIAN_POINT('Ctrl Pts',(-0.629149288092737,1.1232484742514,2.2586900813218));
#21106=CARTESIAN_POINT('Ctrl Pts',(-0.669439334101873,1.11371954411997,
2.26130693166769));
#21107=CARTESIAN_POINT('Ctrl Pts',(-0.704606732325397,1.08253113166048,
2.26392378201358));
#21108=CARTESIAN_POINT('Ctrl Pts',(-0.718882003296907,1.04366848854818,
2.26654063235948));
#21109=CARTESIAN_POINT('Ctrl Pts',(-0.723975889834331,1.0298010183647,2.26747441069363));
#21110=CARTESIAN_POINT('Ctrl Pts',(-0.726409587482227,1.01495639047621,
2.26840818902779));
#21111=CARTESIAN_POINT('Ctrl Pts',(-0.726317906690824,1.0000827376849,2.26934196736194));
#21112=CARTESIAN_POINT('Origin',(-0.6,1.,2.15));
#21113=CARTESIAN_POINT('',(-0.72640212307541,0.999893075304641,2.31934196736194));
#21114=CARTESIAN_POINT('',(-0.726626272216059,0.999953562434948,2.30565803263806));
#21115=CARTESIAN_POINT('',(-0.72645,1.,2.15));
#21116=CARTESIAN_POINT('Ctrl Pts',(-0.726626272216059,0.999953562434948,
2.30565803263806));
#21117=CARTESIAN_POINT('Ctrl Pts',(-0.726440890977488,1.03866557446413,
2.30321233490263));
#21118=CARTESIAN_POINT('Ctrl Pts',(-0.707355716298753,1.0775359415853,2.3007666371672));
#21119=CARTESIAN_POINT('Ctrl Pts',(-0.676523957886503,1.10091556401805,
2.29832093943176));
#21120=CARTESIAN_POINT('Ctrl Pts',(-0.643534559198068,1.12593131807613,
2.29570408908587));
#21121=CARTESIAN_POINT('Ctrl Pts',(-0.597096971966626,1.13321234517294,
2.29308723873998));
#21122=CARTESIAN_POINT('Ctrl Pts',(-0.558034355102894,1.11949373616741,
2.29047038839408));
#21123=CARTESIAN_POINT('Ctrl Pts',(-0.518971738239162,1.10577512716188,
2.28785353804819));
#21124=CARTESIAN_POINT('Ctrl Pts',(-0.487284091743139,1.07105688205399,
2.2852366877023));
#21125=CARTESIAN_POINT('Ctrl Pts',(-0.477180536633045,1.03090707975097,
2.28261983735641));
#21126=CARTESIAN_POINT('Ctrl Pts',(-0.467076981522952,0.990757277447954,
2.28000298701051));
#21127=CARTESIAN_POINT('Ctrl Pts',(-0.478557517798788,0.945175917949804,
2.27738613666462));
#21128=CARTESIAN_POINT('Ctrl Pts',(-0.506474134662531,0.914602222071399,
2.27476928631873));
#21129=CARTESIAN_POINT('Ctrl Pts',(-0.534390751526274,0.884028526192994,
2.27215243597283));
#21130=CARTESIAN_POINT('Ctrl Pts',(-0.578743448977924,0.868462493934334,
2.26953558562694));
#21131=CARTESIAN_POINT('Ctrl Pts',(-0.6196439512168,0.874884120514905,2.26691873528105));
#21132=CARTESIAN_POINT('Ctrl Pts',(-0.660544453455676,0.881305747095476,
2.26430188493516));
#21133=CARTESIAN_POINT('Ctrl Pts',(-0.697992760481779,0.909715032515278,
2.26168503458927));
#21134=CARTESIAN_POINT('Ctrl Pts',(-0.715196605800255,0.947372914822063,
2.25906818424337));
#21135=CARTESIAN_POINT('Ctrl Pts',(-0.722669676218981,0.96373088602496,
2.2579314670416));
#21136=CARTESIAN_POINT('Ctrl Pts',(-0.72632283493267,0.981833967767914,
2.25679474983983));
#21137=CARTESIAN_POINT('Ctrl Pts',(-0.726267835011577,0.999958186565595,
2.25565803263806));
#21138=CARTESIAN_POINT('Ctrl Pts',(-0.726317906690824,1.0000827376849,2.26934196736194));
#21139=CARTESIAN_POINT('Ctrl Pts',(-0.726152658292592,0.973273988959771,
2.27102503937368));
#21140=CARTESIAN_POINT('Ctrl Pts',(-0.717783058022956,0.946370945252116,
2.27270811138542));
#21141=CARTESIAN_POINT('Ctrl Pts',(-0.701998511611248,0.924925560916646,
2.27439118339715));
#21142=CARTESIAN_POINT('Ctrl Pts',(-0.677456605234583,0.891582150162549,
2.27700803374305));
#21143=CARTESIAN_POINT('Ctrl Pts',(-0.634989648761757,0.871432202419483,
2.27962488408894));
#21144=CARTESIAN_POINT('Ctrl Pts',(-0.593640329984797,0.873511181412128,
2.28224173443483));
#21145=CARTESIAN_POINT('Ctrl Pts',(-0.552291011207836,0.875590160404774,
2.28485858478073));
#21146=CARTESIAN_POINT('Ctrl Pts',(-0.512059330126741,0.899898066133132,
2.28747543512662));
#21147=CARTESIAN_POINT('Ctrl Pts',(-0.490985651329738,0.935534969012601,
2.29009228547251));
#21148=CARTESIAN_POINT('Ctrl Pts',(-0.469911972532735,0.971171871892071,
2.2927091358184));
#21149=CARTESIAN_POINT('Ctrl Pts',(-0.467996296019824,1.01813777192265,
2.29532598616429));
#21150=CARTESIAN_POINT('Ctrl Pts',(-0.486097632801175,1.0553725535377,2.29794283651019));
#21151=CARTESIAN_POINT('Ctrl Pts',(-0.504198969582526,1.09260733515275,
2.30055968685608));
#21152=CARTESIAN_POINT('Ctrl Pts',(-0.54231731965814,1.12011099835227,2.30317653720197));
#21153=CARTESIAN_POINT('Ctrl Pts',(-0.583359963928024,1.12555066737707,
2.30579338754787));
#21154=CARTESIAN_POINT('Ctrl Pts',(-0.624402608197908,1.13099033640186,
2.30841023789376));
#21155=CARTESIAN_POINT('Ctrl Pts',(-0.668369546662063,1.11436601125193,
2.31102708823965));
#21156=CARTESIAN_POINT('Ctrl Pts',(-0.695545477203344,1.08313205274415,
2.31364393858554));
#21157=CARTESIAN_POINT('Ctrl Pts',(-0.71527010971722,1.0604620524443,2.31554328151101));
#21158=CARTESIAN_POINT('Ctrl Pts',(-0.726149173523156,1.0300956400971,2.31744262443648));
#21159=CARTESIAN_POINT('Ctrl Pts',(-0.72640212307541,0.999893075304641,
2.31934196736194));
#21160=CARTESIAN_POINT('Origin',(-0.6,1.,2.15));
#21161=CARTESIAN_POINT('',(-0.726604172280256,1.00006079745576,2.36934196736194));
#21162=CARTESIAN_POINT('',(-0.726369333664333,1.00010094057762,2.35565803263806));
#21163=CARTESIAN_POINT('',(-0.72645,1.,2.15));
#21164=CARTESIAN_POINT('',(-0.504188384727764,1.08252112989365,2.4));
#21165=CARTESIAN_POINT('Ctrl Pts',(-0.726604172280256,1.00006079745576,
2.36934196736194));
#21166=CARTESIAN_POINT('Ctrl Pts',(-0.7263677230741,0.962556440882506,2.37171076053695));
#21167=CARTESIAN_POINT('Ctrl Pts',(-0.708610935503227,0.92486733001342,
2.37407955371196));
#21168=CARTESIAN_POINT('Ctrl Pts',(-0.679417479773344,0.901356582338566,
2.37644834688697));
#21169=CARTESIAN_POINT('Ctrl Pts',(-0.647166920488327,0.875383817458018,
2.37906519723286));
#21170=CARTESIAN_POINT('Ctrl Pts',(-0.600959009984164,0.866714378341853,
2.38168204757875));
#21171=CARTESIAN_POINT('Ctrl Pts',(-0.561514903279023,0.879318622378776,
2.38429889792465));
#21172=CARTESIAN_POINT('Ctrl Pts',(-0.522070796573882,0.891922866415699,
2.38691574827054));
#21173=CARTESIAN_POINT('Ctrl Pts',(-0.489390493667762,0.92580079360571,
2.38953259861643));
#21174=CARTESIAN_POINT('Ctrl Pts',(-0.478135764397917,0.965573612020961,
2.39214944896232));
#21175=CARTESIAN_POINT('Ctrl Pts',(-0.466881035128071,1.00534643043621,
2.39476629930821));
#21176=CARTESIAN_POINT('Ctrl Pts',(-0.4770518794945,1.0510141400767,2.39738314965411));
#21177=CARTESIAN_POINT('Ctrl Pts',(-0.504188384727764,1.08252112989365,
2.4));
#21178=CARTESIAN_POINT('',(-0.695988964037237,1.08263519275223,2.4));
#21179=CARTESIAN_POINT('Origin',(-0.6,1.,2.4));
#21180=CARTESIAN_POINT('Ctrl Pts',(-0.695989827719566,1.0826357482344,2.4));
#21181=CARTESIAN_POINT('Ctrl Pts',(-0.670163685851419,1.11242103345157,
2.3975091839613));
#21182=CARTESIAN_POINT('Ctrl Pts',(-0.629259696534257,1.12936969176545,
2.3950183679226));
#21183=CARTESIAN_POINT('Ctrl Pts',(-0.589969605883147,1.12624203918417,
2.3925275518839));
#21184=CARTESIAN_POINT('Ctrl Pts',(-0.548691452172472,1.12295612861833,
2.38991070153801));
#21185=CARTESIAN_POINT('Ctrl Pts',(-0.509194654494277,1.09751079858255,
2.38729385119211));
#21186=CARTESIAN_POINT('Ctrl Pts',(-0.489166158833217,1.06128256815865,
2.38467700084622));
#21187=CARTESIAN_POINT('Ctrl Pts',(-0.469137663172157,1.02505433773475,
2.38206015050033));
#21188=CARTESIAN_POINT('Ctrl Pts',(-0.468577469528232,0.978043206922726,
2.37944330015444));
#21189=CARTESIAN_POINT('Ctrl Pts',(-0.487748907242888,0.94134646243954,
2.37682644980854));
#21190=CARTESIAN_POINT('Ctrl Pts',(-0.506920344957544,0.904649717956355,
2.37420959946265));
#21191=CARTESIAN_POINT('Ctrl Pts',(-0.54582341403078,0.878267359802006,
2.37159274911676));
#21192=CARTESIAN_POINT('Ctrl Pts',(-0.587007343519609,0.874020939484002,
2.36897589877086));
#21193=CARTESIAN_POINT('Ctrl Pts',(-0.628191273008439,0.869774519165998,
2.36635904842497));
#21194=CARTESIAN_POINT('Ctrl Pts',(-0.671656062912861,0.887664036684341,
2.36374219807908));
#21195=CARTESIAN_POINT('Ctrl Pts',(-0.697914726064929,0.919672001884272,
2.36112534773319));
#21196=CARTESIAN_POINT('Ctrl Pts',(-0.716201899123246,0.94196312902452,
2.35930290936814));
#21197=CARTESIAN_POINT('Ctrl Pts',(-0.726143981825042,0.971101800838385,
2.3574804710031));
#21198=CARTESIAN_POINT('Ctrl Pts',(-0.726369333664333,1.00010094057762,
2.35565803263806));
#21199=CARTESIAN_POINT('Origin',(0.6,1.,2.51042117235887));
#21200=CARTESIAN_POINT('',(0.44550661348391,1.00007637252271,2.03957882764113));
#21201=CARTESIAN_POINT('',(0.445941879748409,0.999994887077554,2.03542117235887));
#21202=CARTESIAN_POINT('',(0.4457,1.,2.51042117235887));
#21203=CARTESIAN_POINT('',(0.639851384185725,0.850935057178149,2.));
#21204=CARTESIAN_POINT('Ctrl Pts',(0.445941879748409,0.999994887077554,
2.03542117235887));
#21205=CARTESIAN_POINT('Ctrl Pts',(0.445958427563446,1.02606888540753,2.03408151628949));
#21206=CARTESIAN_POINT('Ctrl Pts',(0.464522119816522,1.10309173428669,2.03012500987421));
#21207=CARTESIAN_POINT('Ctrl Pts',(0.585586764715563,1.18108624726655,2.02355165311303));
#21208=CARTESIAN_POINT('Ctrl Pts',(0.74321627607811,1.11199512704675,2.01570110207536));
#21209=CARTESIAN_POINT('Ctrl Pts',(0.772174135599484,0.94213024790789,2.00785055103768));
#21210=CARTESIAN_POINT('Ctrl Pts',(0.688870364005735,0.864039910406678,
2.00261685034589));
#21211=CARTESIAN_POINT('Ctrl Pts',(0.639851384185725,0.850935057178149,
2.));
#21212=CARTESIAN_POINT('',(0.560048264277831,0.850698128346977,2.));
#21213=CARTESIAN_POINT('Origin',(0.6,1.,2.));
#21214=CARTESIAN_POINT('Ctrl Pts',(0.44550661348391,1.00007637252271,2.03957882764113));
#21215=CARTESIAN_POINT('Ctrl Pts',(0.445479076365182,1.00461168797626,2.03934410251636));
#21216=CARTESIAN_POINT('Ctrl Pts',(0.447699955244927,1.0596817411018,2.03649252704569));
#21217=CARTESIAN_POINT('Ctrl Pts',(0.513561617374857,1.15981701056446,2.03102410122914));
#21218=CARTESIAN_POINT('Ctrl Pts',(0.685634169421134,1.1602711276025,2.02317355019146));
#21219=CARTESIAN_POINT('Ctrl Pts',(0.780906782004492,1.01693885807272,2.01532299915378));
#21220=CARTESIAN_POINT('Ctrl Pts',(0.715015266367875,0.861059909554376,
2.00759848242329));
#21221=CARTESIAN_POINT('Ctrl Pts',(0.606562024823064,0.838426846369365,
2.0024908160387));
#21222=CARTESIAN_POINT('Ctrl Pts',(0.560047775926799,0.850696975355777,
2.));
#21223=CARTESIAN_POINT('Origin',(0.6,1.,2.51042117235887));
#21224=CARTESIAN_POINT('',(0.445932524475483,1.00003263872856,2.08957882764113));
#21225=CARTESIAN_POINT('',(0.445538932974414,0.999905097479817,2.08542117235887));
#21226=CARTESIAN_POINT('',(0.4457,1.,2.51042117235887));
#21227=CARTESIAN_POINT('Ctrl Pts',(0.445538932974414,0.999905097479817,
2.08542117235887));
#21228=CARTESIAN_POINT('Ctrl Pts',(0.445863620600756,1.04447123493477,2.08311595169817));
#21229=CARTESIAN_POINT('Ctrl Pts',(0.489384741719965,1.14018208017193,2.07819388069158));
#21230=CARTESIAN_POINT('Ctrl Pts',(0.651047898079357,1.17438225782416,2.0706549593391));
#21231=CARTESIAN_POINT('Ctrl Pts',(0.773614618887169,1.05360877841752,2.06280440830142));
#21232=CARTESIAN_POINT('Ctrl Pts',(0.740475677832241,0.884752178886651,
2.05495385726374));
#21233=CARTESIAN_POINT('Ctrl Pts',(0.581362560637208,0.819263360725568,
2.04710330622607));
#21234=CARTESIAN_POINT('Ctrl Pts',(0.463250898323639,0.899361552534091,
2.04059241125778));
#21235=CARTESIAN_POINT('Ctrl Pts',(0.445926103479307,0.975136595316218,
2.03669836663538));
#21236=CARTESIAN_POINT('Ctrl Pts',(0.445941879748409,0.999994887077554,
2.03542117235887));
#21237=CARTESIAN_POINT('Ctrl Pts',(0.445932524475483,1.00003263872856,2.08957882764113));
#21238=CARTESIAN_POINT('Ctrl Pts',(0.445887391771903,1.02338938965811,2.08837853792505));
#21239=CARTESIAN_POINT('Ctrl Pts',(0.461764469489331,1.09760988546538,2.08456139786307));
#21240=CARTESIAN_POINT('Ctrl Pts',(0.57612672137744,1.18012607114374,2.07812740745521));
#21241=CARTESIAN_POINT('Ctrl Pts',(0.737078048375186,1.11926881624917,2.07027685641753));
#21242=CARTESIAN_POINT('Ctrl Pts',(0.775094502137202,0.951447557128672,
2.06242630537985));
#21243=CARTESIAN_POINT('Ctrl Pts',(0.656082084236305,0.827171040068,2.05457575434217));
#21244=CARTESIAN_POINT('Ctrl Pts',(0.491836019895195,0.856969773295158,
2.04695992842926));
#21245=CARTESIAN_POINT('Ctrl Pts',(0.445786075962011,0.954049389522044,
2.04196095286225));
#21246=CARTESIAN_POINT('Ctrl Pts',(0.44550661348391,1.00007637252271,2.03957882764113));
#21247=CARTESIAN_POINT('Origin',(0.6,1.,2.51042117235887));
#21248=CARTESIAN_POINT('',(0.445609664942012,0.999879240692409,2.13957882764113));
#21249=CARTESIAN_POINT('',(0.445723577648801,1.00013290047684,2.13542117235887));
#21250=CARTESIAN_POINT('',(0.4457,1.,2.51042117235887));
#21251=CARTESIAN_POINT('Ctrl Pts',(0.445723577648801,1.00013290047684,2.13542117235887));
#21252=CARTESIAN_POINT('Ctrl Pts',(0.445613060502099,1.01281442421482,2.13476723745276));
#21253=CARTESIAN_POINT('Ctrl Pts',(0.45279637409468,1.07612012598108,2.13149645220075));
#21254=CARTESIAN_POINT('Ctrl Pts',(0.539792347657613,1.17143637275151,2.12560881660284));
#21255=CARTESIAN_POINT('Ctrl Pts',(0.70978808601476,1.14478245624706,2.11775826556517));
#21256=CARTESIAN_POINT('Ctrl Pts',(0.781323293607615,0.988284239491303,
2.10990771452749));
#21257=CARTESIAN_POINT('Ctrl Pts',(0.690243392316909,0.842292899938004,
2.10205716348982));
#21258=CARTESIAN_POINT('Ctrl Pts',(0.518231205927094,0.837737224374896,
2.09420661245213));
#21259=CARTESIAN_POINT('Ctrl Pts',(0.448527232502997,0.937309583846461,
2.08866128207516));
#21260=CARTESIAN_POINT('Ctrl Pts',(0.445495040298755,0.993880454536856,
2.08573280204407));
#21261=CARTESIAN_POINT('Ctrl Pts',(0.445538932974414,0.999905097479817,
2.08542117235887));
#21262=CARTESIAN_POINT('Ctrl Pts',(0.445609664942012,0.999879240692409,
2.13957882764113));
#21263=CARTESIAN_POINT('Ctrl Pts',(0.445970133311311,1.04180105694513,2.13741297333374));
#21264=CARTESIAN_POINT('Ctrl Pts',(0.485126633726011,1.13496755094661,2.13263026868045));
#21265=CARTESIAN_POINT('Ctrl Pts',(0.641820162707069,1.17682322770038,2.12523071368128));
#21266=CARTESIAN_POINT('Ctrl Pts',(0.770558701511974,1.06265070285456,2.11738016264359));
#21267=CARTESIAN_POINT('Ctrl Pts',(0.746336141641471,0.892291522696776,
2.10952961160592));
#21268=CARTESIAN_POINT('Ctrl Pts',(0.590875851708506,0.818527896169216,
2.10167906056824));
#21269=CARTESIAN_POINT('Ctrl Pts',(0.466115932152929,0.893907603907564,
2.09502879924665));
#21270=CARTESIAN_POINT('Ctrl Pts',(0.445985789291595,0.972467415629669,
2.09099538827094));
#21271=CARTESIAN_POINT('Ctrl Pts',(0.445932524475483,1.00003263872856,2.08957882764113));
#21272=CARTESIAN_POINT('Origin',(0.6,1.,2.51042117235887));
#21273=CARTESIAN_POINT('',(0.445644927187824,1.00012792448195,2.18957882764113));
#21274=CARTESIAN_POINT('',(0.445884646673086,0.999912830487253,2.18542117235887));
#21275=CARTESIAN_POINT('',(0.4457,1.,2.51042117235887));
#21276=CARTESIAN_POINT('Ctrl Pts',(0.445884646673086,0.999912830487253,
2.18542117235887));
#21277=CARTESIAN_POINT('Ctrl Pts',(0.446050503878428,1.03140252422683,2.18380167286145));
#21278=CARTESIAN_POINT('Ctrl Pts',(0.470644510125523,1.11401244662307,2.17956532301813));
#21279=CARTESIAN_POINT('Ctrl Pts',(0.604772735062981,1.18163868139168,2.17271212282892));
#21280=CARTESIAN_POINT('Ctrl Pts',(0.754140428515542,1.09620871962996,2.16486157179123));
#21281=CARTESIAN_POINT('Ctrl Pts',(0.765271321801097,0.924496491715462,
2.15701102075356));
#21282=CARTESIAN_POINT('Ctrl Pts',(0.628182963406343,0.820497603368372,
2.14916046971588));
#21283=CARTESIAN_POINT('Ctrl Pts',(0.479344005128078,0.872734156235485,
2.14196385358432));
#21284=CARTESIAN_POINT('Ctrl Pts',(0.446055316804476,0.962066789442876,
2.13738408779865));
#21285=CARTESIAN_POINT('Ctrl Pts',(0.445723577648801,1.00013290047684,2.13542117235887));
#21286=CARTESIAN_POINT('Ctrl Pts',(0.445644927187824,1.00012792448195,2.18957882764113));
#21287=CARTESIAN_POINT('Ctrl Pts',(0.445556744991309,1.01009369744184,2.18906425908832));
#21288=CARTESIAN_POINT('Ctrl Pts',(0.450939973182116,1.07064584055842,2.18593284018961));
#21289=CARTESIAN_POINT('Ctrl Pts',(0.530872330435983,1.16803793011858,2.18018457094502));
#21290=CARTESIAN_POINT('Ctrl Pts',(0.702033231237909,1.1503482635805,2.17233401990734));
#21291=CARTESIAN_POINT('Ctrl Pts',(0.781688304564893,0.997822700079642,
2.16448346886966));
#21292=CARTESIAN_POINT('Ctrl Pts',(0.698400986961052,0.847249790637147,
2.15663291783198));
#21293=CARTESIAN_POINT('Ctrl Pts',(0.526865324912526,0.833666900912216,
2.14878236679431));
#21294=CARTESIAN_POINT('Ctrl Pts',(0.450147764311532,0.931848543518796,
2.14309767006402));
#21295=CARTESIAN_POINT('Ctrl Pts',(0.445534604580841,0.991149857098978,
2.14002982367963));
#21296=CARTESIAN_POINT('Ctrl Pts',(0.445609664942012,0.999879240692409,
2.13957882764113));
#21297=CARTESIAN_POINT('Origin',(0.6,1.,2.51042117235887));
#21298=CARTESIAN_POINT('',(0.445922292476226,0.999948977361648,2.23957882764113));
#21299=CARTESIAN_POINT('',(0.445458679031241,0.999989078051821,2.23542117235887));
#21300=CARTESIAN_POINT('',(0.4457,1.,2.51042117235887));
#21301=CARTESIAN_POINT('Ctrl Pts',(0.445458679031242,0.999989078051821,
2.23542117235887));
#21302=CARTESIAN_POINT('Ctrl Pts',(0.445510650069037,1.04989637335789,2.23283610827014));
#21303=CARTESIAN_POINT('Ctrl Pts',(0.498659772012076,1.15041990786983,2.22763419383551));
#21304=CARTESIAN_POINT('Ctrl Pts',(0.669127678863374,1.16803795272366,2.21981542905498));
#21305=CARTESIAN_POINT('Ctrl Pts',(0.778293256865801,1.03502719068774,2.21196487801731));
#21306=CARTESIAN_POINT('Ctrl Pts',(0.727561203441069,0.870603211369231,
2.20411432697963));
#21307=CARTESIAN_POINT('Ctrl Pts',(0.562429230156179,0.822225348280642,
2.19626377594195));
#21308=CARTESIAN_POINT('Ctrl Pts',(0.458106037926808,0.910370419295299,
2.1900327244017));
#21309=CARTESIAN_POINT('Ctrl Pts',(0.445782505348105,0.980520250977966,
2.18641852320734));
#21310=CARTESIAN_POINT('Ctrl Pts',(0.445884646673086,0.999912830487253,
2.18542117235887));
#21311=CARTESIAN_POINT('Ctrl Pts',(0.445922292476226,0.999948977361648,
2.23957882764113));
#21312=CARTESIAN_POINT('Ctrl Pts',(0.446009681621634,1.02874647305155,2.23809869449701));
#21313=CARTESIAN_POINT('Ctrl Pts',(0.467487221018094,1.10857850003564,2.23400171100699));
#21314=CARTESIAN_POINT('Ctrl Pts',(0.595227265578502,1.18163865695784,2.22728787717108));
#21315=CARTESIAN_POINT('Ctrl Pts',(0.748875240939872,1.10417074102503,2.21943732613341));
#21316=CARTESIAN_POINT('Ctrl Pts',(0.769008360762544,0.933280028245809,
2.21158677509573));
#21317=CARTESIAN_POINT('Ctrl Pts',(0.637570764789711,0.822225372195567,
2.20373622405805));
#21318=CARTESIAN_POINT('Ctrl Pts',(0.483262475482066,0.867432276377129,
2.19640024157318));
#21319=CARTESIAN_POINT('Ctrl Pts',(0.446005197603095,0.959412527217309,
2.19168110943421));
#21320=CARTESIAN_POINT('Ctrl Pts',(0.445644927187824,1.00012792448195,2.18957882764113));
#21321=CARTESIAN_POINT('Origin',(0.6,1.,2.51042117235887));
#21322=CARTESIAN_POINT('',(0.445484911225394,0.999943334804163,2.28957882764113));
#21323=CARTESIAN_POINT('',(0.445861169326679,1.00010096027373,2.28542117235887));
#21324=CARTESIAN_POINT('',(0.4457,1.,2.51042117235887));
#21325=CARTESIAN_POINT('Ctrl Pts',(0.445861169326679,1.00010096027373,2.28542117235887));
#21326=CARTESIAN_POINT('Ctrl Pts',(0.445749296272184,1.01825046503264,2.28448739402472));
#21327=CARTESIAN_POINT('Ctrl Pts',(0.457041409544473,1.08712805126299,2.28093676534467));
#21328=CARTESIAN_POINT('Ctrl Pts',(0.558179831669208,1.17682325150234,2.27476928631873));
#21329=CARTESIAN_POINT('Ctrl Pts',(0.724423708785572,1.13241650393702,2.26691873528105));
#21330=CARTESIAN_POINT('Ctrl Pts',(0.779081445955335,0.969255483615749,
2.25906818424337));
#21331=CARTESIAN_POINT('Ctrl Pts',(0.673134684925636,0.833666878534013,
2.25121763320569));
#21332=CARTESIAN_POINT('Ctrl Pts',(0.50159899980171,0.84724977008965,2.24336708216802));
#21333=CARTESIAN_POINT('Ctrl Pts',(0.445736890155226,0.948241381044753,
2.23810159521908));
#21334=CARTESIAN_POINT('Ctrl Pts',(0.445458039989146,0.999375411980858,
2.23545295861603));
#21335=CARTESIAN_POINT('Ctrl Pts',(0.445458679031242,0.999989078051821,
2.23542117235887));
#21336=CARTESIAN_POINT('Ctrl Pts',(0.445484911225394,0.999943334804162,
2.28957882764113));
#21337=CARTESIAN_POINT('Ctrl Pts',(0.445711121771824,1.04718147797272,2.2871331299057));
#21338=CARTESIAN_POINT('Ctrl Pts',(0.493918064875951,1.14536352796849,2.28207058182437));
#21339=CARTESIAN_POINT('Ctrl Pts',(0.660207644220989,1.17143634973614,2.27439118339715));
#21340=CARTESIAN_POINT('Ctrl Pts',(0.776207730757634,1.04434204382826,2.26654063235948));
#21341=CARTESIAN_POINT('Ctrl Pts',(0.734180526190243,0.87748075149375,2.2586900813218));
#21342=CARTESIAN_POINT('Ctrl Pts',(0.571817040388558,0.820497627508739,
2.25083953028412));
#21343=CARTESIAN_POINT('Ctrl Pts',(0.460575165814633,0.904888683245033,
2.24446911239056));
#21344=CARTESIAN_POINT('Ctrl Pts',(0.445855179091712,0.977832988101724,
2.2407155448429));
#21345=CARTESIAN_POINT('Ctrl Pts',(0.445922292476226,0.999948977361648,
2.23957882764113));
#21346=CARTESIAN_POINT('Origin',(0.6,1.,2.51042117235887));
#21347=CARTESIAN_POINT('',(0.445798439227784,1.00012317213786,2.33957882764113));
#21348=CARTESIAN_POINT('',(0.445758404806891,0.999869526120069,2.33542117235887));
#21349=CARTESIAN_POINT('',(0.4457,1.,2.51042117235887));
#21350=CARTESIAN_POINT('Ctrl Pts',(0.445758404806891,0.999869526120069,
2.33542117235887));
#21351=CARTESIAN_POINT('Ctrl Pts',(0.446067065282869,1.03672406343128,2.33352182943341));
#21352=CARTESIAN_POINT('Ctrl Pts',(0.477632210806756,1.12483092984331,2.32900563616205));
#21353=CARTESIAN_POINT('Ctrl Pts',(0.623873281963166,1.1801260959606,2.3218725925448));
#21354=CARTESIAN_POINT('Ctrl Pts',(0.76341449322476,1.07944244879737,2.31402204150712));
#21355=CARTESIAN_POINT('Ctrl Pts',(0.756401707578768,0.907512694301026,
2.30617149046944));
#21356=CARTESIAN_POINT('Ctrl Pts',(0.609124149502328,0.818527871661859,
2.29832093943176));
#21357=CARTESIAN_POINT('Ctrl Pts',(0.472154957249585,0.883517743796439,
2.29140416672824));
#21358=CARTESIAN_POINT('Ctrl Pts',(0.446062812907388,0.967387710919709,
2.28710424437061));
#21359=CARTESIAN_POINT('Ctrl Pts',(0.445861169326679,1.00010096027373,2.28542117235887));
#21360=CARTESIAN_POINT('Ctrl Pts',(0.445798439227784,1.00012317213786,2.33957882764113));
#21361=CARTESIAN_POINT('Ctrl Pts',(0.445678571748812,1.01554817070058,2.33878441566028));
#21362=CARTESIAN_POINT('Ctrl Pts',(0.454838216821075,1.08164530296445,2.33537315333353));
#21363=CARTESIAN_POINT('Ctrl Pts',(0.548952109888326,1.17438223097154,2.3293450406609));
#21364=CARTESIAN_POINT('Ctrl Pts',(0.717297767916034,1.1387683610531,2.32149448962322));
#21365=CARTESIAN_POINT('Ctrl Pts',(0.780449022522885,0.978702297157564,
2.31364393858554));
#21366=CARTESIAN_POINT('Ctrl Pts',(0.681768782849741,0.837737246759644,
2.30579338754786));
#21367=CARTESIAN_POINT('Ctrl Pts',(0.509756619949943,0.842292920851884,
2.29794283651019));
#21368=CARTESIAN_POINT('Ctrl Pts',(0.447051029253845,0.942803275635825,
2.29253798320794));
#21369=CARTESIAN_POINT('Ctrl Pts',(0.445469080763202,0.996637557724894,
2.28974998025159));
#21370=CARTESIAN_POINT('Ctrl Pts',(0.445484911225394,0.999943334804162,
2.28957882764113));
#21371=CARTESIAN_POINT('Origin',(0.6,1.,2.51042117235887));
#21372=CARTESIAN_POINT('',(0.445864724392684,0.99983533609866,2.38957882764113));
#21373=CARTESIAN_POINT('',(0.44551185913013,1.0000741974826,2.38542117235887));
#21374=CARTESIAN_POINT('',(0.4457,1.,2.51042117235887));
#21375=CARTESIAN_POINT('',(0.560148615814278,0.850935057178148,2.4));
#21376=CARTESIAN_POINT('Ctrl Pts',(0.560148615814278,0.850935057178148,
2.4));
#21377=CARTESIAN_POINT('Ctrl Pts',(0.511129635994267,0.864039910406677,
2.39738314965411));
#21378=CARTESIAN_POINT('Ctrl Pts',(0.455839024989005,0.915869990257929,
2.39390942553448));
#21379=CARTESIAN_POINT('Ctrl Pts',(0.445750544275333,0.983186184474914,
2.39043570141486));
#21380=CARTESIAN_POINT('Ctrl Pts',(0.445864724392684,0.99983533609866,2.38957882764113));
#21381=CARTESIAN_POINT('',(0.639951772688379,0.850698147244252,2.4));
#21382=CARTESIAN_POINT('Origin',(0.6,1.,2.4));
#21383=CARTESIAN_POINT('Ctrl Pts',(0.639952262351544,0.850696991672977,
2.4));
#21384=CARTESIAN_POINT('Ctrl Pts',(0.593438030028895,0.838426877605595,
2.3975091839613));
#21385=CARTESIAN_POINT('Ctrl Pts',(0.490251767896999,0.859960628309645,
2.39264957474759));
#21386=CARTESIAN_POINT('Ctrl Pts',(0.445800376826071,0.954309672447724,
2.38778996553388));
#21387=CARTESIAN_POINT('Ctrl Pts',(0.445511859130131,1.0000741974826,2.38542117235887));
#21388=CARTESIAN_POINT('Origin',(-0.6,1.,2.51042117235887));
#21389=CARTESIAN_POINT('',(-0.75449339269049,1.00007637145626,2.03957882764113));
#21390=CARTESIAN_POINT('',(-0.754058103775977,0.999994895029031,2.03542117235887));
#21391=CARTESIAN_POINT('',(-0.7543,1.,2.51042117235887));
#21392=CARTESIAN_POINT('',(-0.560148615814275,0.850935057178149,2.));
#21393=CARTESIAN_POINT('Ctrl Pts',(-0.754058103775977,0.999994895029031,
2.03542117235887));
#21394=CARTESIAN_POINT('Ctrl Pts',(-0.754041555268885,1.02606889659328,
2.03408151628949));
#21395=CARTESIAN_POINT('Ctrl Pts',(-0.735477862467914,1.10309174989979,
2.03012500987421));
#21396=CARTESIAN_POINT('Ctrl Pts',(-0.614413230072635,1.18108614472194,
2.02355165311304));
#21397=CARTESIAN_POINT('Ctrl Pts',(-0.456783762484268,1.11199525865091,
2.01570110207535));
#21398=CARTESIAN_POINT('Ctrl Pts',(-0.427825820216639,0.942129974923708,
2.00785055103768));
#21399=CARTESIAN_POINT('Ctrl Pts',(-0.511129635994264,0.864039910406679,
2.00261685034589));
#21400=CARTESIAN_POINT('Ctrl Pts',(-0.560148615814275,0.850935057178149,
2.));
#21401=CARTESIAN_POINT('',(-0.639951747396791,0.850698134330425,2.));
#21402=CARTESIAN_POINT('Origin',(-0.6,1.,2.));
#21403=CARTESIAN_POINT('Ctrl Pts',(-0.754493392690491,1.00007637145626,
2.03957882764113));
#21404=CARTESIAN_POINT('Ctrl Pts',(-0.754520929823858,1.00461168712382,
2.03934410251636));
#21405=CARTESIAN_POINT('Ctrl Pts',(-0.752300051092223,1.05968174304917,
2.03649252704569));
#21406=CARTESIAN_POINT('Ctrl Pts',(-0.686438388751686,1.15981702310584,
2.03102410122914));
#21407=CARTESIAN_POINT('Ctrl Pts',(-0.514365822072695,1.16027112465931,
2.02317355019146));
#21408=CARTESIAN_POINT('Ctrl Pts',(-0.41909321999119,1.01693887482571,2.01532299915378));
#21409=CARTESIAN_POINT('Ctrl Pts',(-0.484984709990756,0.861059878644944,
2.00759848242329));
#21410=CARTESIAN_POINT('Ctrl Pts',(-0.593437992489385,0.838426856238601,
2.0024908160387));
#21411=CARTESIAN_POINT('Ctrl Pts',(-0.63995223616215,0.850696980524376,
2.));
#21412=CARTESIAN_POINT('Origin',(-0.6,1.,2.51042117235887));
#21413=CARTESIAN_POINT('',(-0.754067482051008,1.00003263870824,2.08957882764113));
#21414=CARTESIAN_POINT('',(-0.754461050156182,0.999905097350985,2.08542117235887));
#21415=CARTESIAN_POINT('',(-0.7543,1.,2.51042117235887));
#21416=CARTESIAN_POINT('Ctrl Pts',(-0.754461050156182,0.999905097350985,
2.08542117235887));
#21417=CARTESIAN_POINT('Ctrl Pts',(-0.754136362473472,1.0444712301837,2.08311595169818));
#21418=CARTESIAN_POINT('Ctrl Pts',(-0.71061524567478,1.14018206615738,2.07819388069158));
#21419=CARTESIAN_POINT('Ctrl Pts',(-0.548952108412014,1.17438223594748,
2.0706549593391));
#21420=CARTESIAN_POINT('Ctrl Pts',(-0.426385398697532,1.05360877753029,
2.06280440830142));
#21421=CARTESIAN_POINT('Ctrl Pts',(-0.459524339782119,0.884752182582313,
2.05495385726375));
#21422=CARTESIAN_POINT('Ctrl Pts',(-0.618637434184013,0.819263396393857,
2.04710330622607));
#21423=CARTESIAN_POINT('Ctrl Pts',(-0.736749089275893,0.89936154319225,
2.04059241125778));
#21424=CARTESIAN_POINT('Ctrl Pts',(-0.754073880704865,0.975136600184218,
2.03669836663538));
#21425=CARTESIAN_POINT('Ctrl Pts',(-0.754058103775977,0.999994895029031,
2.03542117235887));
#21426=CARTESIAN_POINT('Ctrl Pts',(-0.754067482051008,1.00003263870824,
2.08957882764113));
#21427=CARTESIAN_POINT('Ctrl Pts',(-0.754112614754579,1.02338939061779,
2.08837853792505));
#21428=CARTESIAN_POINT('Ctrl Pts',(-0.738235536361179,1.09760988955354,
2.08456139786307));
#21429=CARTESIAN_POINT('Ctrl Pts',(-0.623873279675432,1.18012607896462,
2.0781274074552));
#21430=CARTESIAN_POINT('Ctrl Pts',(-0.462921945732953,1.11926882096942,
2.07027685641753));
#21431=CARTESIAN_POINT('Ctrl Pts',(-0.424905490600427,0.951447555675582,
2.06242630537985));
#21432=CARTESIAN_POINT('Ctrl Pts',(-0.54391791306908,0.827171031659744,
2.05457575434217));
#21433=CARTESIAN_POINT('Ctrl Pts',(-0.708163985289881,0.856969769057042,
2.04695992842926));
#21434=CARTESIAN_POINT('Ctrl Pts',(-0.754213930063824,0.954049386283767,
2.04196095286225));
#21435=CARTESIAN_POINT('Ctrl Pts',(-0.754493392690491,1.00007637145626,
2.03957882764113));
#21436=CARTESIAN_POINT('Origin',(-0.6,1.,2.51042117235887));
#21437=CARTESIAN_POINT('',(-0.754390341602871,0.999879240687419,2.13957882764113));
#21438=CARTESIAN_POINT('',(-0.75427640544451,1.00013290045585,2.13542117235887));
#21439=CARTESIAN_POINT('',(-0.7543,1.,2.51042117235887));
#21440=CARTESIAN_POINT('Ctrl Pts',(-0.75427640544451,1.00013290045585,2.13542117235887));
#21441=CARTESIAN_POINT('Ctrl Pts',(-0.754386922579298,1.01281442280347,
2.13476723745276));
#21442=CARTESIAN_POINT('Ctrl Pts',(-0.747203609773684,1.07612011763199,
2.13149645220075));
#21443=CARTESIAN_POINT('Ctrl Pts',(-0.660207645725328,1.17143635399922,
2.12560881660285));
#21444=CARTESIAN_POINT('Ctrl Pts',(-0.490211926051119,1.14478244030651,
2.11775826556517));
#21445=CARTESIAN_POINT('Ctrl Pts',(-0.418676726208604,0.988284240908056,
2.10990771452749));
#21446=CARTESIAN_POINT('Ctrl Pts',(-0.509756617677689,0.842292916978238,
2.10205716348981));
#21447=CARTESIAN_POINT('Ctrl Pts',(-0.681768784928714,0.837737242612945,
2.09420661245213));
#21448=CARTESIAN_POINT('Ctrl Pts',(-0.75147275106401,0.937309590263154,
2.08866128207516));
#21449=CARTESIAN_POINT('Ctrl Pts',(-0.754504942839462,0.993880455032877,
2.08573280204407));
#21450=CARTESIAN_POINT('Ctrl Pts',(-0.754461050156182,0.999905097350985,
2.08542117235887));
#21451=CARTESIAN_POINT('Ctrl Pts',(-0.75439034160287,0.999879240687419,
2.13957882764113));
#21452=CARTESIAN_POINT('Ctrl Pts',(-0.754029873218229,1.04180105871682,
2.13741297333374));
#21453=CARTESIAN_POINT('Ctrl Pts',(-0.714873371143386,1.13496755666601,
2.13263026868045));
#21454=CARTESIAN_POINT('Ctrl Pts',(-0.558179835520779,1.17682323520091,
2.12523071368127));
#21455=CARTESIAN_POINT('Ctrl Pts',(-0.429441291256411,1.0626507055017,2.1173801626436));
#21456=CARTESIAN_POINT('Ctrl Pts',(-0.453663852157743,0.892291518147041,
2.10952961160592));
#21457=CARTESIAN_POINT('Ctrl Pts',(-0.609124148673025,0.818527888446316,
2.10167906056824));
#21458=CARTESIAN_POINT('Ctrl Pts',(-0.733884073530661,0.893907599452349,
2.09502879924664));
#21459=CARTESIAN_POINT('Ctrl Pts',(-0.754014217234906,0.972467414452767,
2.09099538827094));
#21460=CARTESIAN_POINT('Ctrl Pts',(-0.754067482051008,1.00003263870824,
2.08957882764113));
#21461=CARTESIAN_POINT('Origin',(-0.6,1.,2.51042117235887));
#21462=CARTESIAN_POINT('',(-0.754355079355554,1.00012792448738,2.18957882764113));
#21463=CARTESIAN_POINT('',(-0.754115336434833,0.999912830496762,2.18542117235887));
#21464=CARTESIAN_POINT('',(-0.7543,1.,2.51042117235887));
#21465=CARTESIAN_POINT('Ctrl Pts',(-0.754115336434833,0.999912830496762,
2.18542117235887));
#21466=CARTESIAN_POINT('Ctrl Pts',(-0.753949479247709,1.03140252078477,
2.18380167286145));
#21467=CARTESIAN_POINT('Ctrl Pts',(-0.72935547569638,1.11401243412622,2.17956532301813));
#21468=CARTESIAN_POINT('Ctrl Pts',(-0.595227265459685,1.1816386614837,2.17271212282892));
#21469=CARTESIAN_POINT('Ctrl Pts',(-0.445859588380167,1.09620870908317,
2.16486157179124));
#21470=CARTESIAN_POINT('Ctrl Pts',(-0.434728696312199,0.924496499994273,
2.15701102075356));
#21471=CARTESIAN_POINT('Ctrl Pts',(-0.571817039685625,0.820497623037239,
2.14916046971588));
#21472=CARTESIAN_POINT('Ctrl Pts',(-0.720655981642513,0.872734170194251,
2.14196385358432));
#21473=CARTESIAN_POINT('Ctrl Pts',(-0.753944666324598,0.962066793595335,
2.13738408779865));
#21474=CARTESIAN_POINT('Ctrl Pts',(-0.75427640544451,1.00013290045585,2.13542117235887));
#21475=CARTESIAN_POINT('Ctrl Pts',(-0.754355079355553,1.00012792448738,
2.18957882764113));
#21476=CARTESIAN_POINT('Ctrl Pts',(-0.754443261555807,1.01009369786974,
2.18906425908832));
#21477=CARTESIAN_POINT('Ctrl Pts',(-0.749060033136799,1.07064584355324,
2.18593284018961));
#21478=CARTESIAN_POINT('Ctrl Pts',(-0.669127672494447,1.16803793724193,
2.18018457094502));
#21479=CARTESIAN_POINT('Ctrl Pts',(-0.497966764436741,1.15034826995414,
2.17233401990734));
#21480=CARTESIAN_POINT('Ctrl Pts',(-0.418311687733005,0.997822699987136,
2.16448346886966));
#21481=CARTESIAN_POINT('Ctrl Pts',(-0.501599008867606,0.847249784162188,
2.15663291783199));
#21482=CARTESIAN_POINT('Ctrl Pts',(-0.673134678187691,0.833666893860354,
2.1487823667943));
#21483=CARTESIAN_POINT('Ctrl Pts',(-0.749852242041061,0.931848540630513,
2.14309767006402));
#21484=CARTESIAN_POINT('Ctrl Pts',(-0.754465401967237,0.99114985672403,
2.14002982367963));
#21485=CARTESIAN_POINT('Ctrl Pts',(-0.75439034160287,0.999879240687419,
2.13957882764113));
#21486=CARTESIAN_POINT('Origin',(-0.6,1.,2.51042117235887));
#21487=CARTESIAN_POINT('',(-0.75407771405525,0.999948977359204,2.23957882764113));
#21488=CARTESIAN_POINT('',(-0.754541304029948,0.999989078053162,2.23542117235887));
#21489=CARTESIAN_POINT('',(-0.7543,1.,2.51042117235887));
#21490=CARTESIAN_POINT('Ctrl Pts',(-0.754541304029948,0.999989078053162,
2.23542117235887));
#21491=CARTESIAN_POINT('Ctrl Pts',(-0.754489332997837,1.04989636788915,
2.23283610827014));
#21492=CARTESIAN_POINT('Ctrl Pts',(-0.701340216880369,1.15041989138249,
2.2276341938355));
#21493=CARTESIAN_POINT('Ctrl Pts',(-0.530872328713473,1.16803793430571,
2.21981542905499));
#21494=CARTESIAN_POINT('Ctrl Pts',(-0.421706762676398,1.0350271868484,2.2119648780173));
#21495=CARTESIAN_POINT('Ctrl Pts',(-0.472438810540477,0.870603225552124,
2.20411432697963));
#21496=CARTESIAN_POINT('Ctrl Pts',(-0.637570765725878,0.822225367765818,
2.19626377594195));
#21497=CARTESIAN_POINT('Ctrl Pts',(-0.741893946520544,0.910370429119493,
2.1900327244017));
#21498=CARTESIAN_POINT('Ctrl Pts',(-0.754217477748594,0.980520253113081,
2.18641852320734));
#21499=CARTESIAN_POINT('Ctrl Pts',(-0.754115336434833,0.999912830496762,
2.18542117235887));
#21500=CARTESIAN_POINT('Ctrl Pts',(-0.75407771405525,0.999948977359204,
2.23957882764113));
#21501=CARTESIAN_POINT('Ctrl Pts',(-0.753990324906209,1.02874647427002,
2.23809869449701));
#21502=CARTESIAN_POINT('Ctrl Pts',(-0.732512784599607,1.10857850463897,
2.23400171100699));
#21503=CARTESIAN_POINT('Ctrl Pts',(-0.604772734623643,1.18163866465747,
2.22728787717109));
#21504=CARTESIAN_POINT('Ctrl Pts',(-0.451124752749149,1.10417074544119,
2.21943732613341));
#21505=CARTESIAN_POINT('Ctrl Pts',(-0.43099163207285,0.933280025417337,
2.21158677509573));
#21506=CARTESIAN_POINT('Ctrl Pts',(-0.562429233617627,0.822225364659454,
2.20373622405805));
#21507=CARTESIAN_POINT('Ctrl Pts',(-0.716737529466624,0.867432270757321,
2.19640024157319));
#21508=CARTESIAN_POINT('Ctrl Pts',(-0.753994808925007,0.959412525496741,
2.19168110943421));
#21509=CARTESIAN_POINT('Ctrl Pts',(-0.754355079355553,1.00012792448738,
2.18957882764113));
#21510=CARTESIAN_POINT('Origin',(-0.6,1.,2.51042117235887));
#21511=CARTESIAN_POINT('',(-0.754515095317817,0.999943334786189,2.28957882764113));
#21512=CARTESIAN_POINT('',(-0.754138813779314,1.00010096025924,2.28542117235887));
#21513=CARTESIAN_POINT('',(-0.7543,1.,2.51042117235887));
#21514=CARTESIAN_POINT('Ctrl Pts',(-0.754138813779314,1.00010096025924,
2.28542117235887));
#21515=CARTESIAN_POINT('Ctrl Pts',(-0.754250686820938,1.01825046303266,
2.28448739402472));
#21516=CARTESIAN_POINT('Ctrl Pts',(-0.74295857478395,1.08712804172823,2.28093676534467));
#21517=CARTESIAN_POINT('Ctrl Pts',(-0.641820163748749,1.17682323210921,
2.27476928631873));
#21518=CARTESIAN_POINT('Ctrl Pts',(-0.47557630485125,1.13241648942973,2.26691873528105));
#21519=CARTESIAN_POINT('Ctrl Pts',(-0.420918573673669,0.969255486982105,
2.25906818424337));
#21520=CARTESIAN_POINT('Ctrl Pts',(-0.526865323090207,0.833666896767115,
2.2512176332057));
#21521=CARTESIAN_POINT('Ctrl Pts',(-0.698400989412974,0.847249786831145,
2.24336708216802));
#21522=CARTESIAN_POINT('Ctrl Pts',(-0.75426309293647,0.948241386717884,
2.23810159521908));
#21523=CARTESIAN_POINT('Ctrl Pts',(-0.754541943071973,0.999375412049459,
2.23545295861603));
#21524=CARTESIAN_POINT('Ctrl Pts',(-0.754541304029948,0.999989078053162,
2.23542117235887));
#21525=CARTESIAN_POINT('Ctrl Pts',(-0.754515095317817,0.999943334786189,
2.28957882764113));
#21526=CARTESIAN_POINT('Ctrl Pts',(-0.754288884759399,1.04718147995109,
2.2871331299057));
#21527=CARTESIAN_POINT('Ctrl Pts',(-0.706081939633174,1.1453635341575,2.28207058182437));
#21528=CARTESIAN_POINT('Ctrl Pts',(-0.539792353219763,1.17143635698873,
2.27439118339715));
#21529=CARTESIAN_POINT('Ctrl Pts',(-0.423792261776434,1.04434204571596,
2.26654063235948));
#21530=CARTESIAN_POINT('Ctrl Pts',(-0.465819468119529,0.877480746295693,
2.2586900813218));
#21531=CARTESIAN_POINT('Ctrl Pts',(-0.6281829608073,0.820497619901593,2.25083953028412));
#21532=CARTESIAN_POINT('Ctrl Pts',(-0.73942484009554,0.90488867921255,2.24446911239056));
#21533=CARTESIAN_POINT('Ctrl Pts',(-0.754144827442555,0.977832987161639,
2.2407155448429));
#21534=CARTESIAN_POINT('Ctrl Pts',(-0.75407771405525,0.999948977359204,
2.23957882764113));
#21535=CARTESIAN_POINT('Origin',(-0.6,1.,2.51042117235887));
#21536=CARTESIAN_POINT('',(-0.754201567294635,1.0001231722509,2.33957882764113));
#21537=CARTESIAN_POINT('',(-0.754241578414675,0.999869525658411,2.33542117235887));
#21538=CARTESIAN_POINT('',(-0.7543,1.,2.51042117235887));
#21539=CARTESIAN_POINT('Ctrl Pts',(-0.754241578414675,0.999869525658411,
2.33542117235887));
#21540=CARTESIAN_POINT('Ctrl Pts',(-0.753932917948777,1.03672405905087,
2.33352182943341));
#21541=CARTESIAN_POINT('Ctrl Pts',(-0.72236777560142,1.12483091690338,2.32900563616205));
#21542=CARTESIAN_POINT('Ctrl Pts',(-0.576126720758545,1.18012607574093,
2.3218725925448));
#21543=CARTESIAN_POINT('Ctrl Pts',(-0.436585524633584,1.079442440351,2.31402204150712));
#21544=CARTESIAN_POINT('Ctrl Pts',(-0.443598309590693,0.907512704295987,
2.30617149046944));
#21545=CARTESIAN_POINT('Ctrl Pts',(-0.59087585148424,0.818527891629664,
2.29832093943176));
#21546=CARTESIAN_POINT('Ctrl Pts',(-0.727845028742113,0.883517756536112,
2.29140416672824));
#21547=CARTESIAN_POINT('Ctrl Pts',(-0.753937170221803,0.967387714483928,
2.28710424437061));
#21548=CARTESIAN_POINT('Ctrl Pts',(-0.754138813779314,1.00010096025924,
2.28542117235887));
#21549=CARTESIAN_POINT('Ctrl Pts',(-0.754201567294635,1.0001231722509,2.33957882764113));
#21550=CARTESIAN_POINT('Ctrl Pts',(-0.754321434708458,1.01554817119723,
2.33878441566028));
#21551=CARTESIAN_POINT('Ctrl Pts',(-0.745161788983251,1.08164530518807,
2.33537315333353));
#21552=CARTESIAN_POINT('Ctrl Pts',(-0.651047892623131,1.17438223943631,
2.3293450406609));
#21553=CARTESIAN_POINT('Ctrl Pts',(-0.48270222690289,1.13876836634555,2.32149448962322));
#21554=CARTESIAN_POINT('Ctrl Pts',(-0.419550969949932,0.978702296577685,
2.31364393858554));
#21555=CARTESIAN_POINT('Ctrl Pts',(-0.518231213613428,0.837737239705173,
2.30579338754787));
#21556=CARTESIAN_POINT('Ctrl Pts',(-0.690243383915708,0.842292914261777,
2.29794283651019));
#21557=CARTESIAN_POINT('Ctrl Pts',(-0.752948977226896,0.9428032732054,2.29253798320794));
#21558=CARTESIAN_POINT('Ctrl Pts',(-0.754530925780848,0.996637557567215,
2.28974998025159));
#21559=CARTESIAN_POINT('Ctrl Pts',(-0.754515095317817,0.999943334786189,
2.28957882764113));
#21560=CARTESIAN_POINT('Origin',(-0.6,1.,2.51042117235887));
#21561=CARTESIAN_POINT('',(-0.754135271629158,0.999835375941562,2.38957882764113));
#21562=CARTESIAN_POINT('',(-0.754488127978201,1.0000741878009,2.38542117235887));
#21563=CARTESIAN_POINT('',(-0.7543,1.,2.51042117235887));
#21564=CARTESIAN_POINT('',(-0.639851384185722,0.850935057178148,2.4));
#21565=CARTESIAN_POINT('Ctrl Pts',(-0.639851384185722,0.850935057178148,
2.4));
#21566=CARTESIAN_POINT('Ctrl Pts',(-0.688870364005733,0.864039910406677,
2.39738314965411));
#21567=CARTESIAN_POINT('Ctrl Pts',(-0.744160963654378,0.915870060408085,
2.39390942553448));
#21568=CARTESIAN_POINT('Ctrl Pts',(-0.754249449960209,0.983186232192211,
2.39043570141486));
#21569=CARTESIAN_POINT('Ctrl Pts',(-0.754135271629158,0.999835375941562,
2.38957882764113));
#21570=CARTESIAN_POINT('',(-0.560048257412569,0.850698131867252,2.4));
#21571=CARTESIAN_POINT('Origin',(-0.6,1.,2.4));
#21572=CARTESIAN_POINT('Ctrl Pts',(-0.56004776881791,0.850696978396875,
2.4));
#21573=CARTESIAN_POINT('Ctrl Pts',(-0.606562014643699,0.838426852173434,
2.3975091839613));
#21574=CARTESIAN_POINT('Ctrl Pts',(-0.709748176229453,0.859960702974294,
2.39264957474759));
#21575=CARTESIAN_POINT('Ctrl Pts',(-0.754199601979702,0.954309678356425,
2.38778996553388));
#21576=CARTESIAN_POINT('Ctrl Pts',(-0.754488127978201,1.0000741878009,2.38542117235887));
#21577=CARTESIAN_POINT('Origin',(-0.6,1.,2.51042117235887));
#21578=CARTESIAN_POINT('Ctrl Pts',(-0.754488127978201,1.0000741878009,2.38542117235887));
#21579=CARTESIAN_POINT('Ctrl Pts',(-0.754518342073576,1.00486659216084,
2.38517311518799));
#21580=CARTESIAN_POINT('Ctrl Pts',(-0.75215961407118,1.06018735745674,2.38230820767121));
#21581=CARTESIAN_POINT('Ctrl Pts',(-0.685634174422424,1.16027112587027,
2.37682644980854));
#21582=CARTESIAN_POINT('Ctrl Pts',(-0.513561613772921,1.15981701793772,
2.36897589877087));
#21583=CARTESIAN_POINT('Ctrl Pts',(-0.419009660745144,1.01606137072615,
2.36112534773318));
#21584=CARTESIAN_POINT('Ctrl Pts',(-0.486773837186857,0.857888188850051,
2.35327479669551));
#21585=CARTESIAN_POINT('Ctrl Pts',(-0.656082085820325,0.827171035125292,
2.34542424565783));
#21586=CARTESIAN_POINT('Ctrl Pts',(-0.746300935356365,0.921380401738197,
2.33947303754562));
#21587=CARTESIAN_POINT('Ctrl Pts',(-0.754358179883375,0.985947131323567,
2.3361386797793));
#21588=CARTESIAN_POINT('Ctrl Pts',(-0.754241578414675,0.999869525658411,
2.33542117235887));
#21589=CARTESIAN_POINT('Ctrl Pts',(-0.754135271629158,0.999835375941562,
2.38957882764113));
#21590=CARTESIAN_POINT('Ctrl Pts',(-0.753900754954872,1.03403189804748,
2.38781885106897));
#21591=CARTESIAN_POINT('Ctrl Pts',(-0.726011265053425,1.1195363898437,2.38344202415091));
#21592=CARTESIAN_POINT('Ctrl Pts',(-0.585586769094172,1.18108616109394,
2.37644834688697));
#21593=CARTESIAN_POINT('Ctrl Pts',(-0.44099944093888,1.08793753892263,2.36859779584929));
#21594=CARTESIAN_POINT('Ctrl Pts',(-0.438948720197302,0.915842224941729,
2.36074724481161));
#21595=CARTESIAN_POINT('Ctrl Pts',(-0.581362564989717,0.819263390701727,
2.35289669377393));
#21596=CARTESIAN_POINT('Ctrl Pts',(-0.724374710267433,0.878125248400964,
2.34584055471711));
#21597=CARTESIAN_POINT('Ctrl Pts',(-0.753926582804302,0.964737112450477,
2.34140126600617));
#21598=CARTESIAN_POINT('Ctrl Pts',(-0.754201567294635,1.0001231722509,2.33957882764113));
#21599=CARTESIAN_POINT('Ctrl Pts',(-0.504188384727764,1.08252112989365,
2.4));
#21600=CARTESIAN_POINT('Ctrl Pts',(-0.4770518794945,1.0510141400767,2.39738314965411));
#21601=CARTESIAN_POINT('Ctrl Pts',(-0.456710190761643,0.959678720795721,
2.39214944896232));
#21602=CARTESIAN_POINT('Ctrl Pts',(-0.554751099480001,0.858044939225688,
2.38429889792465));
#21603=CARTESIAN_POINT('Ctrl Pts',(-0.69337483099249,0.884053256574183,
2.37644834688697));
#21604=CARTESIAN_POINT('Ctrl Pts',(-0.7482544551901,1.01388152850897,2.36859779584929));
#21605=CARTESIAN_POINT('Ctrl Pts',(-0.670177844171844,1.13134338215356,
2.36074724481161));
#21606=CARTESIAN_POINT('Ctrl Pts',(-0.52916309826044,1.13097123731837,2.35289669377393));
#21607=CARTESIAN_POINT('Ctrl Pts',(-0.451677068057184,1.01316241301569,
2.34504614273626));
#21608=CARTESIAN_POINT('Ctrl Pts',(-0.507210315698497,0.883538311601356,
2.33719559169857));
#21609=CARTESIAN_POINT('Ctrl Pts',(-0.645959687310304,0.858365375188547,
2.3293450406609));
#21610=CARTESIAN_POINT('Ctrl Pts',(-0.743491252981436,0.960210910505111,
2.32149448962322));
#21611=CARTESIAN_POINT('Ctrl Pts',(-0.712336485126218,1.097741686102,2.31364393858554));
#21612=CARTESIAN_POINT('Ctrl Pts',(-0.580435669733753,1.14761466155179,
2.30579338754787));
#21613=CARTESIAN_POINT('Ctrl Pts',(-0.466080619506913,1.06510367195323,
2.29794283651019));
#21614=CARTESIAN_POINT('Ctrl Pts',(-0.471827649045646,0.924205971861489,
2.29009228547251));
#21615=CARTESIAN_POINT('Ctrl Pts',(-0.592522692288931,0.851282254676416,
2.28224173443483));
#21616=CARTESIAN_POINT('Ctrl Pts',(-0.719923561707409,0.911732097905615,
2.27439118339715));
#21617=CARTESIAN_POINT('Ctrl Pts',(-0.739774130548921,1.051342719201,2.26654063235948));
#21618=CARTESIAN_POINT('Ctrl Pts',(-0.634271935878349,1.14490795657946,
2.2586900813218));
#21619=CARTESIAN_POINT('Ctrl Pts',(-0.498033854494106,1.10851629998956,
2.25083953028412));
#21620=CARTESIAN_POINT('Ctrl Pts',(-0.453241436429265,0.974804642442561,
2.24298897924644));
#21621=CARTESIAN_POINT('Ctrl Pts',(-0.540065587198681,0.86368878221777,
2.23513842820877));
#21622=CARTESIAN_POINT('Ctrl Pts',(-0.680640344207846,0.874820061858706,
2.22728787717108));
#21623=CARTESIAN_POINT('Ctrl Pts',(-0.748894923426505,0.998215686443256,
2.21943732613341));
#21624=CARTESIAN_POINT('Ctrl Pts',(-0.68361699553809,1.12321152562211,2.21158677509573));
#21625=CARTESIAN_POINT('Ctrl Pts',(-0.543349358171216,1.13770833955254,
2.20373622405805));
#21626=CARTESIAN_POINT('Ctrl Pts',(-0.453887363191384,1.02870504068037,
2.19588567302037));
#21627=CARTESIAN_POINT('Ctrl Pts',(-0.49546265452264,0.893958378944044,
2.1880351219827));
#21628=CARTESIAN_POINT('Ctrl Pts',(-0.630789522527785,0.854312363927335,
2.18018457094502));
#21629=CARTESIAN_POINT('Ctrl Pts',(-0.73850361471777,0.945322484520081,
2.17233401990734));
#21630=CARTESIAN_POINT('Ctrl Pts',(-0.722004372559477,1.08536870078326,
2.16448346886966));
#21631=CARTESIAN_POINT('Ctrl Pts',(-0.596088708472957,1.14885423684131,
2.15663291783199));
#21632=CARTESIAN_POINT('Ctrl Pts',(-0.473680783866961,1.07884375413848,
2.14878236679431));
#21633=CARTESIAN_POINT('Ctrl Pts',(-0.464558934858572,0.938124319016692,
2.14093181575663));
#21634=CARTESIAN_POINT('Ctrl Pts',(-0.576903853974382,0.85289646424536,
2.13308126471895));
#21635=CARTESIAN_POINT('Ctrl Pts',(-0.709961944003222,0.899594560207548,
2.12523071368127));
#21636=CARTESIAN_POINT('Ctrl Pts',(-0.744403552230901,1.03633863630844,
2.1173801626436));
#21637=CARTESIAN_POINT('Ctrl Pts',(-0.64934061440031,1.14049336981984,2.10952961160591));
#21638=CARTESIAN_POINT('Ctrl Pts',(-0.510027855146882,1.11865028889668,
2.10167906056824));
#21639=CARTESIAN_POINT('Ctrl Pts',(-0.451404225723124,0.99039884810644,
2.09382850953056));
#21640=CARTESIAN_POINT('Ctrl Pts',(-0.526044875601709,0.87075787007063,
2.08597795849289));
#21641=CARTESIAN_POINT('Ctrl Pts',(-0.667010128672949,0.867024460974769,
2.0781274074552));
#21642=CARTESIAN_POINT('Ctrl Pts',(-0.747879322472409,0.982546373509308,
2.07027685641753));
#21643=CARTESIAN_POINT('Ctrl Pts',(-0.696126397524862,1.11372170867476,
2.06242630537985));
#21644=CARTESIAN_POINT('Ctrl Pts',(-0.558165872383014,1.14290754203214,
2.05457575434217));
#21645=CARTESIAN_POINT('Ctrl Pts',(-0.457721540280641,1.04393279273302,
2.04672520330449));
#21646=CARTESIAN_POINT('Ctrl Pts',(-0.484879149484439,0.905553554682652,
2.03887465226682));
#21647=CARTESIAN_POINT('Ctrl Pts',(-0.615273516218849,0.851885006312401,
2.03102410122914));
#21648=CARTESIAN_POINT('Ctrl Pts',(-0.731982722301914,0.931032073672457,
2.02317355019146));
#21649=CARTESIAN_POINT('Ctrl Pts',(-0.730302140552184,1.07206547359851,
2.01532299915378));
#21650=CARTESIAN_POINT('Ctrl Pts',(-0.611811749466523,1.14840144523713,
2.0074724481161));
#21651=CARTESIAN_POINT('Ctrl Pts',(-0.482633225963291,1.09178094916661,
1.99962189707843));
#21652=CARTESIAN_POINT('Ctrl Pts',(-0.45890197645103,0.952575083143895,
1.99177134604075));
#21653=CARTESIAN_POINT('Ctrl Pts',(-0.527170074345267,0.888579693265875,
1.98653764534896));
#21654=CARTESIAN_POINT('Ctrl Pts',(-0.56734149364689,0.877840168374445,
1.98392079500307));
#21655=CARTESIAN_POINT('Ctrl Pts',(-0.497154370004338,1.08857942294107,
2.40535973499898));
#21656=CARTESIAN_POINT('Ctrl Pts',(-0.468025636826573,1.05475934582637,
2.40274288465309));
#21657=CARTESIAN_POINT('Ctrl Pts',(-0.446190561956348,0.956718531983702,
2.3975091839613));
#21658=CARTESIAN_POINT('Ctrl Pts',(-0.551429149092544,0.847623301048373,
2.38965863292362));
#21659=CARTESIAN_POINT('Ctrl Pts',(-0.700229949071154,0.875541020369071,
2.38180808188594));
#21660=CARTESIAN_POINT('Ctrl Pts',(-0.759138563736414,1.01490064164717,
2.37395753084827));
#21661=CARTESIAN_POINT('Ctrl Pts',(-0.675329954255372,1.14098596339246,
2.36610697981059));
#21662=CARTESIAN_POINT('Ctrl Pts',(-0.523962603431266,1.14058649752482,
2.35825642877291));
#21663=CARTESIAN_POINT('Ctrl Pts',(-0.440787932286505,1.01412873225251,
2.35040587773523));
#21664=CARTESIAN_POINT('Ctrl Pts',(-0.500398156194616,0.874988270684254,
2.34255532669756));
#21665=CARTESIAN_POINT('Ctrl Pts',(-0.649333820146978,0.84796726183413,
2.33470477565988));
#21666=CARTESIAN_POINT('Ctrl Pts',(-0.754025670789615,0.957289792428312,
2.3268542246222));
#21667=CARTESIAN_POINT('Ctrl Pts',(-0.720583674030304,1.10491739707588,
2.31900367358452));
#21668=CARTESIAN_POINT('Ctrl Pts',(-0.578999353408684,1.15845179961484,
2.31115312254684));
#21669=CARTESIAN_POINT('Ctrl Pts',(-0.456248921215803,1.06988326141916,
2.30330257150917));
#21670=CARTESIAN_POINT('Ctrl Pts',(-0.462417869227328,0.918641549339655,
2.29545202047149));
#21671=CARTESIAN_POINT('Ctrl Pts',(-0.591973745354034,0.840364133660832,
2.28760146943381));
#21672=CARTESIAN_POINT('Ctrl Pts',(-0.728727756233707,0.905251905277888,
2.27975091839613));
#21673=CARTESIAN_POINT('Ctrl Pts',(-0.750035655620193,1.05511204760418,
2.27190036735845));
#21674=CARTESIAN_POINT('Ctrl Pts',(-0.636788011835149,1.15554638175604,
2.26404981632077));
#21675=CARTESIAN_POINT('Ctrl Pts',(-0.490548004613153,1.11648302980295,
2.2561992652831));
#21676=CARTESIAN_POINT('Ctrl Pts',(-0.442467148844067,0.972954923955743,
2.24834871424542));
#21677=CARTESIAN_POINT('Ctrl Pts',(-0.535665499162523,0.85368148706755,
2.24049816320774));
#21678=CARTESIAN_POINT('Ctrl Pts',(-0.686560559276222,0.865629970182854,
2.23264761217006));
#21679=CARTESIAN_POINT('Ctrl Pts',(-0.759826051981739,0.998084690970592,
2.22479706113239));
#21680=CARTESIAN_POINT('Ctrl Pts',(-0.689755741618848,1.13225710619039,
2.21694651009471));
#21681=CARTESIAN_POINT('Ctrl Pts',(-0.539190348351968,1.14781820447026,
2.20909595905703));
#21682=CARTESIAN_POINT('Ctrl Pts',(-0.443160496353055,1.03081242273638,
2.20124540801935));
#21683=CARTESIAN_POINT('Ctrl Pts',(-0.48778803986192,0.886173327813403,
2.19339485698167));
#21684=CARTESIAN_POINT('Ctrl Pts',(-0.633049936927148,0.843616698540163,
2.185544305944));
#21685=CARTESIAN_POINT('Ctrl Pts',(-0.748671864803154,0.941308331874462,
2.17769375490632));
#21686=CARTESIAN_POINT('Ctrl Pts',(-0.730961329922812,1.09163604839579,
2.16984320386864));
#21687=CARTESIAN_POINT('Ctrl Pts',(-0.595801560801866,1.15978237838877,
2.16199265283096));
#21688=CARTESIAN_POINT('Ctrl Pts',(-0.46440705203803,1.08463207245338,2.15414210179328));
#21689=CARTESIAN_POINT('Ctrl Pts',(-0.454615522009781,0.933581712675886,
2.14629155075561));
#21690=CARTESIAN_POINT('Ctrl Pts',(-0.575208249211462,0.842096850509319,
2.13844099971793));
#21691=CARTESIAN_POINT('Ctrl Pts',(-0.718034805847138,0.892223289617803,
2.13059044868025));
#21692=CARTESIAN_POINT('Ctrl Pts',(-0.755004946535977,1.03900643918491,
2.12273989764257));
#21693=CARTESIAN_POINT('Ctrl Pts',(-0.652962958175316,1.15080769787963,
2.11488934660489));
#21694=CARTESIAN_POINT('Ctrl Pts',(-0.503422545448295,1.12736100603329,
2.10703879556722));
#21695=CARTESIAN_POINT('Ctrl Pts',(-0.440495059218284,0.989693979040313,
2.09918824452954));
#21696=CARTESIAN_POINT('Ctrl Pts',(-0.520615456293703,0.861269552373166,
2.09133769349186));
#21697=CARTESIAN_POINT('Ctrl Pts',(-0.671929680758203,0.857262054854161,
2.08348714245418));
#21698=CARTESIAN_POINT('Ctrl Pts',(-0.758735890630724,0.98126501461181,
2.07563659141651));
#21699=CARTESIAN_POINT('Ctrl Pts',(-0.703183522003752,1.12207059383778,
2.06778604037882));
#21700=CARTESIAN_POINT('Ctrl Pts',(-0.555094617726015,1.15339910667059,
2.05993548934115));
#21701=CARTESIAN_POINT('Ctrl Pts',(-0.447276159752938,1.04715812099878,
2.05208493830347));
#21702=CARTESIAN_POINT('Ctrl Pts',(-0.476427546250332,0.89861976398254,
2.0442343872658));
#21703=CARTESIAN_POINT('Ctrl Pts',(-0.616394822207238,0.841011136339552,
2.03638383622811));
#21704=CARTESIAN_POINT('Ctrl Pts',(-0.74167224073109,0.925968789770463,
2.02853328519044));
#21705=CARTESIAN_POINT('Ctrl Pts',(-0.73986827898471,1.07735616409467,2.02068273415276));
#21706=CARTESIAN_POINT('Ctrl Pts',(-0.612678909668559,1.1592963450654,2.01283218311508));
#21707=CARTESIAN_POINT('Ctrl Pts',(-0.474016738136951,1.09851905232804,
2.0049816320774));
#21708=CARTESIAN_POINT('Ctrl Pts',(-0.448543257706232,0.949093380403833,
1.99713108103973));
#21709=CARTESIAN_POINT('Ctrl Pts',(-0.5218232615616,0.880399765646143,1.99189738034794));
#21710=CARTESIAN_POINT('Ctrl Pts',(-0.564943867702685,0.86887179797568,
1.98928053000205));
#21711=CARTESIAN_POINT('Ctrl Pts',(-0.490120355280912,1.09463771598849,
2.41071946999795));
#21712=CARTESIAN_POINT('Ctrl Pts',(-0.458999394158645,1.05850455157604,
2.40810261965206));
#21713=CARTESIAN_POINT('Ctrl Pts',(-0.435670933151054,0.953758343171685,
2.40286891896027));
#21714=CARTESIAN_POINT('Ctrl Pts',(-0.548107198705087,0.837201662871056,
2.3950183679226));
#21715=CARTESIAN_POINT('Ctrl Pts',(-0.707085067149817,0.867028784163962,
2.38716781688492));
#21716=CARTESIAN_POINT('Ctrl Pts',(-0.770022672282728,1.01591975478537,
2.37931726584724));
#21717=CARTESIAN_POINT('Ctrl Pts',(-0.680482064338898,1.15062854463137,
2.37146671480957));
#21718=CARTESIAN_POINT('Ctrl Pts',(-0.518762108602093,1.15020175773127,
2.36361616377188));
#21719=CARTESIAN_POINT('Ctrl Pts',(-0.429898796515824,1.01509505148933,
2.35576561273421));
#21720=CARTESIAN_POINT('Ctrl Pts',(-0.493585996690737,0.866438229767152,
2.34791506169653));
#21721=CARTESIAN_POINT('Ctrl Pts',(-0.652707952983651,0.837569148479711,
2.34006451065885));
#21722=CARTESIAN_POINT('Ctrl Pts',(-0.764560088597795,0.954368674351516,
2.33221395962117));
#21723=CARTESIAN_POINT('Ctrl Pts',(-0.728830862934391,1.11209310804976,
2.3243634085835));
#21724=CARTESIAN_POINT('Ctrl Pts',(-0.577563037083615,1.16928893767788,
2.31651285754582));
#21725=CARTESIAN_POINT('Ctrl Pts',(-0.446417222924693,1.07466285088508,
2.30866230650814));
#21726=CARTESIAN_POINT('Ctrl Pts',(-0.453008089409011,0.913077126817822,
2.30081175547046));
#21727=CARTESIAN_POINT('Ctrl Pts',(-0.591424798419137,0.829446012645248,
2.29296120443278));
#21728=CARTESIAN_POINT('Ctrl Pts',(-0.737531950760006,0.89877171265016,
2.28511065339511));
#21729=CARTESIAN_POINT('Ctrl Pts',(-0.760297180691466,1.05888137600737,
2.27726010235743));
#21730=CARTESIAN_POINT('Ctrl Pts',(-0.639304087791949,1.16618480693263,
2.26940955131975));
#21731=CARTESIAN_POINT('Ctrl Pts',(-0.483062154732201,1.12444975961634,
2.26155900028207));
#21732=CARTESIAN_POINT('Ctrl Pts',(-0.431692861258868,0.971105205468923,
2.25370844924439));
#21733=CARTESIAN_POINT('Ctrl Pts',(-0.531265411126364,0.843674191917333,
2.24585789820672));
#21734=CARTESIAN_POINT('Ctrl Pts',(-0.692480774344598,0.856439878506999,
2.23800734716904));
#21735=CARTESIAN_POINT('Ctrl Pts',(-0.770757180536974,0.997953695497927,
2.23015679613137));
#21736=CARTESIAN_POINT('Ctrl Pts',(-0.695894487699607,1.14130268675866,
2.22230624509368));
#21737=CARTESIAN_POINT('Ctrl Pts',(-0.53503133853272,1.15792806938798,2.21445569405601));
#21738=CARTESIAN_POINT('Ctrl Pts',(-0.432433629514727,1.03291980479239,
2.20660514301833));
#21739=CARTESIAN_POINT('Ctrl Pts',(-0.480113425201198,0.878388276682764,
2.19875459198065));
#21740=CARTESIAN_POINT('Ctrl Pts',(-0.635310351326514,0.83292103315299,
2.19090404094297));
#21741=CARTESIAN_POINT('Ctrl Pts',(-0.758840114888534,0.937294179228842,
2.18305348990529));
#21742=CARTESIAN_POINT('Ctrl Pts',(-0.739918287286149,1.09790339600832,
2.17520293886762));
#21743=CARTESIAN_POINT('Ctrl Pts',(-0.595514413130776,1.17071051993624,
2.16735238782994));
#21744=CARTESIAN_POINT('Ctrl Pts',(-0.455133320209099,1.09042039076827,
2.15950183679226));
#21745=CARTESIAN_POINT('Ctrl Pts',(-0.44467210916099,0.92903910633508,2.15165128575458));
#21746=CARTESIAN_POINT('Ctrl Pts',(-0.573512644448544,0.831297236773279,
2.14380073471691));
#21747=CARTESIAN_POINT('Ctrl Pts',(-0.726107667691055,0.884852019028058,
2.13595018367922));
#21748=CARTESIAN_POINT('Ctrl Pts',(-0.765606340841053,1.04167424206138,
2.12809963264155));
#21749=CARTESIAN_POINT('Ctrl Pts',(-0.656585301950322,1.16112202593943,
2.12024908160387));
#21750=CARTESIAN_POINT('Ctrl Pts',(-0.496817235749707,1.1360717231699,2.11239853056619));
#21751=CARTESIAN_POINT('Ctrl Pts',(-0.429585892713444,0.988989109974185,
2.10454797952851));
#21752=CARTESIAN_POINT('Ctrl Pts',(-0.515186036985696,0.851781234675702,
2.09669742849084));
#21753=CARTESIAN_POINT('Ctrl Pts',(-0.67684923284346,0.847499648733552,
2.08884687745316));
#21754=CARTESIAN_POINT('Ctrl Pts',(-0.769592458789038,0.979983655714312,
2.08099632641548));
#21755=CARTESIAN_POINT('Ctrl Pts',(-0.710240646482644,1.1304194790008,2.0731457753778));
#21756=CARTESIAN_POINT('Ctrl Pts',(-0.552023363069014,1.16389067130903,
2.06529522434013));
#21757=CARTESIAN_POINT('Ctrl Pts',(-0.436830779225235,1.05038344926453,
2.05744467330245));
#21758=CARTESIAN_POINT('Ctrl Pts',(-0.467975943016225,0.891685973282426,
2.04959412226477));
#21759=CARTESIAN_POINT('Ctrl Pts',(-0.617516128195625,0.830137266366705,
2.04174357122709));
#21760=CARTESIAN_POINT('Ctrl Pts',(-0.751361759160267,0.920905505868468,
2.03389302018941));
#21761=CARTESIAN_POINT('Ctrl Pts',(-0.749434417417234,1.08264685459083,
2.02604246915173));
#21762=CARTESIAN_POINT('Ctrl Pts',(-0.613546069870597,1.17019124489367,
2.01819191811406));
#21763=CARTESIAN_POINT('Ctrl Pts',(-0.465400250310609,1.10525715548948,
2.01034136707638));
#21764=CARTESIAN_POINT('Ctrl Pts',(-0.438184538961436,0.945611677663771,
2.0024908160387));
#21765=CARTESIAN_POINT('Ctrl Pts',(-0.516476448777932,0.872219838026411,
1.99725711534692));
#21766=CARTESIAN_POINT('Ctrl Pts',(-0.56254624175848,0.859903427576914,
1.99464026500102));
#21767=CARTESIAN_POINT('Ctrl Pts',(-0.483086340557485,1.10069600903591,
2.41607920499693));
#21768=CARTESIAN_POINT('Ctrl Pts',(-0.449973151490718,1.0622497573257,2.41346235465104));
#21769=CARTESIAN_POINT('Ctrl Pts',(-0.42515130434576,0.950798154359666,
2.40822865395925));
#21770=CARTESIAN_POINT('Ctrl Pts',(-0.54478524831763,0.826780024693742,
2.40037810292158));
#21771=CARTESIAN_POINT('Ctrl Pts',(-0.71394018522848,0.858516547958849,
2.3925275518839));
#21772=CARTESIAN_POINT('Ctrl Pts',(-0.780906780829043,1.01693886792356,
2.38467700084622));
#21773=CARTESIAN_POINT('Ctrl Pts',(-0.685634174422424,1.16027112587027,
2.37682644980854));
#21774=CARTESIAN_POINT('Ctrl Pts',(-0.513561613772921,1.15981701793772,
2.36897589877087));
#21775=CARTESIAN_POINT('Ctrl Pts',(-0.419009660745144,1.01606137072615,
2.36112534773318));
#21776=CARTESIAN_POINT('Ctrl Pts',(-0.486773837186857,0.857888188850051,
2.35327479669551));
#21777=CARTESIAN_POINT('Ctrl Pts',(-0.656082085820325,0.827171035125292,
2.34542424565783));
#21778=CARTESIAN_POINT('Ctrl Pts',(-0.775094506405975,0.951447556274721,
2.33757369462015));
#21779=CARTESIAN_POINT('Ctrl Pts',(-0.737078051838477,1.11926881902364,
2.32972314358247));
#21780=CARTESIAN_POINT('Ctrl Pts',(-0.576126720758545,1.18012607574093,
2.3218725925448));
#21781=CARTESIAN_POINT('Ctrl Pts',(-0.436585524633584,1.079442440351,2.31402204150712));
#21782=CARTESIAN_POINT('Ctrl Pts',(-0.443598309590693,0.907512704295987,
2.30617149046944));
#21783=CARTESIAN_POINT('Ctrl Pts',(-0.59087585148424,0.818527891629664,
2.29832093943176));
#21784=CARTESIAN_POINT('Ctrl Pts',(-0.746336145286304,0.892291520022432,
2.29047038839408));
#21785=CARTESIAN_POINT('Ctrl Pts',(-0.77055870576274,1.06265070441055,2.28261983735641));
#21786=CARTESIAN_POINT('Ctrl Pts',(-0.641820163748749,1.17682323210921,
2.27476928631873));
#21787=CARTESIAN_POINT('Ctrl Pts',(-0.47557630485125,1.13241648942973,2.26691873528105));
#21788=CARTESIAN_POINT('Ctrl Pts',(-0.420918573673669,0.969255486982105,
2.25906818424337));
#21789=CARTESIAN_POINT('Ctrl Pts',(-0.526865323090207,0.833666896767115,
2.2512176332057));
#21790=CARTESIAN_POINT('Ctrl Pts',(-0.698400989412974,0.847249786831145,
2.24336708216802));
#21791=CARTESIAN_POINT('Ctrl Pts',(-0.781688309092209,0.997822700025263,
2.23551653113034));
#21792=CARTESIAN_POINT('Ctrl Pts',(-0.702033233780365,1.15034826732694,
2.22766598009266));
#21793=CARTESIAN_POINT('Ctrl Pts',(-0.530872328713473,1.16803793430571,
2.21981542905499));
#21794=CARTESIAN_POINT('Ctrl Pts',(-0.421706762676398,1.0350271868484,2.2119648780173));
#21795=CARTESIAN_POINT('Ctrl Pts',(-0.472438810540477,0.870603225552124,
2.20411432697963));
#21796=CARTESIAN_POINT('Ctrl Pts',(-0.637570765725878,0.822225367765818,
2.19626377594195));
#21797=CARTESIAN_POINT('Ctrl Pts',(-0.769008364973917,0.933280026583224,
2.18841322490427));
#21798=CARTESIAN_POINT('Ctrl Pts',(-0.748875244649484,1.10417074362085,
2.18056267386659));
#21799=CARTESIAN_POINT('Ctrl Pts',(-0.595227265459685,1.1816386614837,2.17271212282892));
#21800=CARTESIAN_POINT('Ctrl Pts',(-0.445859588380167,1.09620870908317,
2.16486157179124));
#21801=CARTESIAN_POINT('Ctrl Pts',(-0.434728696312199,0.924496499994273,
2.15701102075356));
#21802=CARTESIAN_POINT('Ctrl Pts',(-0.571817039685625,0.820497623037239,
2.14916046971588));
#21803=CARTESIAN_POINT('Ctrl Pts',(-0.734180529534971,0.877480748438312,
2.14130991867821));
#21804=CARTESIAN_POINT('Ctrl Pts',(-0.776207735146129,1.04434204493786,
2.13345936764052));
#21805=CARTESIAN_POINT('Ctrl Pts',(-0.660207645725328,1.17143635399922,
2.12560881660285));
#21806=CARTESIAN_POINT('Ctrl Pts',(-0.490211926051119,1.14478244030651,
2.11775826556517));
#21807=CARTESIAN_POINT('Ctrl Pts',(-0.418676726208604,0.988284240908056,
2.10990771452749));
#21808=CARTESIAN_POINT('Ctrl Pts',(-0.509756617677689,0.842292916978238,
2.10205716348981));
#21809=CARTESIAN_POINT('Ctrl Pts',(-0.681768784928714,0.837737242612945,
2.09420661245213));
#21810=CARTESIAN_POINT('Ctrl Pts',(-0.780449026947353,0.978702296816814,
2.08635606141446));
#21811=CARTESIAN_POINT('Ctrl Pts',(-0.717297770961535,1.13876836416382,
2.07850551037678));
#21812=CARTESIAN_POINT('Ctrl Pts',(-0.548952108412014,1.17438223594748,
2.0706549593391));
#21813=CARTESIAN_POINT('Ctrl Pts',(-0.426385398697532,1.05360877753029,
2.06280440830142));
#21814=CARTESIAN_POINT('Ctrl Pts',(-0.459524339782119,0.884752182582313,
2.05495385726375));
#21815=CARTESIAN_POINT('Ctrl Pts',(-0.618637434184013,0.819263396393857,
2.04710330622607));
#21816=CARTESIAN_POINT('Ctrl Pts',(-0.761051277589445,0.915842221966472,
2.03925275518839));
#21817=CARTESIAN_POINT('Ctrl Pts',(-0.759000555849758,1.08793754508699,
2.03140220415071));
#21818=CARTESIAN_POINT('Ctrl Pts',(-0.614413230072635,1.18108614472194,
2.02355165311304));
#21819=CARTESIAN_POINT('Ctrl Pts',(-0.456783762484268,1.11199525865091,
2.01570110207535));
#21820=CARTESIAN_POINT('Ctrl Pts',(-0.427825820216639,0.942129974923708,
2.00785055103768));
#21821=CARTESIAN_POINT('Ctrl Pts',(-0.511129635994264,0.864039910406679,
2.00261685034589));
#21822=CARTESIAN_POINT('Ctrl Pts',(-0.560148615814275,0.850935057178149,
2.));
#21823=CARTESIAN_POINT('Ctrl Pts',(-0.560148615814275,0.850935057178149,
2.));
#21824=CARTESIAN_POINT('Ctrl Pts',(-0.550119441743087,0.85459967610481,
2.));
#21825=CARTESIAN_POINT('Ctrl Pts',(-0.540564999899567,0.859362631836586,
2.));
#21826=CARTESIAN_POINT('Ctrl Pts',(-0.531596825272739,0.86507409197529,
2.));
#21827=CARTESIAN_POINT('Ctrl Pts',(-0.527131635014649,0.867917787290334,
2.));
#21828=CARTESIAN_POINT('Ctrl Pts',(-0.522812202969371,0.870997335784893,
2.));
#21829=CARTESIAN_POINT('Ctrl Pts',(-0.518655551555349,0.874297548143145,
2.));
#21830=CARTESIAN_POINT('Ctrl Pts',(-0.515850210886717,0.876524874666724,
2.));
#21831=CARTESIAN_POINT('Ctrl Pts',(-0.51311906464033,0.878852752659134,
2.));
#21832=CARTESIAN_POINT('Ctrl Pts',(-0.510468070497139,0.881276854651557,
2.));
#21833=CARTESIAN_POINT('Ctrl Pts',(-0.508096882944962,0.883445098019579,
2.));
#21834=CARTESIAN_POINT('Ctrl Pts',(-0.505796523707934,0.885684247113283,
2.));
#21835=CARTESIAN_POINT('Ctrl Pts',(-0.503571407093493,0.887989067169883,
2.));
#21836=CARTESIAN_POINT('Ctrl Pts',(-0.496344337828248,0.895475009293033,
2.));
#21837=CARTESIAN_POINT('Ctrl Pts',(-0.489902887206981,0.90365635994166,
2.));
#21838=CARTESIAN_POINT('Ctrl Pts',(-0.4843803033401,0.912413093858066,2.));
#21839=CARTESIAN_POINT('Ctrl Pts',(-0.482085852075076,0.91605122769112,
2.));
#21840=CARTESIAN_POINT('Ctrl Pts',(-0.479950567463666,0.919788922535331,
2.));
#21841=CARTESIAN_POINT('Ctrl Pts',(-0.477986666560954,0.923618208076587,
2.));
#21842=CARTESIAN_POINT('Ctrl Pts',(-0.47650289740366,0.926511315245457,
2.));
#21843=CARTESIAN_POINT('Ctrl Pts',(-0.475117210175375,0.929457020402162,
2.));
#21844=CARTESIAN_POINT('Ctrl Pts',(-0.473840374763333,0.932438174193855,
2.));
#21845=CARTESIAN_POINT('Ctrl Pts',(-0.470678071962382,0.939821514988315,
2.));
#21846=CARTESIAN_POINT('Ctrl Pts',(-0.468171074744705,0.947441922900028,
2.));
#21847=CARTESIAN_POINT('Ctrl Pts',(-0.466390213028648,0.95524361805541,
2.));
#21848=CARTESIAN_POINT('Ctrl Pts',(-0.464752059680358,0.962420128688376,
2.));
#21849=CARTESIAN_POINT('Ctrl Pts',(-0.463728780577517,0.969750541677906,
2.));
#21850=CARTESIAN_POINT('Ctrl Pts',(-0.463308983993722,0.977159407672611,
2.));
#21851=CARTESIAN_POINT('Ctrl Pts',(-0.46313283978449,0.9802681248283,2.));
#21852=CARTESIAN_POINT('Ctrl Pts',(-0.463063521137214,0.983387155046876,
2.));
#21853=CARTESIAN_POINT('Ctrl Pts',(-0.463099420187341,0.986501027428933,
2.));
#21854=CARTESIAN_POINT('Ctrl Pts',(-0.463196744049792,0.994942868824082,
2.));
#21855=CARTESIAN_POINT('Ctrl Pts',(-0.464064111260558,1.00336874731576,
2.));
#21856=CARTESIAN_POINT('Ctrl Pts',(-0.465675457037548,1.01166504030789,
2.));
#21857=CARTESIAN_POINT('Ctrl Pts',(-0.466871286975471,1.01782197799031,
2.));
#21858=CARTESIAN_POINT('Ctrl Pts',(-0.468477483228933,1.02390757245997,
2.));
#21859=CARTESIAN_POINT('Ctrl Pts',(-0.47049180892072,1.02987016754483,2.));
#21860=CARTESIAN_POINT('Ctrl Pts',(-0.471677004317114,1.03337845832122,
2.));
#21861=CARTESIAN_POINT('Ctrl Pts',(-0.473001297362186,1.03683670978256,
2.));
#21862=CARTESIAN_POINT('Ctrl Pts',(-0.474460925722079,1.04022912201569,
2.));
#21863=CARTESIAN_POINT('Ctrl Pts',(-0.476751357662528,1.04555245605566,
2.));
#21864=CARTESIAN_POINT('Ctrl Pts',(-0.479376312983413,1.05071850549913,
2.));
#21865=CARTESIAN_POINT('Ctrl Pts',(-0.482333055615295,1.05568494193306,
2.));
#21866=CARTESIAN_POINT('Ctrl Pts',(-0.484374509820886,1.05911396968661,
2.));
#21867=CARTESIAN_POINT('Ctrl Pts',(-0.486574680171624,1.06244757845398,
2.));
#21868=CARTESIAN_POINT('Ctrl Pts',(-0.488924280031899,1.0656592034053,2.));
#21869=CARTESIAN_POINT('Ctrl Pts',(-0.492216707647991,1.07015956232216,
2.));
#21870=CARTESIAN_POINT('Ctrl Pts',(-0.495805970213506,1.07442716727356,
2.));
#21871=CARTESIAN_POINT('Ctrl Pts',(-0.499690940637682,1.07842077494232,
2.));
#21872=CARTESIAN_POINT('Ctrl Pts',(-0.501092717011139,1.07986174984398,
2.));
#21873=CARTESIAN_POINT('Ctrl Pts',(-0.502533033199793,1.08126699098065,
2.));
#21874=CARTESIAN_POINT('Ctrl Pts',(-0.504010174669742,1.08263575197434,
2.));
#21875=CARTESIAN_POINT('Ctrl Pts',(-0.504188384727764,1.08252112989365,
2.4));
#21876=CARTESIAN_POINT('Ctrl Pts',(-0.497506954663502,1.07628156217526,
2.4));
#21877=CARTESIAN_POINT('Ctrl Pts',(-0.491604269963233,1.06931033894935,
2.4));
#21878=CARTESIAN_POINT('Ctrl Pts',(-0.48648731081533,1.06178682142811,2.4));
#21879=CARTESIAN_POINT('Ctrl Pts',(-0.482497621478512,1.05592074027282,
2.4));
#21880=CARTESIAN_POINT('Ctrl Pts',(-0.478985885254584,1.04971755224006,
2.4));
#21881=CARTESIAN_POINT('Ctrl Pts',(-0.475968008505373,1.04324617240972,
2.4));
#21882=CARTESIAN_POINT('Ctrl Pts',(-0.474670784833122,1.04046447262352,
2.4));
#21883=CARTESIAN_POINT('Ctrl Pts',(-0.473467326409776,1.03763771123602,
2.4));
#21884=CARTESIAN_POINT('Ctrl Pts',(-0.472361166010358,1.03477908326479,
2.4));
#21885=CARTESIAN_POINT('Ctrl Pts',(-0.46880698586937,1.02559408733548,2.4));
#21886=CARTESIAN_POINT('Ctrl Pts',(-0.466243719906724,1.01606060675579,
2.4));
#21887=CARTESIAN_POINT('Ctrl Pts',(-0.464705314070165,1.00636042835626,
2.4));
#21888=CARTESIAN_POINT('Ctrl Pts',(-0.463992227392452,1.00186417137142,
2.4));
#21889=CARTESIAN_POINT('Ctrl Pts',(-0.463499928942431,0.997331640290426,
2.4));
#21890=CARTESIAN_POINT('Ctrl Pts',(-0.463235268916811,0.992779403524773,
2.4));
#21891=CARTESIAN_POINT('Ctrl Pts',(-0.463040851274643,0.989435358134849,
2.4));
#21892=CARTESIAN_POINT('Ctrl Pts',(-0.462969940004504,0.986088143884579,
2.4));
#21893=CARTESIAN_POINT('Ctrl Pts',(-0.463023793901296,0.982751466845985,
2.4));
#21894=CARTESIAN_POINT('Ctrl Pts',(-0.463137062422501,0.975733581485534,
2.4));
#21895=CARTESIAN_POINT('Ctrl Pts',(-0.463800894161501,0.968753185610107,
2.4));
#21896=CARTESIAN_POINT('Ctrl Pts',(-0.465031332332612,0.96187163776825,
2.4));
#21897=CARTESIAN_POINT('Ctrl Pts',(-0.466389645164331,0.954274917384296,
2.4));
#21898=CARTESIAN_POINT('Ctrl Pts',(-0.468438000905081,0.946798204321114,
2.4));
#21899=CARTESIAN_POINT('Ctrl Pts',(-0.471116528460654,0.93949859713407,
2.4));
#21900=CARTESIAN_POINT('Ctrl Pts',(-0.472251134057494,0.936406534425243,
2.4));
#21901=CARTESIAN_POINT('Ctrl Pts',(-0.473496260389133,0.933354194164882,
2.4));
#21902=CARTESIAN_POINT('Ctrl Pts',(-0.474844488633202,0.930349739998837,
2.4));
#21903=CARTESIAN_POINT('Ctrl Pts',(-0.478666411965482,0.9218327893056,2.4));
#21904=CARTESIAN_POINT('Ctrl Pts',(-0.4833179823867,0.913689872025069,2.4));
#21905=CARTESIAN_POINT('Ctrl Pts',(-0.488689869589499,0.906016299690457,
2.4));
#21906=CARTESIAN_POINT('Ctrl Pts',(-0.491565626713204,0.901908370861642,
2.4));
#21907=CARTESIAN_POINT('Ctrl Pts',(-0.494648453197326,0.897935009702848,
2.4));
#21908=CARTESIAN_POINT('Ctrl Pts',(-0.497925430586844,0.894112166139119,
2.4));
#21909=CARTESIAN_POINT('Ctrl Pts',(-0.500336511660046,0.89129945653917,
2.4));
#21910=CARTESIAN_POINT('Ctrl Pts',(-0.502853434868661,0.888568042774596,
2.4));
#21911=CARTESIAN_POINT('Ctrl Pts',(-0.505459753140441,0.885935602377086,
2.4));
#21912=CARTESIAN_POINT('Ctrl Pts',(-0.510032980818731,0.881316538996496,
2.4));
#21913=CARTESIAN_POINT('Ctrl Pts',(-0.514888373574847,0.876993017632294,
2.4));
#21914=CARTESIAN_POINT('Ctrl Pts',(-0.519995790255463,0.872997627556259,
2.4));
#21915=CARTESIAN_POINT('Ctrl Pts',(-0.524771384850184,0.869261812672909,
2.4));
#21916=CARTESIAN_POINT('Ctrl Pts',(-0.529772960099733,0.865810225418053,
2.4));
#21917=CARTESIAN_POINT('Ctrl Pts',(-0.534950219195867,0.86268896384257,
2.4));
#21918=CARTESIAN_POINT('Ctrl Pts',(-0.540826101062414,0.859146517163432,
2.4));
#21919=CARTESIAN_POINT('Ctrl Pts',(-0.546932707573367,0.85602468566073,
2.4));
#21920=CARTESIAN_POINT('Ctrl Pts',(-0.553238064171717,0.853364150883981,
2.4));
#21921=CARTESIAN_POINT('Ctrl Pts',(-0.555483414843566,0.852416728885673,
2.4));
#21922=CARTESIAN_POINT('Ctrl Pts',(-0.557754020887936,0.851527863380312,
2.4));
#21923=CARTESIAN_POINT('Ctrl Pts',(-0.560047768817924,0.850696978396871,
2.4));
#21924=CARTESIAN_POINT('Ctrl Pts',(-0.72640212307541,0.999893075304641,
2.31934196736194));
#21925=CARTESIAN_POINT('Ctrl Pts',(-0.726497678848041,0.988483569383442,
2.32005947478237));
#21926=CARTESIAN_POINT('Ctrl Pts',(-0.725076811113891,0.977097445695636,
2.32077698220279));
#21927=CARTESIAN_POINT('Ctrl Pts',(-0.722043530727044,0.966158450551832,
2.32149448962322));
#21928=CARTESIAN_POINT('Ctrl Pts',(-0.710980731091059,0.926262398732923,
2.32411133996911));
#21929=CARTESIAN_POINT('Ctrl Pts',(-0.678470209200682,0.892313886960735,
2.32672819031501));
#21930=CARTESIAN_POINT('Ctrl Pts',(-0.639090052986859,0.879535120476776,
2.3293450406609));
#21931=CARTESIAN_POINT('Ctrl Pts',(-0.599709896773035,0.866756353992817,
2.33196189100679));
#21932=CARTESIAN_POINT('Ctrl Pts',(-0.553460106235766,0.875147332797086,
2.33457874135268));
#21933=CARTESIAN_POINT('Ctrl Pts',(-0.52107966969358,0.900946839101611,
2.33719559169858));
#21934=CARTESIAN_POINT('Ctrl Pts',(-0.488699233151393,0.926746345406136,
2.33981244204447));
#21935=CARTESIAN_POINT('Ctrl Pts',(-0.470188150604288,0.969954379210915,
2.34242929239036));
#21936=CARTESIAN_POINT('Ctrl Pts',(-0.473846947697945,1.01119320016375,
2.34504614273626));
#21937=CARTESIAN_POINT('Ctrl Pts',(-0.477505744791602,1.05243202111659,
2.34766299308215));
#21938=CARTESIAN_POINT('Ctrl Pts',(-0.503334421526021,1.09170162921748,
2.35027984342804));
#21939=CARTESIAN_POINT('Ctrl Pts',(-0.539751217545131,1.11139845740712,
2.35289669377393));
#21940=CARTESIAN_POINT('Ctrl Pts',(-0.576168013564241,1.13109528559677,
2.35551354411982));
#21941=CARTESIAN_POINT('Ctrl Pts',(-0.623172928868043,1.13121933387517,
2.35813039446572));
#21942=CARTESIAN_POINT('Ctrl Pts',(-0.659688155022986,1.11170438240693,
2.36074724481161));
#21943=CARTESIAN_POINT('Ctrl Pts',(-0.696203381177929,1.0921894309387,2.3633640951575));
#21944=CARTESIAN_POINT('Ctrl Pts',(-0.722228918184014,1.05303547972384,
2.3659809455034));
#21945=CARTESIAN_POINT('Ctrl Pts',(-0.726095082654122,1.01182045879394,
2.36859779584929));
#21946=CARTESIAN_POINT('Ctrl Pts',(-0.726461565140266,1.00791359361693,
2.36884585302017));
#21947=CARTESIAN_POINT('Ctrl Pts',(-0.726628932956602,1.00398820854659,
2.36909391019106));
#21948=CARTESIAN_POINT('Ctrl Pts',(-0.726604172280256,1.00006079745576,
2.36934196736194));
#21949=CARTESIAN_POINT('Ctrl Pts',(-0.639851384185722,0.850935057178148,
2.4));
#21950=CARTESIAN_POINT('Ctrl Pts',(-0.688870364005733,0.864039910406677,
2.39738314965411));
#21951=CARTESIAN_POINT('Ctrl Pts',(-0.772174172732383,0.942130018479807,
2.39214944896232));
#21952=CARTESIAN_POINT('Ctrl Pts',(-0.743216243669936,1.11199523763249,
2.38429889792464));
#21953=CARTESIAN_POINT('Ctrl Pts',(-0.585586769094172,1.18108616109394,
2.37644834688697));
#21954=CARTESIAN_POINT('Ctrl Pts',(-0.44099944093888,1.08793753892263,2.36859779584929));
#21955=CARTESIAN_POINT('Ctrl Pts',(-0.438948720197302,0.915842224941729,
2.36074724481161));
#21956=CARTESIAN_POINT('Ctrl Pts',(-0.581362564989717,0.819263390701727,
2.35289669377393));
#21957=CARTESIAN_POINT('Ctrl Pts',(-0.740475663026546,0.88475218199663,
2.34504614273626));
#21958=CARTESIAN_POINT('Ctrl Pts',(-0.773614604105453,1.05360877766967,
2.33719559169858));
#21959=CARTESIAN_POINT('Ctrl Pts',(-0.651047892623131,1.17438223943631,
2.3293450406609));
#21960=CARTESIAN_POINT('Ctrl Pts',(-0.48270222690289,1.13876836634555,2.32149448962322));
#21961=CARTESIAN_POINT('Ctrl Pts',(-0.419550969949932,0.978702296577685,
2.31364393858554));
#21962=CARTESIAN_POINT('Ctrl Pts',(-0.518231213613428,0.837737239705173,
2.30579338754787));
#21963=CARTESIAN_POINT('Ctrl Pts',(-0.690243383915708,0.842292914261777,
2.29794283651019));
#21964=CARTESIAN_POINT('Ctrl Pts',(-0.781323276950512,0.988284240682119,
2.29009228547251));
#21965=CARTESIAN_POINT('Ctrl Pts',(-0.709788075872465,1.14478244284782,
2.28224173443483));
#21966=CARTESIAN_POINT('Ctrl Pts',(-0.539792353219763,1.17143635698873,
2.27439118339715));
#21967=CARTESIAN_POINT('Ctrl Pts',(-0.423792261776434,1.04434204571596,
2.26654063235948));
#21968=CARTESIAN_POINT('Ctrl Pts',(-0.465819468119529,0.877480746295693,
2.2586900813218));
#21969=CARTESIAN_POINT('Ctrl Pts',(-0.6281829608073,0.820497619901593,2.25083953028412));
#21970=CARTESIAN_POINT('Ctrl Pts',(-0.765271306575456,0.924496498674441,
2.24298897924644));
#21971=CARTESIAN_POINT('Ctrl Pts',(-0.754140414313383,1.09620871076456,
2.23513842820876));
#21972=CARTESIAN_POINT('Ctrl Pts',(-0.604772734623643,1.18163866465747,
2.22728787717109));
#21973=CARTESIAN_POINT('Ctrl Pts',(-0.451124752749149,1.10417074544119,
2.21943732613341));
#21974=CARTESIAN_POINT('Ctrl Pts',(-0.43099163207285,0.933280025417337,
2.21158677509573));
#21975=CARTESIAN_POINT('Ctrl Pts',(-0.562429233617627,0.822225364659454,
2.20373622405805));
#21976=CARTESIAN_POINT('Ctrl Pts',(-0.727561191688486,0.870603223291056,
2.19588567302038));
#21977=CARTESIAN_POINT('Ctrl Pts',(-0.778293240439059,1.03502718746047,
2.1880351219827));
#21978=CARTESIAN_POINT('Ctrl Pts',(-0.669127672494447,1.16803793724193,
2.18018457094502));
#21979=CARTESIAN_POINT('Ctrl Pts',(-0.497966764436741,1.15034826995414,
2.17233401990734));
#21980=CARTESIAN_POINT('Ctrl Pts',(-0.418311687733005,0.997822699987136,
2.16448346886966));
#21981=CARTESIAN_POINT('Ctrl Pts',(-0.501599008867606,0.847249784162188,
2.15663291783199));
#21982=CARTESIAN_POINT('Ctrl Pts',(-0.673134678187691,0.833666893860354,
2.1487823667943));
#21983=CARTESIAN_POINT('Ctrl Pts',(-0.779081429455625,0.969255486445431,
2.14093181575663));
#21984=CARTESIAN_POINT('Ctrl Pts',(-0.724423697322763,1.1324164917425,2.13308126471895));
#21985=CARTESIAN_POINT('Ctrl Pts',(-0.558179835520779,1.17682323520091,
2.12523071368127));
#21986=CARTESIAN_POINT('Ctrl Pts',(-0.429441291256411,1.0626507055017,2.1173801626436));
#21987=CARTESIAN_POINT('Ctrl Pts',(-0.453663852157743,0.892291518147041,
2.10952961160592));
#21988=CARTESIAN_POINT('Ctrl Pts',(-0.609124148673025,0.818527888446316,
2.10167906056824));
#21989=CARTESIAN_POINT('Ctrl Pts',(-0.756401693146515,0.907512702702641,
2.09382850953056));
#21990=CARTESIAN_POINT('Ctrl Pts',(-0.763414478213392,1.07944244169741,
2.08597795849288));
#21991=CARTESIAN_POINT('Ctrl Pts',(-0.623873279675432,1.18012607896462,
2.0781274074552));
#21992=CARTESIAN_POINT('Ctrl Pts',(-0.462921945732953,1.11926882096942,
2.07027685641753));
#21993=CARTESIAN_POINT('Ctrl Pts',(-0.424905490600427,0.951447555675582,
2.06242630537985));
#21994=CARTESIAN_POINT('Ctrl Pts',(-0.54391791306908,0.827171031659744,
2.05457575434217));
#21995=CARTESIAN_POINT('Ctrl Pts',(-0.713226165050295,0.857888187155562,
2.04672520330449));
#21996=CARTESIAN_POINT('Ctrl Pts',(-0.780990341905239,1.01606136962747,
2.03887465226682));
#21997=CARTESIAN_POINT('Ctrl Pts',(-0.686438388751686,1.15981702310584,
2.03102410122914));
#21998=CARTESIAN_POINT('Ctrl Pts',(-0.514365822072695,1.16027112465931,
2.02317355019146));
#21999=CARTESIAN_POINT('Ctrl Pts',(-0.41909321999119,1.01693887482571,2.01532299915378));
#22000=CARTESIAN_POINT('Ctrl Pts',(-0.486059804858393,0.858516534902566,
2.0074724481161));
#22001=CARTESIAN_POINT('Ctrl Pts',(-0.655214768609463,0.826780038590561,
1.99962189707843));
#22002=CARTESIAN_POINT('Ctrl Pts',(-0.774848665287453,0.950798122348591,
1.99177134604075));
#22003=CARTESIAN_POINT('Ctrl Pts',(-0.750026848509283,1.0622497573257,1.98653764534896));
#22004=CARTESIAN_POINT('Ctrl Pts',(-0.716913659442517,1.10069600903591,
1.98392079500307));
#22005=CARTESIAN_POINT('Ctrl Pts',(-0.637453758241517,0.859903427576914,
2.40535973499898));
#22006=CARTESIAN_POINT('Ctrl Pts',(-0.683523551222066,0.872219838026409,
2.40274288465309));
#22007=CARTESIAN_POINT('Ctrl Pts',(-0.761815454411802,0.945611718599352,
2.3975091839613));
#22008=CARTESIAN_POINT('Ctrl Pts',(-0.734599755473333,1.10525713573561,
2.38965863292362));
#22009=CARTESIAN_POINT('Ctrl Pts',(-0.586453929346337,1.17019126028066,
2.38180808188594));
#22010=CARTESIAN_POINT('Ctrl Pts',(-0.450565579564614,1.08264684879734,
2.37395753084827));
#22011=CARTESIAN_POINT('Ctrl Pts',(-0.448638238759637,0.920905508664721,
2.36610697981058));
#22012=CARTESIAN_POINT('Ctrl Pts',(-0.582483871027817,0.830137261017037,
2.35825642877291));
#22013=CARTESIAN_POINT('Ctrl Pts',(-0.732024059623459,0.891685972731981,
2.35040587773523));
#22014=CARTESIAN_POINT('Ctrl Pts',(-0.76316922340911,1.05038344939552,2.34255532669756));
#22015=CARTESIAN_POINT('Ctrl Pts',(-0.647976637903853,1.16389067458796,
2.33470477565988));
#22016=CARTESIAN_POINT('Ctrl Pts',(-0.489759351510266,1.13041948105126,
2.3268542246222));
#22017=CARTESIAN_POINT('Ctrl Pts',(-0.430407538294919,0.979983655489569,
2.31900367358452));
#22018=CARTESIAN_POINT('Ctrl Pts',(-0.523150765786394,0.847499646000726,
2.31115312254684));
#22019=CARTESIAN_POINT('Ctrl Pts',(-0.684813964511835,0.851781232122674,
2.30330257150917));
#22020=CARTESIAN_POINT('Ctrl Pts',(-0.770414110255606,0.98898910976184,
2.29545202047149));
#22021=CARTESIAN_POINT('Ctrl Pts',(-0.703182766058146,1.13607172555832,
2.28760146943381));
#22022=CARTESIAN_POINT('Ctrl Pts',(-0.543414697058237,1.16112202874907,
2.27975091839613));
#22023=CARTESIAN_POINT('Ctrl Pts',(-0.434393656266662,1.04167424279268,
2.27190036735845));
#22024=CARTESIAN_POINT('Ctrl Pts',(-0.47389233010456,0.884852017014347,
2.26404981632077));
#22025=CARTESIAN_POINT('Ctrl Pts',(-0.626487356014725,0.831297233826287,
2.2561992652831));
#22026=CARTESIAN_POINT('Ctrl Pts',(-0.755327893552931,0.929039105094654,
2.24834871424542));
#22027=CARTESIAN_POINT('Ctrl Pts',(-0.744866682322397,1.0904203923485,2.24049816320774));
#22028=CARTESIAN_POINT('Ctrl Pts',(-0.604485586947538,1.17071052291906,
2.23264761217006));
#22029=CARTESIAN_POINT('Ctrl Pts',(-0.460081710268994,1.09790339771914,
2.22479706113239));
#22030=CARTESIAN_POINT('Ctrl Pts',(-0.441159882335912,0.937294178133102,
2.21694651009471));
#22031=CARTESIAN_POINT('Ctrl Pts',(-0.564689648056489,0.832921030233517,
2.20909595905703));
#22032=CARTESIAN_POINT('Ctrl Pts',(-0.719886576893662,0.878388274557731,
2.20124540801935));
#22033=CARTESIAN_POINT('Ctrl Pts',(-0.767566373413291,1.03291980536764,
2.19339485698167));
#22034=CARTESIAN_POINT('Ctrl Pts',(-0.664968662602526,1.15792807214755,
2.185544305944));
#22035=CARTESIAN_POINT('Ctrl Pts',(-0.504105510624766,1.1413026892278,2.17769375490632));
#22036=CARTESIAN_POINT('Ctrl Pts',(-0.429242816479248,0.997953695462094,
2.16984320386864));
#22037=CARTESIAN_POINT('Ctrl Pts',(-0.50751922403943,0.856439875998617,
2.16199265283096));
#22038=CARTESIAN_POINT('Ctrl Pts',(-0.668734590074648,0.843674189185456,
2.15414210179328));
#22039=CARTESIAN_POINT('Ctrl Pts',(-0.768307141682156,0.971105204964537,
2.14629155075561));
#22040=CARTESIAN_POINT('Ctrl Pts',(-0.716937847311012,1.12444976178997,
2.13844099971793));
#22041=CARTESIAN_POINT('Ctrl Pts',(-0.560695911521528,1.16618480983832,
2.13059044868025));
#22042=CARTESIAN_POINT('Ctrl Pts',(-0.439702816507024,1.05888137703287,
2.12273989764257));
#22043=CARTESIAN_POINT('Ctrl Pts',(-0.462468046837819,0.8987717108876,2.11488934660489));
#22044=CARTESIAN_POINT('Ctrl Pts',(-0.608575201728667,0.829446009653423,
2.10703879556722));
#22045=CARTESIAN_POINT('Ctrl Pts',(-0.746991913163515,0.913077125320336,
2.09918824452953));
#22046=CARTESIAN_POINT('Ctrl Pts',(-0.753582779750997,1.07466285215048,
2.09133769349186));
#22047=CARTESIAN_POINT('Ctrl Pts',(-0.622436963324253,1.16928894070762,
2.08348714245418));
#22048=CARTESIAN_POINT('Ctrl Pts',(-0.471169134783152,1.11209310987848,
2.07563659141651));
#22049=CARTESIAN_POINT('Ctrl Pts',(-0.435439908588715,0.954368673788424,
2.06778604037882));
#22050=CARTESIAN_POINT('Ctrl Pts',(-0.547292045972571,0.837569145222665,
2.05993548934115));
#22051=CARTESIAN_POINT('Ctrl Pts',(-0.706414005411818,0.866438228174611,
2.05208493830347));
#22052=CARTESIAN_POINT('Ctrl Pts',(-0.770101205975101,1.01509505045675,
2.04423438726579));
#22053=CARTESIAN_POINT('Ctrl Pts',(-0.681237893770622,1.15020176258845,
2.03638383622811));
#22054=CARTESIAN_POINT('Ctrl Pts',(-0.519517932367091,1.15062854349327,
2.02853328519044));
#22055=CARTESIAN_POINT('Ctrl Pts',(-0.429977328488155,1.01591976127225,
2.02068273415276));
#22056=CARTESIAN_POINT('Ctrl Pts',(-0.492914923533471,0.867028771893199,
2.01283218311508));
#22057=CARTESIAN_POINT('Ctrl Pts',(-0.651892817203601,0.837201675931786,
2.0049816320774));
#22058=CARTESIAN_POINT('Ctrl Pts',(-0.764329038309151,0.95375831308653,
1.99713108103972));
#22059=CARTESIAN_POINT('Ctrl Pts',(-0.741000605841356,1.05850455157603,
1.99189738034794));
#22060=CARTESIAN_POINT('Ctrl Pts',(-0.709879644719091,1.09463771598849,
1.98928053000205));
#22061=CARTESIAN_POINT('Ctrl Pts',(-0.635056132297313,0.868871797975679,
2.41071946999795));
#22062=CARTESIAN_POINT('Ctrl Pts',(-0.678176738438398,0.880399765646142,
2.40810261965206));
#22063=CARTESIAN_POINT('Ctrl Pts',(-0.751456736091222,0.949093418718895,
2.40286891896028));
#22064=CARTESIAN_POINT('Ctrl Pts',(-0.725983267276729,1.09851903383873,
2.3950183679226));
#22065=CARTESIAN_POINT('Ctrl Pts',(-0.587321089598503,1.15929635946738,
2.38716781688492));
#22066=CARTESIAN_POINT('Ctrl Pts',(-0.460131718190347,1.07735615867206,
2.37931726584724));
#22067=CARTESIAN_POINT('Ctrl Pts',(-0.458327757321973,0.925968792387711,
2.37146671480957));
#22068=CARTESIAN_POINT('Ctrl Pts',(-0.583605177065917,0.841011131332347,
2.36361616377189));
#22069=CARTESIAN_POINT('Ctrl Pts',(-0.72357245622037,0.898619763467331,
2.35576561273421));
#22070=CARTESIAN_POINT('Ctrl Pts',(-0.752723842712768,1.04715812112138,
2.34791506169653));
#22071=CARTESIAN_POINT('Ctrl Pts',(-0.644905383184573,1.15339910973961,
2.34006451065885));
#22072=CARTESIAN_POINT('Ctrl Pts',(-0.496816476117644,1.12207059575698,
2.33221395962118));
#22073=CARTESIAN_POINT('Ctrl Pts',(-0.441264106639905,0.981265014401455,
2.3243634085835));
#22074=CARTESIAN_POINT('Ctrl Pts',(-0.528070317959361,0.857262052296277,
2.31651285754582));
#22075=CARTESIAN_POINT('Ctrl Pts',(-0.679384545107962,0.861269549983572,
2.30866230650814));
#22076=CARTESIAN_POINT('Ctrl Pts',(-0.759504943560701,0.989693978841561,
2.30081175547046));
#22077=CARTESIAN_POINT('Ctrl Pts',(-0.696577456243827,1.12736100826881,
2.29296120443279));
#22078=CARTESIAN_POINT('Ctrl Pts',(-0.547037040896711,1.15080770050942,
2.28511065339511));
#22079=CARTESIAN_POINT('Ctrl Pts',(-0.444995050756889,1.03900643986939,
2.27726010235743));
#22080=CARTESIAN_POINT('Ctrl Pts',(-0.481965192089592,0.892223287733,2.26940955131975));
#22081=CARTESIAN_POINT('Ctrl Pts',(-0.624791751222149,0.842096847750981,
2.26155900028208));
#22082=CARTESIAN_POINT('Ctrl Pts',(-0.745384480530408,0.933581711514867,
2.2537084492444));
#22083=CARTESIAN_POINT('Ctrl Pts',(-0.735592950331409,1.08463207393244,
2.24585789820672));
#22084=CARTESIAN_POINT('Ctrl Pts',(-0.604198439271435,1.15978238118065,
2.23800734716904));
#22085=CARTESIAN_POINT('Ctrl Pts',(-0.469038667788838,1.09163604999709,
2.23015679613136));
#22086=CARTESIAN_POINT('Ctrl Pts',(-0.451328132598973,0.941308330848865,
2.22230624509368));
#22087=CARTESIAN_POINT('Ctrl Pts',(-0.56695006249535,0.843616695807582,
2.21445569405601));
#22088=CARTESIAN_POINT('Ctrl Pts',(-0.712211962098838,0.886173325824406,
2.20660514301833));
#22089=CARTESIAN_POINT('Ctrl Pts',(-0.756839506387522,1.0308124232748,2.19875459198065));
#22090=CARTESIAN_POINT('Ctrl Pts',(-0.660809652710606,1.14781820705317,
2.19090404094297));
#22091=CARTESIAN_POINT('Ctrl Pts',(-0.51024425681279,1.13225710850146,2.1830534899053));
#22092=CARTESIAN_POINT('Ctrl Pts',(-0.440173945225492,0.998084690937051,
2.17520293886762));
#22093=CARTESIAN_POINT('Ctrl Pts',(-0.513439439211253,0.865629967835047,
2.16735238782994));
#22094=CARTESIAN_POINT('Ctrl Pts',(-0.664334501961606,0.853681484510555,
2.15950183679226));
#22095=CARTESIAN_POINT('Ctrl Pts',(-0.757532853908686,0.972954923483646,
2.15165128575458));
#22096=CARTESIAN_POINT('Ctrl Pts',(-0.709451997299263,1.11648303183743,
2.1438007347169));
#22097=CARTESIAN_POINT('Ctrl Pts',(-0.563211987522275,1.15554638447572,
2.13595018367923));
#22098=CARTESIAN_POINT('Ctrl Pts',(-0.449964341757637,1.05511204856404,
2.12809963264155));
#22099=CARTESIAN_POINT('Ctrl Pts',(-0.471272241517894,0.905251903628159,
2.12024908160387));
#22100=CARTESIAN_POINT('Ctrl Pts',(-0.608026254784307,0.840364130860531,
2.11239853056619));
#22101=CARTESIAN_POINT('Ctrl Pts',(-0.737582133180516,0.918641547938033,
2.10454797952851));
#22102=CARTESIAN_POINT('Ctrl Pts',(-0.7437510812886,1.06988326260355,2.09669742849084));
#22103=CARTESIAN_POINT('Ctrl Pts',(-0.621000646973074,1.15845180245062,
2.08884687745316));
#22104=CARTESIAN_POINT('Ctrl Pts',(-0.479416323833351,1.10491739878753,
2.08099632641548));
#22105=CARTESIAN_POINT('Ctrl Pts',(-0.445974326577002,0.957289791901268,
2.0731457753778));
#22106=CARTESIAN_POINT('Ctrl Pts',(-0.550666178876061,0.847967258785586,
2.06529522434013));
#22107=CARTESIAN_POINT('Ctrl Pts',(-0.699601845773343,0.87498826919366,
2.05744467330245));
#22108=CARTESIAN_POINT('Ctrl Pts',(-0.759212070044963,1.01412873128603,
2.04959412226477));
#22109=CARTESIAN_POINT('Ctrl Pts',(-0.676037398789558,1.14058650207107,
2.04174357122709));
#22110=CARTESIAN_POINT('Ctrl Pts',(-0.524670042661485,1.14098596232722,
2.03389302018941));
#22111=CARTESIAN_POINT('Ctrl Pts',(-0.440861436985121,1.01490064771879,
2.02604246915174));
#22112=CARTESIAN_POINT('Ctrl Pts',(-0.49977004220855,0.875541008883831,
2.01819191811406));
#22113=CARTESIAN_POINT('Ctrl Pts',(-0.648570865797738,0.847623313273011,
2.01034136707638));
#22114=CARTESIAN_POINT('Ctrl Pts',(-0.753809411330851,0.956718503824468,
2.0024908160387));
#22115=CARTESIAN_POINT('Ctrl Pts',(-0.731974363173429,1.05475934582637,
1.99725711534692));
#22116=CARTESIAN_POINT('Ctrl Pts',(-0.702845629995664,1.08857942294107,
1.99464026500102));
#22117=CARTESIAN_POINT('Ctrl Pts',(-0.632658506353108,0.877840168374445,
2.41607920499693));
#22118=CARTESIAN_POINT('Ctrl Pts',(-0.672829925654731,0.888579693265874,
2.41346235465104));
#22119=CARTESIAN_POINT('Ctrl Pts',(-0.74109801777064,0.952575118838442,
2.40822865395925));
#22120=CARTESIAN_POINT('Ctrl Pts',(-0.717366779080126,1.09178093194185,
2.40037810292158));
#22121=CARTESIAN_POINT('Ctrl Pts',(-0.588188249850668,1.1484014586541,2.3925275518839));
#22122=CARTESIAN_POINT('Ctrl Pts',(-0.469697856816082,1.07206546854677,
2.38467700084622));
#22123=CARTESIAN_POINT('Ctrl Pts',(-0.468017275884308,0.931032076110704,
2.37682644980854));
#22124=CARTESIAN_POINT('Ctrl Pts',(-0.584726483104016,0.851885001647656,
2.36897589877086));
#22125=CARTESIAN_POINT('Ctrl Pts',(-0.715120852817283,0.905553554202683,
2.36112534773319));
#22126=CARTESIAN_POINT('Ctrl Pts',(-0.742278462016426,1.04393279284724,
2.35327479669551));
#22127=CARTESIAN_POINT('Ctrl Pts',(-0.641834128465295,1.14290754489126,
2.34542424565783));
#22128=CARTESIAN_POINT('Ctrl Pts',(-0.50387360072502,1.1137217104627,2.33757369462015));
#22129=CARTESIAN_POINT('Ctrl Pts',(-0.452120674984892,0.98254637331334,
2.32972314358248));
#22130=CARTESIAN_POINT('Ctrl Pts',(-0.532989870132326,0.867024458591828,
2.32187259254479));
#22131=CARTESIAN_POINT('Ctrl Pts',(-0.673955125704091,0.870757867844471,
2.31402204150712));
#22132=CARTESIAN_POINT('Ctrl Pts',(-0.748595776865795,0.990398847921281,
2.30617149046944));
#22133=CARTESIAN_POINT('Ctrl Pts',(-0.689972146429509,1.11865029097931,
2.29832093943176));
#22134=CARTESIAN_POINT('Ctrl Pts',(-0.550659384735185,1.14049337226976,
2.29047038839408));
#22135=CARTESIAN_POINT('Ctrl Pts',(-0.455596445247116,1.0363386369461,2.28261983735641));
#22136=CARTESIAN_POINT('Ctrl Pts',(-0.490038054074624,0.899594558451655,
2.27476928631873));
#22137=CARTESIAN_POINT('Ctrl Pts',(-0.623096146429573,0.852896461675674,
2.26691873528105));
#22138=CARTESIAN_POINT('Ctrl Pts',(-0.735441067507883,0.938124317935081,
2.25906818424337));
#22139=CARTESIAN_POINT('Ctrl Pts',(-0.726319218340423,1.07884375551639,
2.25121763320569));
#22140=CARTESIAN_POINT('Ctrl Pts',(-0.603911291595331,1.14885423944223,
2.24336708216802));
#22141=CARTESIAN_POINT('Ctrl Pts',(-0.477995625308683,1.08536870227504,
2.23551653113034));
#22142=CARTESIAN_POINT('Ctrl Pts',(-0.461496382862034,0.945322483564629,
2.22766598009266));
#22143=CARTESIAN_POINT('Ctrl Pts',(-0.569210476934212,0.854312361381646,
2.21981542905498));
#22144=CARTESIAN_POINT('Ctrl Pts',(-0.704537347304013,0.893958377091083,
2.21196487801731));
#22145=CARTESIAN_POINT('Ctrl Pts',(-0.746112639361755,1.02870504118196,
2.20411432697963));
#22146=CARTESIAN_POINT('Ctrl Pts',(-0.656650642818685,1.1377083419588,2.19626377594195));
#22147=CARTESIAN_POINT('Ctrl Pts',(-0.516383003000816,1.12321152777512,
2.18841322490427));
#22148=CARTESIAN_POINT('Ctrl Pts',(-0.451105073971734,0.998215686412011,
2.18056267386659));
#22149=CARTESIAN_POINT('Ctrl Pts',(-0.519359654383078,0.874820059671476,
2.17271212282892));
#22150=CARTESIAN_POINT('Ctrl Pts',(-0.659934413848564,0.863688779835656,
2.16486157179123));
#22151=CARTESIAN_POINT('Ctrl Pts',(-0.746758566135216,0.974804642002754,
2.15701102075356));
#22152=CARTESIAN_POINT('Ctrl Pts',(-0.701966147287513,1.1085163018849,2.14916046971588));
#22153=CARTESIAN_POINT('Ctrl Pts',(-0.565728063523024,1.14490795911313,
2.1413099186782));
#22154=CARTESIAN_POINT('Ctrl Pts',(-0.46022586700825,1.0513427200952,2.13345936764053));
#22155=CARTESIAN_POINT('Ctrl Pts',(-0.48007643619797,0.91173209636872,2.12560881660285));
#22156=CARTESIAN_POINT('Ctrl Pts',(-0.607477307839948,0.851282252067638,
2.11775826556517));
#22157=CARTESIAN_POINT('Ctrl Pts',(-0.728172353197516,0.924205970555728,
2.10990771452749));
#22158=CARTESIAN_POINT('Ctrl Pts',(-0.733919382826205,1.06510367305662,
2.10205716348981));
#22159=CARTESIAN_POINT('Ctrl Pts',(-0.619564330621895,1.14761466419362,
2.09420661245214));
#22160=CARTESIAN_POINT('Ctrl Pts',(-0.487663512883551,1.09774168769659,
2.08635606141446));
#22161=CARTESIAN_POINT('Ctrl Pts',(-0.456508744565289,0.960210910014111,
2.07850551037678));
#22162=CARTESIAN_POINT('Ctrl Pts',(-0.554040311779553,0.858365372348507,
2.0706549593391));
#22163=CARTESIAN_POINT('Ctrl Pts',(-0.692789686134866,0.883538310212708,
2.06280440830143));
#22164=CARTESIAN_POINT('Ctrl Pts',(-0.748322934114825,1.01316241211532,
2.05495385726374));
#22165=CARTESIAN_POINT('Ctrl Pts',(-0.670836903808495,1.13097124155368,
2.04710330622607));
#22166=CARTESIAN_POINT('Ctrl Pts',(-0.529822152955879,1.13134338116118,
2.03925275518839));
#22167=CARTESIAN_POINT('Ctrl Pts',(-0.451745545482087,1.01388153416533,
2.03140220415071));
#22168=CARTESIAN_POINT('Ctrl Pts',(-0.506625160883627,0.884053245874464,
2.02355165311303));
#22169=CARTESIAN_POINT('Ctrl Pts',(-0.645248914391877,0.858044950614234,
2.01570110207536));
#22170=CARTESIAN_POINT('Ctrl Pts',(-0.743289784352549,0.959678694562408,
2.00785055103768));
#22171=CARTESIAN_POINT('Ctrl Pts',(-0.722948120505502,1.0510141400767,2.00261685034589));
#22172=CARTESIAN_POINT('Ctrl Pts',(-0.695811615272238,1.08252112989365,
2.));
#22173=CARTESIAN_POINT('Ctrl Pts',(-0.695811615272238,1.08252112989365,
2.));
#22174=CARTESIAN_POINT('Ctrl Pts',(-0.702493043757975,1.07628156364939,
2.));
#22175=CARTESIAN_POINT('Ctrl Pts',(-0.708395726655653,1.06931034161853,
2.));
#22176=CARTESIAN_POINT('Ctrl Pts',(-0.713512684042454,1.06178682515746,
2.));
#22177=CARTESIAN_POINT('Ctrl Pts',(-0.717502373507965,1.05592074262065,
2.));
#22178=CARTESIAN_POINT('Ctrl Pts',(-0.721014109525759,1.04971755287119,
2.));
#22179=CARTESIAN_POINT('Ctrl Pts',(-0.724031985841351,1.04324617113496,
2.));
#22180=CARTESIAN_POINT('Ctrl Pts',(-0.72532920883522,1.04046447158453,2.));
#22181=CARTESIAN_POINT('Ctrl Pts',(-0.726532666614568,1.03763771042115,
2.));
#22182=CARTESIAN_POINT('Ctrl Pts',(-0.727638826408048,1.0347790826819,2.));
#22183=CARTESIAN_POINT('Ctrl Pts',(-0.731193005346523,1.0255940855742,2.));
#22184=CARTESIAN_POINT('Ctrl Pts',(-0.733756270098347,1.01606060371262,
2.));
#22185=CARTESIAN_POINT('Ctrl Pts',(-0.73529467500939,1.0063604242084,2.));
#22186=CARTESIAN_POINT('Ctrl Pts',(-0.736007760405585,1.00186417208695,
2.));
#22187=CARTESIAN_POINT('Ctrl Pts',(-0.736500058162718,0.997331645993815,
2.));
#22188=CARTESIAN_POINT('Ctrl Pts',(-0.736764718140032,0.992779414308968,
2.));
#22189=CARTESIAN_POINT('Ctrl Pts',(-0.736959136386439,0.989435361647935,
2.));
#22190=CARTESIAN_POINT('Ctrl Pts',(-0.737030047799371,0.986088140051384,
2.));
#22191=CARTESIAN_POINT('Ctrl Pts',(-0.736976193579456,0.982751455795261,
2.));
#22192=CARTESIAN_POINT('Ctrl Pts',(-0.73686292459887,0.975733568899372,
2.));
#22193=CARTESIAN_POINT('Ctrl Pts',(-0.736199092496592,0.968753171717965,
2.));
#22194=CARTESIAN_POINT('Ctrl Pts',(-0.734968654150234,0.961871622922131,
2.));
#22195=CARTESIAN_POINT('Ctrl Pts',(-0.733610341240648,0.954274902131536,
2.));
#22196=CARTESIAN_POINT('Ctrl Pts',(-0.731561985767923,0.946798189069373,
2.));
#22197=CARTESIAN_POINT('Ctrl Pts',(-0.728883458720402,0.939498582185105,
2.));
#22198=CARTESIAN_POINT('Ctrl Pts',(-0.727748853408495,0.936406519794552,
2.));
#22199=CARTESIAN_POINT('Ctrl Pts',(-0.726503727419379,0.933354179904992,
2.));
#22200=CARTESIAN_POINT('Ctrl Pts',(-0.725155499563838,0.930349726147835,
2.));
#22201=CARTESIAN_POINT('Ctrl Pts',(-0.721333577255107,0.921832776440231,
2.));
#22202=CARTESIAN_POINT('Ctrl Pts',(-0.716682008196949,0.913689860477865,
2.));
#22203=CARTESIAN_POINT('Ctrl Pts',(-0.711310122504209,0.906016289602163,
2.));
#22204=CARTESIAN_POINT('Ctrl Pts',(-0.708434363463016,0.901908357660524,
2.));
#22205=CARTESIAN_POINT('Ctrl Pts',(-0.705351534711708,0.897934993684464,
2.));
#22206=CARTESIAN_POINT('Ctrl Pts',(-0.702074554712817,0.894112147617013,
2.));
#22207=CARTESIAN_POINT('Ctrl Pts',(-0.699663476442214,0.891299441684046,
2.));
#22208=CARTESIAN_POINT('Ctrl Pts',(-0.69714655627776,0.888568031452597,
2.));
#22209=CARTESIAN_POINT('Ctrl Pts',(-0.694540241228364,0.885935594383534,
2.));
#22210=CARTESIAN_POINT('Ctrl Pts',(-0.68996701323731,0.881316530816482,
2.));
#22211=CARTESIAN_POINT('Ctrl Pts',(-0.685111619991385,0.87699300942471,
2.));
#22212=CARTESIAN_POINT('Ctrl Pts',(-0.680004202609246,0.872997619450478,
2.));
#22213=CARTESIAN_POINT('Ctrl Pts',(-0.67522861092298,0.869261807450647,
2.));
#22214=CARTESIAN_POINT('Ctrl Pts',(-0.670227038735164,0.865810222770729,
2.));
#22215=CARTESIAN_POINT('Ctrl Pts',(-0.66504978274748,0.862688963354369,
2.));
#22216=CARTESIAN_POINT('Ctrl Pts',(-0.659173901912074,0.859146517620461,
2.));
#22217=CARTESIAN_POINT('Ctrl Pts',(-0.653067296294555,0.856024686886556,
2.));
#22218=CARTESIAN_POINT('Ctrl Pts',(-0.64676194038029,0.853364152629858,
2.));
#22219=CARTESIAN_POINT('Ctrl Pts',(-0.644516589878667,0.85241673078578,
2.));
#22220=CARTESIAN_POINT('Ctrl Pts',(-0.642245983976318,0.851527865406908,
2.));
#22221=CARTESIAN_POINT('Ctrl Pts',(-0.639952236162157,0.850696980524378,
2.));
#22222=CARTESIAN_POINT('Ctrl Pts',(-0.726369333664333,1.00010094057762,
2.35565803263806));
#22223=CARTESIAN_POINT('Ctrl Pts',(-0.726467565903334,1.01274184217687,
2.35486362065721));
#22224=CARTESIAN_POINT('Ctrl Pts',(-0.724719482090242,1.02535623071191,
2.35406920867636));
#22225=CARTESIAN_POINT('Ctrl Pts',(-0.721011471558047,1.03736537841382,
2.35327479669551));
#22226=CARTESIAN_POINT('Ctrl Pts',(-0.708797017499383,1.07692437686191,
2.35065794634961));
#22227=CARTESIAN_POINT('Ctrl Pts',(-0.675315572982339,1.10991596087659,
2.34804109600372));
#22228=CARTESIAN_POINT('Ctrl Pts',(-0.635581429433771,1.12154744714583,
2.34542424565783));
#22229=CARTESIAN_POINT('Ctrl Pts',(-0.595847285885203,1.13317893341507,
2.34280739531194));
#22230=CARTESIAN_POINT('Ctrl Pts',(-0.549860443305111,1.12345032193889,
2.34019054496604));
#22231=CARTESIAN_POINT('Ctrl Pts',(-0.518241534391711,1.09672346000923,
2.33757369462015));
#22232=CARTESIAN_POINT('Ctrl Pts',(-0.486622625478311,1.06999659807958,
2.33495684427426));
#22233=CARTESIAN_POINT('Ctrl Pts',(-0.469371650231601,1.02627148569646,
2.33233999392837));
#22234=CARTESIAN_POINT('Ctrl Pts',(-0.474224361799485,0.985155277051315,
2.32972314358247));
#22235=CARTESIAN_POINT('Ctrl Pts',(-0.47907707336737,0.944039068406169,
2.32710629323658));
#22236=CARTESIAN_POINT('Ctrl Pts',(-0.506033471749848,0.905531763498998,
2.32448944289069));
#22237=CARTESIAN_POINT('Ctrl Pts',(-0.543005880203048,0.886900345920854,
2.3218725925448));
#22238=CARTESIAN_POINT('Ctrl Pts',(-0.579978288656248,0.868268928342709,
2.3192557421989));
#22239=CARTESIAN_POINT('Ctrl Pts',(-0.62696670718017,0.86951339809359,2.31663889185301));
#22240=CARTESIAN_POINT('Ctrl Pts',(-0.662901024969081,0.890075796315165,
2.31402204150712));
#22241=CARTESIAN_POINT('Ctrl Pts',(-0.698835342757992,0.910638194536741,
2.31140519116123));
#22242=CARTESIAN_POINT('Ctrl Pts',(-0.723715559811894,0.950518521229011,
2.30878834081533));
#22243=CARTESIAN_POINT('Ctrl Pts',(-0.72638506326613,0.991833925084817,
2.30617149046944));
#22244=CARTESIAN_POINT('Ctrl Pts',(-0.726559659603113,0.994536119817981,
2.30600033785898));
#22245=CARTESIAN_POINT('Ctrl Pts',(-0.726639245398498,0.997244453365998,
2.30582918524852));
#22246=CARTESIAN_POINT('Ctrl Pts',(-0.726626272216059,0.999953562434948,
2.30565803263806));
#22247=CARTESIAN_POINT('Ctrl Pts',(-0.639851384185722,0.850935057178148,
2.4));
#22248=CARTESIAN_POINT('Ctrl Pts',(-0.649880557039356,0.854599675659919,
2.4));
#22249=CARTESIAN_POINT('Ctrl Pts',(-0.659434997625568,0.85936263163469,
2.4));
#22250=CARTESIAN_POINT('Ctrl Pts',(-0.668403171068605,0.865074092345247,
2.4));
#22251=CARTESIAN_POINT('Ctrl Pts',(-0.672868373471587,0.86791779605496,
2.4));
#22252=CARTESIAN_POINT('Ctrl Pts',(-0.67718781684999,0.870997354370473,
2.4));
#22253=CARTESIAN_POINT('Ctrl Pts',(-0.681344478651501,0.874297577803816,
2.4));
#22254=CARTESIAN_POINT('Ctrl Pts',(-0.684149819111287,0.8765249060701,2.4));
#22255=CARTESIAN_POINT('Ctrl Pts',(-0.686880965099162,0.878852785859471,
2.4));
#22256=CARTESIAN_POINT('Ctrl Pts',(-0.689531958931665,0.88127688968642,
2.4));
#22257=CARTESIAN_POINT('Ctrl Pts',(-0.691903137355438,0.883445126602317,
2.4));
#22258=CARTESIAN_POINT('Ctrl Pts',(-0.694203487834536,0.885684268626149,
2.4));
#22259=CARTESIAN_POINT('Ctrl Pts',(-0.696428596284293,0.887989081198335,
2.4));
#22260=CARTESIAN_POINT('Ctrl Pts',(-0.703655665265446,0.895475026186606,
2.4));
#22261=CARTESIAN_POINT('Ctrl Pts',(-0.710097115492295,0.903656379805453,
2.4));
#22262=CARTESIAN_POINT('Ctrl Pts',(-0.715619698888934,0.91241311638882,
2.4));
#22263=CARTESIAN_POINT('Ctrl Pts',(-0.717914152011463,0.916051254584994,
2.4));
#22264=CARTESIAN_POINT('Ctrl Pts',(-0.720049438182606,0.919788953917886,
2.4));
#22265=CARTESIAN_POINT('Ctrl Pts',(-0.722013340315698,0.923618244020841,
2.4));
#22266=CARTESIAN_POINT('Ctrl Pts',(-0.723497106826098,0.926511347662634,
2.4));
#22267=CARTESIAN_POINT('Ctrl Pts',(-0.724882791677009,0.929457049049758,
2.4));
#22268=CARTESIAN_POINT('Ctrl Pts',(-0.726159625039968,0.932438198899027,
2.4));
#22269=CARTESIAN_POINT('Ctrl Pts',(-0.7293219265251,0.939821538706109,2.4));
#22270=CARTESIAN_POINT('Ctrl Pts',(-0.731828922840258,0.947441945091078,
2.4));
#22271=CARTESIAN_POINT('Ctrl Pts',(-0.733609784156052,0.955243638029731,
2.4));
#22272=CARTESIAN_POINT('Ctrl Pts',(-0.735247937517986,0.962420148296355,
2.4));
#22273=CARTESIAN_POINT('Ctrl Pts',(-0.736271216774028,0.969750560405923,
2.4));
#22274=CARTESIAN_POINT('Ctrl Pts',(-0.736691013623241,0.977159425155101,
2.4));
#22275=CARTESIAN_POINT('Ctrl Pts',(-0.736867157952635,0.980268141943398,
2.4));
#22276=CARTESIAN_POINT('Ctrl Pts',(-0.736936476729183,0.983387171734525,
2.4));
#22277=CARTESIAN_POINT('Ctrl Pts',(-0.736900577814768,0.986501043637764,
2.4));
#22278=CARTESIAN_POINT('Ctrl Pts',(-0.73680325432052,0.994942883710025,
2.4));
#22279=CARTESIAN_POINT('Ctrl Pts',(-0.735935887531182,1.00336876050526,
2.4));
#22280=CARTESIAN_POINT('Ctrl Pts',(-0.73432454218896,1.01166505164342,2.4));
#22281=CARTESIAN_POINT('Ctrl Pts',(-0.733128713302574,1.01782198419718,
2.4));
#22282=CARTESIAN_POINT('Ctrl Pts',(-0.731522518607655,1.02390757353733,
2.4));
#22283=CARTESIAN_POINT('Ctrl Pts',(-0.729508194962256,1.0298701636783,2.4));
#22284=CARTESIAN_POINT('Ctrl Pts',(-0.728322998806314,1.03337845735825,
2.4));
#22285=CARTESIAN_POINT('Ctrl Pts',(-0.726998704692332,1.03683671166907,
2.4));
#22286=CARTESIAN_POINT('Ctrl Pts',(-0.72553907497761,1.04022912662095,2.4));
#22287=CARTESIAN_POINT('Ctrl Pts',(-0.723248641788982,1.04555246288699,
2.4));
#22288=CARTESIAN_POINT('Ctrl Pts',(-0.720623684757818,1.05071851440316,
2.4));
#22289=CARTESIAN_POINT('Ctrl Pts',(-0.717666939943194,1.055684952745,2.4));
#22290=CARTESIAN_POINT('Ctrl Pts',(-0.715625486572472,1.05911397788213,
2.4));
#22291=CARTESIAN_POINT('Ctrl Pts',(-0.713425317203702,1.06244758415869,
2.4));
#22292=CARTESIAN_POINT('Ctrl Pts',(-0.711075718450412,1.06565920682025,
2.4));
#22293=CARTESIAN_POINT('Ctrl Pts',(-0.707783291943712,1.07015956313241,
2.4));
#22294=CARTESIAN_POINT('Ctrl Pts',(-0.704194030655052,1.07442716580257,
2.4));
#22295=CARTESIAN_POINT('Ctrl Pts',(-0.700309061659577,1.07842077162732,
2.4));
#22296=CARTESIAN_POINT('Ctrl Pts',(-0.69890728532317,1.07986174635546,2.4));
#22297=CARTESIAN_POINT('Ctrl Pts',(-0.697466969165074,1.08126698735129,
2.4));
#22298=CARTESIAN_POINT('Ctrl Pts',(-0.695989827719556,1.08263574823442,
2.4));
#22299=CARTESIAN_POINT('Origin',(0.,0.,2.));
#22300=CARTESIAN_POINT('',(-0.8,0.6,2.));
#22301=CARTESIAN_POINT('',(0.8,0.6,2.));
#22302=CARTESIAN_POINT('Origin',(0.,0.,2.));
#22303=CARTESIAN_POINT('',(-1.8,0.6,2.));
#22304=CARTESIAN_POINT('',(-1.8,0.6,2.));
#22305=CARTESIAN_POINT('',(-1.8,1.4,2.));
#22306=CARTESIAN_POINT('',(-1.8,1.4,2.));
#22307=CARTESIAN_POINT('',(1.8,1.4,2.));
#22308=CARTESIAN_POINT('',(1.8,1.4,2.));
#22309=CARTESIAN_POINT('',(1.8,0.6,2.));
#22310=CARTESIAN_POINT('',(1.8,0.6,2.));
#22311=CARTESIAN_POINT('',(-1.8,0.6,2.));
#22312=CARTESIAN_POINT('Ctrl Pts',(0.504188384727762,1.08252112989365,2.));
#22313=CARTESIAN_POINT('Ctrl Pts',(0.497506952411728,1.07628156007241,2.));
#22314=CARTESIAN_POINT('Ctrl Pts',(0.491604265140002,1.06931033514179,2.));
#22315=CARTESIAN_POINT('Ctrl Pts',(0.486487303479808,1.06178681610824,2.));
#22316=CARTESIAN_POINT('Ctrl Pts',(0.482497614326221,1.0559207369233,2.));
#22317=CARTESIAN_POINT('Ctrl Pts',(0.478985877807952,1.04971755133896,2.));
#22318=CARTESIAN_POINT('Ctrl Pts',(0.47596800043997,1.04324617422688,2.));
#22319=CARTESIAN_POINT('Ctrl Pts',(0.474670775798635,1.04046447410142,2.));
#22320=CARTESIAN_POINT('Ctrl Pts',(0.473467316455455,1.03763771239116,2.));
#22321=CARTESIAN_POINT('Ctrl Pts',(0.472361155190705,1.03477908408591,2.));
#22322=CARTESIAN_POINT('Ctrl Pts',(0.468806973334995,1.02559408983729,2.));
#22323=CARTESIAN_POINT('Ctrl Pts',(0.466243705645806,1.01606061108597,2.));
#22324=CARTESIAN_POINT('Ctrl Pts',(0.464705298489784,1.00636043426204,2.));
#22325=CARTESIAN_POINT('Ctrl Pts',(0.463992209982944,1.00186417033063,2.));
#22326=CARTESIAN_POINT('Ctrl Pts',(0.463499910544365,0.997331632125338,
2.));
#22327=CARTESIAN_POINT('Ctrl Pts',(0.463235250450622,0.992779388102766,
2.));
#22328=CARTESIAN_POINT('Ctrl Pts',(0.463040833672037,0.989435353096635,
2.));
#22329=CARTESIAN_POINT('Ctrl Pts',(0.46296992260639,0.986088149337579,2.));
#22330=CARTESIAN_POINT('Ctrl Pts',(0.46302377604218,0.982751482606387,2.));
#22331=CARTESIAN_POINT('Ctrl Pts',(0.463137043908312,0.975733599437203,
2.));
#22332=CARTESIAN_POINT('Ctrl Pts',(0.463800875129207,0.968753205425666,
2.));
#22333=CARTESIAN_POINT('Ctrl Pts',(0.465031313050322,0.961871658945486,
2.));
#22334=CARTESIAN_POINT('Ctrl Pts',(0.466389625771061,0.954274939141924,
2.));
#22335=CARTESIAN_POINT('Ctrl Pts',(0.468437981894213,0.946798226077515,
2.));
#22336=CARTESIAN_POINT('Ctrl Pts',(0.471116510174533,0.93949861845872,2.));
#22337=CARTESIAN_POINT('Ctrl Pts',(0.472251116178103,0.936406555295212,
2.));
#22338=CARTESIAN_POINT('Ctrl Pts',(0.473496242998671,0.933354214505235,
2.));
#22339=CARTESIAN_POINT('Ctrl Pts',(0.474844471797333,0.930349759755262,
2.));
#22340=CARTESIAN_POINT('Ctrl Pts',(0.478666396590115,0.921832807655503,
2.));
#22341=CARTESIAN_POINT('Ctrl Pts',(0.483317968956197,0.913689888494062,
2.));
#22342=CARTESIAN_POINT('Ctrl Pts',(0.488689858313544,0.906016314077791,
2.));
#22343=CARTESIAN_POINT('Ctrl Pts',(0.491565612706781,0.90190838968258,2.));
#22344=CARTESIAN_POINT('Ctrl Pts',(0.494648435962255,0.897935032536209,
2.));
#22345=CARTESIAN_POINT('Ctrl Pts',(0.497925409635587,0.894112192538158,
2.));
#22346=CARTESIAN_POINT('Ctrl Pts',(0.500336494700513,0.891299477715359,
2.));
#22347=CARTESIAN_POINT('Ctrl Pts',(0.502853422244813,0.888568058918467,
2.));
#22348=CARTESIAN_POINT('Ctrl Pts',(0.505459745106002,0.885935613780059,
2.));
#22349=CARTESIAN_POINT('Ctrl Pts',(0.510032972332535,0.881316550670653,
2.));
#22350=CARTESIAN_POINT('Ctrl Pts',(0.514888364383629,0.876993029350264,
2.));
#22351=CARTESIAN_POINT('Ctrl Pts',(0.519995780056594,0.872997639132679,
2.));
#22352=CARTESIAN_POINT('Ctrl Pts',(0.52477137880872,0.869261820127707,2.));
#22353=CARTESIAN_POINT('Ctrl Pts',(0.529772958435197,0.865810229192487,
2.));
#22354=CARTESIAN_POINT('Ctrl Pts',(0.534950221975527,0.862688964531106,
2.));
#22355=CARTESIAN_POINT('Ctrl Pts',(0.540826105312277,0.859146516504166,
2.));
#22356=CARTESIAN_POINT('Ctrl Pts',(0.546932713096854,0.856024683905292,
2.));
#22357=CARTESIAN_POINT('Ctrl Pts',(0.553238070670066,0.853364148387157,
2.));
#22358=CARTESIAN_POINT('Ctrl Pts',(0.55548342158471,0.852416726168872,2.));
#22359=CARTESIAN_POINT('Ctrl Pts',(0.55775402783163,0.851527860483116,2.));
#22360=CARTESIAN_POINT('Ctrl Pts',(0.560047775926793,0.850696975355778,
2.));
#22361=CARTESIAN_POINT('Ctrl Pts',(0.639851384185725,0.850935057178149,
2.));
#22362=CARTESIAN_POINT('Ctrl Pts',(0.649880550625801,0.854599673316433,
2.));
#22363=CARTESIAN_POINT('Ctrl Pts',(0.659434984589242,0.859362630571034,
2.));
#22364=CARTESIAN_POINT('Ctrl Pts',(0.668403151796856,0.865074094293816,
2.));
#22365=CARTESIAN_POINT('Ctrl Pts',(0.672868418174611,0.867917842223432,
2.));
#22366=CARTESIAN_POINT('Ctrl Pts',(0.677187921251714,0.870997452272092,
2.));
#22367=CARTESIAN_POINT('Ctrl Pts',(0.68134463777063,0.874297734044997,2.));
#22368=CARTESIAN_POINT('Ctrl Pts',(0.684149977150149,0.876525071506887,
2.));
#22369=CARTESIAN_POINT('Ctrl Pts',(0.686881121795098,0.878852960779101,
2.));
#22370=CARTESIAN_POINT('Ctrl Pts',(0.689532114008666,0.881277074288136,
2.));
#22371=CARTESIAN_POINT('Ctrl Pts',(0.691903244332041,0.883445277204446,
2.));
#22372=CARTESIAN_POINT('Ctrl Pts',(0.694203548662863,0.885684381973589,
2.));
#22373=CARTESIAN_POINT('Ctrl Pts',(0.696428614090338,0.88798915510679,2.));
#22374=CARTESIAN_POINT('Ctrl Pts',(0.703655681573731,0.895475115187732,
2.));
#22375=CARTESIAN_POINT('Ctrl Pts',(0.710097129721786,0.903656484453022,
2.));
#22376=CARTESIAN_POINT('Ctrl Pts',(0.715619710640267,0.912413235085866,
2.));
#22377=CARTESIAN_POINT('Ctrl Pts',(0.717914173550032,0.916051396270592,
2.));
#22378=CARTESIAN_POINT('Ctrl Pts',(0.720049467939456,0.919789119253813,
2.));
#22379=CARTESIAN_POINT('Ctrl Pts',(0.722013376555431,0.923618433392056,
2.));
#22380=CARTESIAN_POINT('Ctrl Pts',(0.723497129119939,0.926511518450447,
2.));
#22381=CARTESIAN_POINT('Ctrl Pts',(0.724882801444961,0.929457199976584,
2.));
#22382=CARTESIAN_POINT('Ctrl Pts',(0.726159624011702,0.932438329054375,
2.));
#22383=CARTESIAN_POINT('Ctrl Pts',(0.729321918563565,0.939821663659088,
2.));
#22384=CARTESIAN_POINT('Ctrl Pts',(0.731828910123054,0.947442062000798,
2.));
#22385=CARTESIAN_POINT('Ctrl Pts',(0.733609769329411,0.955243743262114,
2.));
#22386=CARTESIAN_POINT('Ctrl Pts',(0.735247922763181,0.962420251602462,
2.));
#22387=CARTESIAN_POINT('Ctrl Pts',(0.736271202825978,0.969750659080777,
2.));
#22388=CARTESIAN_POINT('Ctrl Pts',(0.736691001072906,0.977159517273332,
2.));
#22389=CARTESIAN_POINT('Ctrl Pts',(0.736867146035702,0.980268232138734,
2.));
#22390=CARTESIAN_POINT('Ctrl Pts',(0.736936465492878,0.983387259690693,
2.));
#22391=CARTESIAN_POINT('Ctrl Pts',(0.736900567292279,0.986501129084147,
2.));
#22392=CARTESIAN_POINT('Ctrl Pts',(0.736803245735092,0.994942962189629,
2.));
#22393=CARTESIAN_POINT('Ctrl Pts',(0.73593588116366,1.00336883005034,2.));
#22394=CARTESIAN_POINT('Ctrl Pts',(0.734324538110121,1.01166511142386,2.));
#22395=CARTESIAN_POINT('Ctrl Pts',(0.733128714763866,1.01782201695168,2.));
#22396=CARTESIAN_POINT('Ctrl Pts',(0.731522528281544,1.02390757926145,2.));
#22397=CARTESIAN_POINT('Ctrl Pts',(0.729508215420297,1.02987014335002,2.));
#22398=CARTESIAN_POINT('Ctrl Pts',(0.728323015262132,1.03337845233062,2.));
#22399=CARTESIAN_POINT('Ctrl Pts',(0.726998715515976,1.03683672165704,2.));
#22400=CARTESIAN_POINT('Ctrl Pts',(0.725539078662676,1.04022915093548,2.));
#22401=CARTESIAN_POINT('Ctrl Pts',(0.723248638897094,1.04555249893377,2.));
#22402=CARTESIAN_POINT('Ctrl Pts',(0.72062367285432,1.05071856137362,2.));
#22403=CARTESIAN_POINT('Ctrl Pts',(0.717666916538866,1.05568500977016,2.));
#22404=CARTESIAN_POINT('Ctrl Pts',(0.71562546757316,1.05911402111255,2.));
#22405=CARTESIAN_POINT('Ctrl Pts',(0.713425303385499,1.06244761425647,2.));
#22406=CARTESIAN_POINT('Ctrl Pts',(0.711075710473028,1.06565922484506,2.));
#22407=CARTESIAN_POINT('Ctrl Pts',(0.707783289804617,1.0701595674468,2.));
#22408=CARTESIAN_POINT('Ctrl Pts',(0.704194035235276,1.07442715810878,2.));
#22409=CARTESIAN_POINT('Ctrl Pts',(0.700309073757905,1.07842075422663,2.));
#22410=CARTESIAN_POINT('Ctrl Pts',(0.698907297616712,1.07986172804018,2.));
#22411=CARTESIAN_POINT('Ctrl Pts',(0.697466981619643,1.08126696829348,2.));
#22412=CARTESIAN_POINT('Ctrl Pts',(0.695989840302895,1.08263572859343,2.));
#22413=CARTESIAN_POINT('Origin',(0.6,1.,2.51042117235887));
#22414=CARTESIAN_POINT('Ctrl Pts',(0.445511859130131,1.0000741974826,2.38542117235887));
#22415=CARTESIAN_POINT('Ctrl Pts',(0.445481645904189,1.00486660347515,2.38517311518799));
#22416=CARTESIAN_POINT('Ctrl Pts',(0.447840382858598,1.06018738535655,2.38230820767121));
#22417=CARTESIAN_POINT('Ctrl Pts',(0.514365803623529,1.16027111832567,2.37682644980854));
#22418=CARTESIAN_POINT('Ctrl Pts',(0.686438402045863,1.1598170503231,2.36897589877086));
#22419=CARTESIAN_POINT('Ctrl Pts',(0.780990355889297,1.01606136385454,2.36112534773319));
#22420=CARTESIAN_POINT('Ctrl Pts',(0.713226176840859,0.857888178208998,
2.35327479669551));
#22421=CARTESIAN_POINT('Ctrl Pts',(0.54391790721615,0.827171013394288,2.34542424565783));
#22422=CARTESIAN_POINT('Ctrl Pts',(0.453699048722976,0.921380393628473,
2.33947303754562));
#22423=CARTESIAN_POINT('Ctrl Pts',(0.445641803334383,0.985947130304853,
2.3361386797793));
#22424=CARTESIAN_POINT('Ctrl Pts',(0.445758404806891,0.999869526120069,
2.33542117235887));
#22425=CARTESIAN_POINT('Ctrl Pts',(0.445864724392684,0.99983533609866,2.38957882764113));
#22426=CARTESIAN_POINT('Ctrl Pts',(0.446099244735942,1.0340318743782,2.38781885106897));
#22427=CARTESIAN_POINT('Ctrl Pts',(0.47398874803022,1.11953643095444,2.38344202415091));
#22428=CARTESIAN_POINT('Ctrl Pts',(0.614413228882944,1.18108612135922,2.37644834688697));
#22429=CARTESIAN_POINT('Ctrl Pts',(0.759000551270414,1.08793755388759,2.36859779584929));
#22430=CARTESIAN_POINT('Ctrl Pts',(0.761051274433651,0.91584221771742,2.36074724481161));
#22431=CARTESIAN_POINT('Ctrl Pts',(0.618637433005314,0.819263404514795,
2.35289669377393));
#22432=CARTESIAN_POINT('Ctrl Pts',(0.475625295654385,0.878125251073759,
2.34584055471711));
#22433=CARTESIAN_POINT('Ctrl Pts',(0.446073423867575,0.964737113217481,
2.34140126600617));
#22434=CARTESIAN_POINT('Ctrl Pts',(0.445798439227784,1.00012317213786,2.33957882764113));
#22435=CARTESIAN_POINT('Ctrl Pts',(0.695811615272236,1.08252112989365,2.4));
#22436=CARTESIAN_POINT('Ctrl Pts',(0.7229481205055,1.0510141400767,2.39738314965411));
#22437=CARTESIAN_POINT('Ctrl Pts',(0.743289653273766,0.959678556377187,
2.39214944896232));
#22438=CARTESIAN_POINT('Ctrl Pts',(0.645248987396393,0.85804501052042,2.38429889792465));
#22439=CARTESIAN_POINT('Ctrl Pts',(0.506625118128944,0.884053189554221,
2.37644834688697));
#22440=CARTESIAN_POINT('Ctrl Pts',(0.45174554898112,1.01388156392493,2.36859779584929));
#22441=CARTESIAN_POINT('Ctrl Pts',(0.529822137836651,1.13134337597071,2.36074724481161));
#22442=CARTESIAN_POINT('Ctrl Pts',(0.670836914703171,1.13097126385843,2.35289669377393));
#22443=CARTESIAN_POINT('Ctrl Pts',(0.748322945574864,1.01316240738436,2.34504614273625));
#22444=CARTESIAN_POINT('Ctrl Pts',(0.692789695797321,0.883538302880933,
2.33719559169858));
#22445=CARTESIAN_POINT('Ctrl Pts',(0.554040306983033,0.858365357379829,
2.3293450406609));
#22446=CARTESIAN_POINT('Ctrl Pts',(0.456508731628746,0.960210907421746,
2.32149448962322));
#22447=CARTESIAN_POINT('Ctrl Pts',(0.487663502390397,1.09774169610628,2.31364393858554));
#22448=CARTESIAN_POINT('Ctrl Pts',(0.619564332496711,1.14761467812196,2.30579338754787));
#22449=CARTESIAN_POINT('Ctrl Pts',(0.733919395128131,1.0651036788751,2.29794283651019));
#22450=CARTESIAN_POINT('Ctrl Pts',(0.728172365024857,0.924205963670542,
2.29009228547251));
#22451=CARTESIAN_POINT('Ctrl Pts',(0.607477308519567,0.851282238312653,
2.28224173443483));
#22452=CARTESIAN_POINT('Ctrl Pts',(0.480076425153724,0.911732088265042,
2.27439118339715));
#22453=CARTESIAN_POINT('Ctrl Pts',(0.46022585412805,1.05134272481009,2.26654063235948));
#22454=CARTESIAN_POINT('Ctrl Pts',(0.565728060366633,1.14490797247226,2.2586900813218));
#22455=CARTESIAN_POINT('Ctrl Pts',(0.701966156681371,1.1085163118784,2.25083953028412));
#22456=CARTESIAN_POINT('Ctrl Pts',(0.746758579656851,0.974804639683806,
2.24298897924644));
#22457=CARTESIAN_POINT('Ctrl Pts',(0.659934419370361,0.863688767275607,
2.23513842820876));
#22458=CARTESIAN_POINT('Ctrl Pts',(0.519359646953508,0.874820048138925,
2.22728787717109));
#22459=CARTESIAN_POINT('Ctrl Pts',(0.451105060253533,0.998215686247253,
2.21943732613341));
#22460=CARTESIAN_POINT('Ctrl Pts',(0.516382995296938,1.12321153912718,2.21158677509573));
#22461=CARTESIAN_POINT('Ctrl Pts',(0.656650648038066,1.13770835464619,2.20373622405805));
#22462=CARTESIAN_POINT('Ctrl Pts',(0.746112652823594,1.02870504382673,2.19588567302037));
#22463=CARTESIAN_POINT('Ctrl Pts',(0.704537356935342,0.893958367321059,
2.1880351219827));
#22464=CARTESIAN_POINT('Ctrl Pts',(0.569210474097529,0.854312347959086,
2.18018457094502));
#22465=CARTESIAN_POINT('Ctrl Pts',(0.461496370101168,0.945322478526838,
2.17233401990734));
#22466=CARTESIAN_POINT('Ctrl Pts',(0.477995614068202,1.08536871014064,2.16448346886966));
#22467=CARTESIAN_POINT('Ctrl Pts',(0.603911291955373,1.14885425315604,2.15663291783199));
#22468=CARTESIAN_POINT('Ctrl Pts',(0.726319229979197,1.07884376278165,2.14878236679431));
#22469=CARTESIAN_POINT('Ctrl Pts',(0.73544107998541,0.938124312232147,2.14093181575663));
#22470=CARTESIAN_POINT('Ctrl Pts',(0.623096148559508,0.852896448126576,
2.13308126471895));
#22471=CARTESIAN_POINT('Ctrl Pts',(0.490038043939787,0.899594549193445,
2.12523071368128));
#22472=CARTESIAN_POINT('Ctrl Pts',(0.455596431949525,1.03633864030821,2.11738016264359));
#22473=CARTESIAN_POINT('Ctrl Pts',(0.550659380176962,1.14049338518748,2.10952961160592));
#22474=CARTESIAN_POINT('Ctrl Pts',(0.689972154741195,1.11865030196008,2.10167906056824));
#22475=CARTESIAN_POINT('Ctrl Pts',(0.748595790516416,0.990398846945399,
2.09382850953056));
#22476=CARTESIAN_POINT('Ctrl Pts',(0.673955132588938,0.870757856106032,
2.08597795849288));
#22477=CARTESIAN_POINT('Ctrl Pts',(0.532989863833319,0.867024446028552,
2.0781274074552));
#22478=CARTESIAN_POINT('Ctrl Pts',(0.45212066157753,0.982546372277999,2.07027685641753));
#22479=CARTESIAN_POINT('Ctrl Pts',(0.503873591498137,1.11372171989345,2.06242630537985));
#22480=CARTESIAN_POINT('Ctrl Pts',(0.641834132936712,1.14290755996024,2.05457575434217));
#22481=CARTESIAN_POINT('Ctrl Pts',(0.742278474130153,1.04393279346011,2.04672520330449));
#22482=CARTESIAN_POINT('Ctrl Pts',(0.71512086495066,0.905553551654031,2.03887465226682));
#22483=CARTESIAN_POINT('Ctrl Pts',(0.584726479537104,0.851884977081971,
2.03102410122914));
#22484=CARTESIAN_POINT('Ctrl Pts',(0.468017266318098,0.931032088917713,
2.02317355019146));
#22485=CARTESIAN_POINT('Ctrl Pts',(0.469697842938816,1.07206544198931,2.01532299915378));
#22486=CARTESIAN_POINT('Ctrl Pts',(0.588188246262365,1.1484015292732,2.0074724481161));
#22487=CARTESIAN_POINT('Ctrl Pts',(0.717366805638866,1.09178084131602,1.99962189707843));
#22488=CARTESIAN_POINT('Ctrl Pts',(0.741097987339953,0.952575306856465,
1.99177134604075));
#22489=CARTESIAN_POINT('Ctrl Pts',(0.672829925654733,0.888579693265875,
1.98653764534896));
#22490=CARTESIAN_POINT('Ctrl Pts',(0.63265850635311,0.877840168374445,1.98392079500307));
#22491=CARTESIAN_POINT('Ctrl Pts',(0.702845629995662,1.08857942294107,2.40535973499898));
#22492=CARTESIAN_POINT('Ctrl Pts',(0.731974363173428,1.05475934582637,2.40274288465309));
#22493=CARTESIAN_POINT('Ctrl Pts',(0.753809270628911,0.956718355494374,
2.3975091839613));
#22494=CARTESIAN_POINT('Ctrl Pts',(0.648570944161886,0.84762337757721,2.38965863292362));
#22495=CARTESIAN_POINT('Ctrl Pts',(0.499769996315029,0.875540948428836,
2.38180808188594));
#22496=CARTESIAN_POINT('Ctrl Pts',(0.440861440741036,1.01490067966319,2.37395753084827));
#22497=CARTESIAN_POINT('Ctrl Pts',(0.524670026432277,1.1409859567557,2.36610697981059));
#22498=CARTESIAN_POINT('Ctrl Pts',(0.676037410484068,1.14058652601332,2.35825642877291));
#22499=CARTESIAN_POINT('Ctrl Pts',(0.759212082346341,1.01412872620776,2.35040587773524));
#22500=CARTESIAN_POINT('Ctrl Pts',(0.699601856145167,0.87498826132362,2.34255532669755));
#22501=CARTESIAN_POINT('Ctrl Pts',(0.550666173727406,0.847967242717983,
2.33470477565988));
#22502=CARTESIAN_POINT('Ctrl Pts',(0.445974312690722,0.957289789118585,
2.32685422462219));
#22503=CARTESIAN_POINT('Ctrl Pts',(0.479416312569843,1.10491740781463,2.31900367358452));
#22504=CARTESIAN_POINT('Ctrl Pts',(0.62100064898553,1.15845181740151,2.31115312254684));
#22505=CARTESIAN_POINT('Ctrl Pts',(0.743751094493674,1.06988326884919,2.30330257150917));
#22506=CARTESIAN_POINT('Ctrl Pts',(0.737582145876161,0.918641540547371,
2.29545202047149));
#22507=CARTESIAN_POINT('Ctrl Pts',(0.608026255513821,0.840364116095719,
2.28760146943381));
#22508=CARTESIAN_POINT('Ctrl Pts',(0.471272229662835,0.905251894929553,
2.27975091839613));
#22509=CARTESIAN_POINT('Ctrl Pts',(0.449964327931837,1.05511205362507,2.27190036735845));
#22510=CARTESIAN_POINT('Ctrl Pts',(0.563211984134157,1.15554639881562,2.26404981632078));
#22511=CARTESIAN_POINT('Ctrl Pts',(0.709452007382772,1.11648304256461,2.2561992652831));
#22512=CARTESIAN_POINT('Ctrl Pts',(0.757532868423012,0.972954920994454,
2.24834871424542));
#22513=CARTESIAN_POINT('Ctrl Pts',(0.664334507888787,0.853681471028408,
2.24049816320774));
#22514=CARTESIAN_POINT('Ctrl Pts',(0.513439431236242,0.865629955455834,
2.23264761217006));
#22515=CARTESIAN_POINT('Ctrl Pts',(0.440173930500167,0.998084690760198,
2.22479706113238));
#22516=CARTESIAN_POINT('Ctrl Pts',(0.510244248543333,1.13225712068693,2.21694651009471));
#22517=CARTESIAN_POINT('Ctrl Pts',(0.660809658313168,1.14781822067201,2.20909595905703));
#22518=CARTESIAN_POINT('Ctrl Pts',(0.756839520837664,1.03081242611373,2.20124540801935));
#22519=CARTESIAN_POINT('Ctrl Pts',(0.71221197243725,0.886173315337117,2.19339485698167));
#22520=CARTESIAN_POINT('Ctrl Pts',(0.566950059450412,0.843616681399604,
2.18554430594399));
#22521=CARTESIAN_POINT('Ctrl Pts',(0.451328118901268,0.941308325441225,
2.17769375490632));
#22522=CARTESIAN_POINT('Ctrl Pts',(0.469038655723137,1.09163605844015,2.16984320386864));
#22523=CARTESIAN_POINT('Ctrl Pts',(0.604198439657909,1.15978239590126,2.16199265283096));
#22524=CARTESIAN_POINT('Ctrl Pts',(0.735592962824645,1.08463208173108,2.15414210179328));
#22525=CARTESIAN_POINT('Ctrl Pts',(0.745384493923972,0.933581705393252,
2.14629155075561));
#22526=CARTESIAN_POINT('Ctrl Pts',(0.624791753508452,0.842096833207175,
2.13844099971793));
#22527=CARTESIAN_POINT('Ctrl Pts',(0.481965181210706,0.892223277795097,
2.13059044868025));
#22528=CARTESIAN_POINT('Ctrl Pts',(0.444995036483054,1.03900644347833,2.12273989764257));
#22529=CARTESIAN_POINT('Ctrl Pts',(0.547037036003845,1.15080771437549,2.11488934660489));
#22530=CARTESIAN_POINT('Ctrl Pts',(0.696577465165717,1.12736102005574,2.10703879556722));
#22531=CARTESIAN_POINT('Ctrl Pts',(0.759504958213481,0.989693977794033,
2.09918824452954));
#22532=CARTESIAN_POINT('Ctrl Pts',(0.679384552498262,0.861269537383356,
2.09133769349186));
#22533=CARTESIAN_POINT('Ctrl Pts',(0.52807031119791,0.857262038810666,2.08348714245418));
#22534=CARTESIAN_POINT('Ctrl Pts',(0.441264092248243,0.981265013290105,
2.07563659141651));
#22535=CARTESIAN_POINT('Ctrl Pts',(0.496816466213367,1.12207060588009,2.06778604037882));
#22536=CARTESIAN_POINT('Ctrl Pts',(0.644905387984261,1.15339912591488,2.05993548934115));
#22537=CARTESIAN_POINT('Ctrl Pts',(0.752723855715824,1.04715812177925,2.05208493830347));
#22538=CARTESIAN_POINT('Ctrl Pts',(0.723572469244521,0.89861976073157,2.04423438726579));
#22539=CARTESIAN_POINT('Ctrl Pts',(0.583605173237138,0.84101110496317,2.03638383622811));
#22540=CARTESIAN_POINT('Ctrl Pts',(0.458327747053459,0.92596880613495,2.02853328519044));
#22541=CARTESIAN_POINT('Ctrl Pts',(0.460131703294282,1.07735613016487,2.02068273415276));
#22542=CARTESIAN_POINT('Ctrl Pts',(0.587321085746765,1.15929643527098,2.01283218311508));
#22543=CARTESIAN_POINT('Ctrl Pts',(0.72598329578528,1.09851893655959,2.0049816320774));
#22544=CARTESIAN_POINT('Ctrl Pts',(0.751456703426463,0.949093620540274,
1.99713108103973));
#22545=CARTESIAN_POINT('Ctrl Pts',(0.6781767384384,0.880399765646143,1.99189738034794));
#22546=CARTESIAN_POINT('Ctrl Pts',(0.635056132297315,0.86887179797568,1.98928053000205));
#22547=CARTESIAN_POINT('Ctrl Pts',(0.709879644719089,1.09463771598849,2.41071946999795));
#22548=CARTESIAN_POINT('Ctrl Pts',(0.741000605841355,1.05850455157604,2.40810261965206));
#22549=CARTESIAN_POINT('Ctrl Pts',(0.764328887984058,0.953758154611561,
2.40286891896028));
#22550=CARTESIAN_POINT('Ctrl Pts',(0.651892900927377,0.837201744634001,
2.3950183679226));
#22551=CARTESIAN_POINT('Ctrl Pts',(0.492914874501113,0.867028707303451,
2.38716781688492));
#22552=CARTESIAN_POINT('Ctrl Pts',(0.429977332500953,1.01591979540145,2.37931726584724));
#22553=CARTESIAN_POINT('Ctrl Pts',(0.519517915027903,1.15062853754068,2.37146671480957));
#22554=CARTESIAN_POINT('Ctrl Pts',(0.681237906264966,1.15020178816821,2.36361616377189));
#22555=CARTESIAN_POINT('Ctrl Pts',(0.770101219117818,1.01509504503115,2.35576561273421));
#22556=CARTESIAN_POINT('Ctrl Pts',(0.706414016493014,0.866438219766308,
2.34791506169653));
#22557=CARTESIAN_POINT('Ctrl Pts',(0.547292040471776,0.837569128056136,
2.34006451065885));
#22558=CARTESIAN_POINT('Ctrl Pts',(0.435439893752698,0.954368670815423,
2.33221395962117));
#22559=CARTESIAN_POINT('Ctrl Pts',(0.471169122749288,1.11209311952297,2.3243634085835));
#22560=CARTESIAN_POINT('Ctrl Pts',(0.622436965474348,1.16928895668105,2.31651285754582));
#22561=CARTESIAN_POINT('Ctrl Pts',(0.753582793859216,1.07466285882328,2.30866230650814));
#22562=CARTESIAN_POINT('Ctrl Pts',(0.746991926727465,0.913077117424199,
2.30081175547046));
#22563=CARTESIAN_POINT('Ctrl Pts',(0.608575202508074,0.829445993878789,
2.29296120443279));
#22564=CARTESIAN_POINT('Ctrl Pts',(0.462468034171945,0.898771701594062,
2.28511065339511));
#22565=CARTESIAN_POINT('Ctrl Pts',(0.439702801735622,1.05888138244004,2.27726010235743));
#22566=CARTESIAN_POINT('Ctrl Pts',(0.560695907901683,1.16618482515898,2.26940955131976));
#22567=CARTESIAN_POINT('Ctrl Pts',(0.716937858084172,1.12444977325082,2.26155900028207));
#22568=CARTESIAN_POINT('Ctrl Pts',(0.768307157189173,0.9711052023051,2.2537084492444));
#22569=CARTESIAN_POINT('Ctrl Pts',(0.668734596407212,0.843674174781211,
2.24585789820672));
#22570=CARTESIAN_POINT('Ctrl Pts',(0.507519215518976,0.856439862772741,
2.23800734716904));
#22571=CARTESIAN_POINT('Ctrl Pts',(0.429242800746802,0.997953695273144,
2.23015679613136));
#22572=CARTESIAN_POINT('Ctrl Pts',(0.504105501789727,1.14130270224668,2.22230624509369));
#22573=CARTESIAN_POINT('Ctrl Pts',(0.664968668588271,1.15792808669784,2.214455694056));
#22574=CARTESIAN_POINT('Ctrl Pts',(0.767566388851732,1.03291980840074,2.20660514301833));
#22575=CARTESIAN_POINT('Ctrl Pts',(0.71988658793916,0.878388263353175,2.19875459198065));
#22576=CARTESIAN_POINT('Ctrl Pts',(0.564689644803295,0.832921014840122,
2.19090404094297));
#22577=CARTESIAN_POINT('Ctrl Pts',(0.441159867701366,0.937294172355611,
2.1830534899053));
#22578=CARTESIAN_POINT('Ctrl Pts',(0.460081697378071,1.09790340673965,2.17520293886761));
#22579=CARTESIAN_POINT('Ctrl Pts',(0.604485587360446,1.17071053864647,2.16735238782994));
#22580=CARTESIAN_POINT('Ctrl Pts',(0.744866695670093,1.09042040068052,2.15950183679226));
#22581=CARTESIAN_POINT('Ctrl Pts',(0.755327907862536,0.929039098554358,
2.15165128575458));
#22582=CARTESIAN_POINT('Ctrl Pts',(0.626487358457396,0.831297218287773,
2.1438007347169));
#22583=CARTESIAN_POINT('Ctrl Pts',(0.473892318481626,0.884852006396751,
2.13595018367923));
#22584=CARTESIAN_POINT('Ctrl Pts',(0.434393641016582,1.04167424664844,2.12809963264155));
#22585=CARTESIAN_POINT('Ctrl Pts',(0.54341469183073,1.1611220435635,2.12024908160387));
#22586=CARTESIAN_POINT('Ctrl Pts',(0.703182775590238,1.1360717381514,2.11239853056619));
#22587=CARTESIAN_POINT('Ctrl Pts',(0.770414125910549,0.988989108642668,
2.10454797952851));
#22588=CARTESIAN_POINT('Ctrl Pts',(0.684813972407585,0.851781218660681,
2.09669742849084));
#22589=CARTESIAN_POINT('Ctrl Pts',(0.523150758562502,0.84749963159278,2.08884687745316));
#22590=CARTESIAN_POINT('Ctrl Pts',(0.430407522918953,0.979983654302211,
2.08099632641548));
#22591=CARTESIAN_POINT('Ctrl Pts',(0.489759340928599,1.13041949186674,2.0731457753778));
#22592=CARTESIAN_POINT('Ctrl Pts',(0.647976643031809,1.16389069186952,2.06529522434013));
#22593=CARTESIAN_POINT('Ctrl Pts',(0.763169237301496,1.05038345009838,2.05744467330245));
#22594=CARTESIAN_POINT('Ctrl Pts',(0.732024073538381,0.89168596980911,2.04959412226477));
#22595=CARTESIAN_POINT('Ctrl Pts',(0.582483866937173,0.830137232844369,
2.04174357122709));
#22596=CARTESIAN_POINT('Ctrl Pts',(0.448638227788819,0.920905523352185,
2.03389302018941));
#22597=CARTESIAN_POINT('Ctrl Pts',(0.450565563649749,1.08264681834044,2.02604246915174));
#22598=CARTESIAN_POINT('Ctrl Pts',(0.586453925231163,1.17019134126876,2.01819191811406));
#22599=CARTESIAN_POINT('Ctrl Pts',(0.734599785931696,1.10525703180317,2.01034136707638));
#22600=CARTESIAN_POINT('Ctrl Pts',(0.761815419512973,0.945611934224082,
2.0024908160387));
#22601=CARTESIAN_POINT('Ctrl Pts',(0.683523551222068,0.872219838026411,
1.99725711534692));
#22602=CARTESIAN_POINT('Ctrl Pts',(0.63745375824152,0.859903427576914,1.99464026500102));
#22603=CARTESIAN_POINT('Ctrl Pts',(0.716913659442515,1.10069600903591,2.41607920499693));
#22604=CARTESIAN_POINT('Ctrl Pts',(0.750026848509282,1.0622497573257,2.41346235465104));
#22605=CARTESIAN_POINT('Ctrl Pts',(0.774848505339203,0.950797953728747,
2.40822865395925));
#22606=CARTESIAN_POINT('Ctrl Pts',(0.65521485769287,0.826780111690792,2.40037810292158));
#22607=CARTESIAN_POINT('Ctrl Pts',(0.486059752687198,0.858516466178065,
2.3925275518839));
#22608=CARTESIAN_POINT('Ctrl Pts',(0.419093224260869,1.01693891113971,2.38467700084622));
#22609=CARTESIAN_POINT('Ctrl Pts',(0.514365803623529,1.16027111832567,2.37682644980854));
#22610=CARTESIAN_POINT('Ctrl Pts',(0.686438402045863,1.1598170503231,2.36897589877086));
#22611=CARTESIAN_POINT('Ctrl Pts',(0.780990355889297,1.01606136385454,2.36112534773319));
#22612=CARTESIAN_POINT('Ctrl Pts',(0.713226176840859,0.857888178208998,
2.35327479669551));
#22613=CARTESIAN_POINT('Ctrl Pts',(0.54391790721615,0.827171013394288,2.34542424565783));
#22614=CARTESIAN_POINT('Ctrl Pts',(0.424905474814674,0.951447552512262,
2.33757369462016));
#22615=CARTESIAN_POINT('Ctrl Pts',(0.462921932928734,1.11926883123131,2.32972314358247));
#22616=CARTESIAN_POINT('Ctrl Pts',(0.623873281963166,1.1801260959606,2.3218725925448));
#22617=CARTESIAN_POINT('Ctrl Pts',(0.76341449322476,1.07944244879737,2.31402204150712));
#22618=CARTESIAN_POINT('Ctrl Pts',(0.756401707578768,0.907512694301026,
2.30617149046944));
#22619=CARTESIAN_POINT('Ctrl Pts',(0.609124149502328,0.818527871661859,
2.29832093943176));
#22620=CARTESIAN_POINT('Ctrl Pts',(0.453663838681055,0.892291508258571,
2.29047038839408));
#22621=CARTESIAN_POINT('Ctrl Pts',(0.429441275539409,1.06265071125502,2.28261983735641));
#22622=CARTESIAN_POINT('Ctrl Pts',(0.558179831669208,1.17682325150234,2.27476928631873));
#22623=CARTESIAN_POINT('Ctrl Pts',(0.724423708785572,1.13241650393702,2.26691873528105));
#22624=CARTESIAN_POINT('Ctrl Pts',(0.779081445955335,0.969255483615749,
2.25906818424337));
#22625=CARTESIAN_POINT('Ctrl Pts',(0.673134684925636,0.833666878534013,
2.25121763320569));
#22626=CARTESIAN_POINT('Ctrl Pts',(0.50159899980171,0.84724977008965,2.24336708216802));
#22627=CARTESIAN_POINT('Ctrl Pts',(0.418311670993437,0.997822699786089,
2.23551653113034));
#22628=CARTESIAN_POINT('Ctrl Pts',(0.497966755036121,1.15034828380644,2.22766598009266));
#22629=CARTESIAN_POINT('Ctrl Pts',(0.669127678863374,1.16803795272366,2.21981542905498));
#22630=CARTESIAN_POINT('Ctrl Pts',(0.778293256865801,1.03502719068774,2.21196487801731));
#22631=CARTESIAN_POINT('Ctrl Pts',(0.727561203441069,0.870603211369231,
2.20411432697963));
#22632=CARTESIAN_POINT('Ctrl Pts',(0.562429230156179,0.822225348280642,
2.19626377594195));
#22633=CARTESIAN_POINT('Ctrl Pts',(0.430991616501465,0.933280019269996,
2.18841322490427));
#22634=CARTESIAN_POINT('Ctrl Pts',(0.451124739033006,1.10417075503916,2.18056267386659));
#22635=CARTESIAN_POINT('Ctrl Pts',(0.604772735062981,1.18163868139168,2.17271212282892));
#22636=CARTESIAN_POINT('Ctrl Pts',(0.754140428515542,1.09620871962996,2.16486157179123));
#22637=CARTESIAN_POINT('Ctrl Pts',(0.765271321801097,0.924496491715462,
2.15701102075356));
#22638=CARTESIAN_POINT('Ctrl Pts',(0.628182963406343,0.820497603368372,
2.14916046971588));
#22639=CARTESIAN_POINT('Ctrl Pts',(0.465819455752544,0.877480734998406,
2.1413099186782));
#22640=CARTESIAN_POINT('Ctrl Pts',(0.423792245550112,1.04434204981856,2.13345936764053));
#22641=CARTESIAN_POINT('Ctrl Pts',(0.539792347657613,1.17143637275151,2.12560881660284));
#22642=CARTESIAN_POINT('Ctrl Pts',(0.70978808601476,1.14478245624706,2.11775826556517));
#22643=CARTESIAN_POINT('Ctrl Pts',(0.781323293607615,0.988284239491303,
2.10990771452749));
#22644=CARTESIAN_POINT('Ctrl Pts',(0.690243392316909,0.842292899938004,
2.10205716348982));
#22645=CARTESIAN_POINT('Ctrl Pts',(0.518231205927094,0.837737224374896,
2.09420661245213));
#22646=CARTESIAN_POINT('Ctrl Pts',(0.419550953589664,0.978702295314315,
2.08635606141446));
#22647=CARTESIAN_POINT('Ctrl Pts',(0.482702215643831,1.13876837785338,2.07850551037678));
#22648=CARTESIAN_POINT('Ctrl Pts',(0.651047898079357,1.17438225782416,2.0706549593391));
#22649=CARTESIAN_POINT('Ctrl Pts',(0.773614618887169,1.05360877841752,2.06280440830142));
#22650=CARTESIAN_POINT('Ctrl Pts',(0.740475677832241,0.884752178886651,
2.05495385726374));
#22651=CARTESIAN_POINT('Ctrl Pts',(0.581362560637208,0.819263360725568,
2.04710330622607));
#22652=CARTESIAN_POINT('Ctrl Pts',(0.438948708524181,0.915842240569421,
2.03925275518839));
#22653=CARTESIAN_POINT('Ctrl Pts',(0.440999424005214,1.08793750651601,2.03140220415071));
#22654=CARTESIAN_POINT('Ctrl Pts',(0.585586764715563,1.18108624726655,2.02355165311303));
#22655=CARTESIAN_POINT('Ctrl Pts',(0.74321627607811,1.11199512704675,2.01570110207536));
#22656=CARTESIAN_POINT('Ctrl Pts',(0.772174135599484,0.94213024790789,2.00785055103768));
#22657=CARTESIAN_POINT('Ctrl Pts',(0.688870364005735,0.864039910406678,
2.00261685034589));
#22658=CARTESIAN_POINT('Ctrl Pts',(0.639851384185725,0.850935057178149,
2.));
#22659=CARTESIAN_POINT('Ctrl Pts',(0.695811615272236,1.08252112989365,2.4));
#22660=CARTESIAN_POINT('Ctrl Pts',(0.702493035444011,1.07628157141353,2.4));
#22661=CARTESIAN_POINT('Ctrl Pts',(0.708395708847424,1.0693103556765,2.4));
#22662=CARTESIAN_POINT('Ctrl Pts',(0.713512656958279,1.06178684479855,2.4));
#22663=CARTESIAN_POINT('Ctrl Pts',(0.717502347100726,1.05592075498562,2.4));
#22664=CARTESIAN_POINT('Ctrl Pts',(0.721014082031974,1.04971755619462,2.4));
#22665=CARTESIAN_POINT('Ctrl Pts',(0.724031956062882,1.04324616442023,2.4));
#22666=CARTESIAN_POINT('Ctrl Pts',(0.725329175480596,1.04046446611758,2.4));
#22667=CARTESIAN_POINT('Ctrl Pts',(0.726532629865294,1.03763770614082,2.4));
#22668=CARTESIAN_POINT('Ctrl Pts',(0.727638786465014,1.03477907962968,2.4));
#22669=CARTESIAN_POINT('Ctrl Pts',(0.731192959070153,1.02559407631572,2.4));
#22670=CARTESIAN_POINT('Ctrl Pts',(0.733756217444906,1.01606058770234,2.4));
#22671=CARTESIAN_POINT('Ctrl Pts',(0.735294617481607,1.0063604023791,2.4));
#22672=CARTESIAN_POINT('Ctrl Pts',(0.736007696124321,1.00186417589745,2.4));
#22673=CARTESIAN_POINT('Ctrl Pts',(0.736499990230692,0.997331676100057,
2.4));
#22674=CARTESIAN_POINT('Ctrl Pts',(0.736764649954775,0.992779471200463,
2.4));
#22675=CARTESIAN_POINT('Ctrl Pts',(0.736959071387571,0.989435380209583,
2.4));
#22676=CARTESIAN_POINT('Ctrl Pts',(0.737029983554064,0.98608811988667,2.4));
#22677=CARTESIAN_POINT('Ctrl Pts',(0.736976127631269,0.982751397582665,
2.4));
#22678=CARTESIAN_POINT('Ctrl Pts',(0.736862856230108,0.975733502594741,
2.4));
#22679=CARTESIAN_POINT('Ctrl Pts',(0.736199022212823,0.968753098529686,
2.4));
#22680=CARTESIAN_POINT('Ctrl Pts',(0.73496858294117,0.96187154470407,2.4));
#22681=CARTESIAN_POINT('Ctrl Pts',(0.733610269619415,0.954274821768571,
2.4));
#22682=CARTESIAN_POINT('Ctrl Pts',(0.731561915556015,0.946798108708432,
2.4));
#22683=CARTESIAN_POINT('Ctrl Pts',(0.728883391181877,0.939498503415491,
2.4));
#22684=CARTESIAN_POINT('Ctrl Pts',(0.727748787370213,0.936406442701396,
2.4));
#22685=CARTESIAN_POINT('Ctrl Pts',(0.726503663184753,0.933354104764928,
2.4));
#22686=CARTESIAN_POINT('Ctrl Pts',(0.725155437375267,0.93034965316141,2.4));
#22687=CARTESIAN_POINT('Ctrl Pts',(0.721333520454809,0.921832708641144,
2.4));
#22688=CARTESIAN_POINT('Ctrl Pts',(0.716681958573065,0.913689799617633,
2.4));
#22689=CARTESIAN_POINT('Ctrl Pts',(0.711310080831161,0.906016236422445,
2.4));
#22690=CARTESIAN_POINT('Ctrl Pts',(0.708434311712215,0.901908288116612,
2.4));
#22691=CARTESIAN_POINT('Ctrl Pts',(0.705351471044678,0.897934909331024,
2.4));
#22692=CARTESIAN_POINT('Ctrl Pts',(0.702074477330367,0.894112050103086,
2.4));
#22693=CARTESIAN_POINT('Ctrl Pts',(0.699663413790917,0.891299363444374,
2.4));
#22694=CARTESIAN_POINT('Ctrl Pts',(0.697146509627061,0.888567971784173,
2.4));
#22695=CARTESIAN_POINT('Ctrl Pts',(0.694540211514707,0.885935552211034,
2.4));
#22696=CARTESIAN_POINT('Ctrl Pts',(0.689966981858787,0.881316487645227,
2.4));
#22697=CARTESIAN_POINT('Ctrl Pts',(0.685111586013864,0.876992966093948,
2.4));
#22698=CARTESIAN_POINT('Ctrl Pts',(0.680004164916354,0.87299757664439,2.4));
#22699=CARTESIAN_POINT('Ctrl Pts',(0.67522858856925,0.869261779852135,2.4));
#22700=CARTESIAN_POINT('Ctrl Pts',(0.670227032530533,0.865810208752244,
2.4));
#22701=CARTESIAN_POINT('Ctrl Pts',(0.665049792940119,0.862688960723077,
2.4));
#22702=CARTESIAN_POINT('Ctrl Pts',(0.659173917535639,0.859146519967616,
2.4));
#22703=CARTESIAN_POINT('Ctrl Pts',(0.653067316624201,0.856024693283448,
2.4));
#22704=CARTESIAN_POINT('Ctrl Pts',(0.646761964313973,0.85336416176701,2.4));
#22705=CARTESIAN_POINT('Ctrl Pts',(0.644516614709207,0.852416740735641,
2.4));
#22706=CARTESIAN_POINT('Ctrl Pts',(0.642246009555221,0.851527876023459,
2.4));
#22707=CARTESIAN_POINT('Ctrl Pts',(0.63995226235153,0.850696991672974,2.4));
#22708=CARTESIAN_POINT('Ctrl Pts',(0.473597863174539,0.999893075682974,
2.31934196736194));
#22709=CARTESIAN_POINT('Ctrl Pts',(0.473502307398787,0.988483568548598,
2.32005947478237));
#22710=CARTESIAN_POINT('Ctrl Pts',(0.474923175284874,0.977097443610316,
2.3207769822028));
#22711=CARTESIAN_POINT('Ctrl Pts',(0.477956455981403,0.966158447195516,
2.32149448962322));
#22712=CARTESIAN_POINT('Ctrl Pts',(0.489019256746842,0.926262390741107,
2.32411133996911));
#22713=CARTESIAN_POINT('Ctrl Pts',(0.521529781864938,0.892313874060468,
2.32672819031501));
#22714=CARTESIAN_POINT('Ctrl Pts',(0.5609099425597,0.879535106636999,2.3293450406609));
#22715=CARTESIAN_POINT('Ctrl Pts',(0.600290103254463,0.86675633921353,2.33196189100679));
#22716=CARTESIAN_POINT('Ctrl Pts',(0.646539899525892,0.875147321047232,
2.33457874135269));
#22717=CARTESIAN_POINT('Ctrl Pts',(0.678920339291197,0.90094682938132,2.33719559169858));
#22718=CARTESIAN_POINT('Ctrl Pts',(0.711300779056502,0.926746337715409,
2.33981244204447));
#22719=CARTESIAN_POINT('Ctrl Pts',(0.729811862315683,0.969954372549885,
2.34242929239036));
#22720=CARTESIAN_POINT('Ctrl Pts',(0.726153065466658,1.01119319937947,2.34504614273626));
#22721=CARTESIAN_POINT('Ctrl Pts',(0.722494268617633,1.05243202620905,2.34766299308215));
#22722=CARTESIAN_POINT('Ctrl Pts',(0.696665591660402,1.09170164503374,2.35027984342804));
#22723=CARTESIAN_POINT('Ctrl Pts',(0.6602487903707,1.11139847313147,2.35289669377393));
#22724=CARTESIAN_POINT('Ctrl Pts',(0.623831989080998,1.13109530122919,2.35551354411983));
#22725=CARTESIAN_POINT('Ctrl Pts',(0.576827063458825,1.13121933859995,2.35813039446572));
#22726=CARTESIAN_POINT('Ctrl Pts',(0.540311835838483,1.11170438861103,2.36074724481161));
#22727=CARTESIAN_POINT('Ctrl Pts',(0.503796608218141,1.09218943862212,2.3633640951575));
#22728=CARTESIAN_POINT('Ctrl Pts',(0.477771078599631,1.05303550127352,2.3659809455034));
#22729=CARTESIAN_POINT('Ctrl Pts',(0.473904908648346,1.01182047020411,2.36859779584929));
#22730=CARTESIAN_POINT('Ctrl Pts',(0.473538425642629,1.00791360406595,2.36884585302017));
#22731=CARTESIAN_POINT('Ctrl Pts',(0.473371057191087,1.00398821781876,2.36909391019106));
#22732=CARTESIAN_POINT('Ctrl Pts',(0.473395817154925,1.00006080538999,2.36934196736194));
#22733=CARTESIAN_POINT('Ctrl Pts',(0.560148615814278,0.850935057178148,
2.4));
#22734=CARTESIAN_POINT('Ctrl Pts',(0.511129635994267,0.864039910406677,
2.39738314965411));
#22735=CARTESIAN_POINT('Ctrl Pts',(0.427825810157124,0.942129912787787,
2.39214944896232));
#22736=CARTESIAN_POINT('Ctrl Pts',(0.456783771264579,1.11199528864852,2.38429889792464));
#22737=CARTESIAN_POINT('Ctrl Pts',(0.614413228882944,1.18108612135922,2.37644834688697));
#22738=CARTESIAN_POINT('Ctrl Pts',(0.759000551270414,1.08793755388759,2.36859779584929));
#22739=CARTESIAN_POINT('Ctrl Pts',(0.761051274433651,0.91584221771742,2.36074724481161));
#22740=CARTESIAN_POINT('Ctrl Pts',(0.618637433005314,0.819263404514795,
2.35289669377393));
#22741=CARTESIAN_POINT('Ctrl Pts',(0.459524343787705,0.884752183415202,
2.34504614273626));
#22742=CARTESIAN_POINT('Ctrl Pts',(0.426385402694383,1.05360877733288,2.33719559169858));
#22743=CARTESIAN_POINT('Ctrl Pts',(0.548952109888326,1.17438223097154,2.3293450406609));
#22744=CARTESIAN_POINT('Ctrl Pts',(0.717297767916034,1.1387683610531,2.32149448962322));
#22745=CARTESIAN_POINT('Ctrl Pts',(0.780449022522885,0.978702297157564,
2.31364393858554));
#22746=CARTESIAN_POINT('Ctrl Pts',(0.681768782849741,0.837737246759644,
2.30579338754786));
#22747=CARTESIAN_POINT('Ctrl Pts',(0.509756619949943,0.842292920851884,
2.29794283651019));
#22748=CARTESIAN_POINT('Ctrl Pts',(0.418676730713559,0.988284241230286,
2.29009228547251));
#22749=CARTESIAN_POINT('Ctrl Pts',(0.490211928794195,1.14478243668251,2.28224173443483));
#22750=CARTESIAN_POINT('Ctrl Pts',(0.660207644220989,1.17143634973614,2.27439118339715));
#22751=CARTESIAN_POINT('Ctrl Pts',(0.776207730757634,1.04434204382826,2.26654063235948));
#22752=CARTESIAN_POINT('Ctrl Pts',(0.734180526190243,0.87748075149375,2.2586900813218));
#22753=CARTESIAN_POINT('Ctrl Pts',(0.571817040388558,0.820497627508739,
2.25083953028412));
#22754=CARTESIAN_POINT('Ctrl Pts',(0.434728700430063,0.92449650187637,2.24298897924644));
#22755=CARTESIAN_POINT('Ctrl Pts',(0.445859592221225,1.09620870668547,2.23513842820877));
#22756=CARTESIAN_POINT('Ctrl Pts',(0.595227265578502,1.18163865695784,2.22728787717108));
#22757=CARTESIAN_POINT('Ctrl Pts',(0.748875240939872,1.10417074102503,2.21943732613341));
#22758=CARTESIAN_POINT('Ctrl Pts',(0.769008360762544,0.933280028245809,
2.21158677509573));
#22759=CARTESIAN_POINT('Ctrl Pts',(0.637570764789711,0.822225372195567,
2.20373622405805));
#22760=CARTESIAN_POINT('Ctrl Pts',(0.472438813719035,0.870603228776448,
2.19588567302037));
#22761=CARTESIAN_POINT('Ctrl Pts',(0.421706767119107,1.03502718597557,2.1880351219827));
#22762=CARTESIAN_POINT('Ctrl Pts',(0.530872330435983,1.16803793011858,2.18018457094502));
#22763=CARTESIAN_POINT('Ctrl Pts',(0.702033231237909,1.1503482635805,2.17233401990734));
#22764=CARTESIAN_POINT('Ctrl Pts',(0.781688304564893,0.997822700079642,
2.16448346886966));
#22765=CARTESIAN_POINT('Ctrl Pts',(0.698400986961052,0.847249790637147,
2.15663291783198));
#22766=CARTESIAN_POINT('Ctrl Pts',(0.526865324912526,0.833666900912216,
2.14878236679431));
#22767=CARTESIAN_POINT('Ctrl Pts',(0.420918578136115,0.969255487747401,
2.14093181575663));
#22768=CARTESIAN_POINT('Ctrl Pts',(0.475576307951429,1.13241648613165,2.13308126471895));
#22769=CARTESIAN_POINT('Ctrl Pts',(0.641820162707069,1.17682322770038,2.12523071368128));
#22770=CARTESIAN_POINT('Ctrl Pts',(0.770558701511974,1.06265070285456,2.11738016264359));
#22771=CARTESIAN_POINT('Ctrl Pts',(0.746336141641471,0.892291522696776,
2.10952961160592));
#22772=CARTESIAN_POINT('Ctrl Pts',(0.590875851708506,0.818527896169216,
2.10167906056824));
#22773=CARTESIAN_POINT('Ctrl Pts',(0.443598313494032,0.907512706568079,
2.09382850953057));
#22774=CARTESIAN_POINT('Ctrl Pts',(0.436585528693405,1.07944243843108,2.08597795849288));
#22775=CARTESIAN_POINT('Ctrl Pts',(0.57612672137744,1.18012607114374,2.07812740745521));
#22776=CARTESIAN_POINT('Ctrl Pts',(0.737078048375186,1.11926881624917,2.07027685641753));
#22777=CARTESIAN_POINT('Ctrl Pts',(0.775094502137202,0.951447557128672,
2.06242630537985));
#22778=CARTESIAN_POINT('Ctrl Pts',(0.656082084236305,0.827171040068,2.05457575434217));
#22779=CARTESIAN_POINT('Ctrl Pts',(0.48677384037764,0.857888191265152,2.04672520330449));
#22780=CARTESIAN_POINT('Ctrl Pts',(0.419009664523655,1.01606137229499,2.03887465226682));
#22781=CARTESIAN_POINT('Ctrl Pts',(0.513561617374857,1.15981701056446,2.03102410122914));
#22782=CARTESIAN_POINT('Ctrl Pts',(0.685634169421134,1.1602711276025,2.02317355019146));
#22783=CARTESIAN_POINT('Ctrl Pts',(0.780906782004492,1.01693885807272,2.01532299915378));
#22784=CARTESIAN_POINT('Ctrl Pts',(0.713940171081941,0.858516566589665,
2.0074724481161));
#22785=CARTESIAN_POINT('Ctrl Pts',(0.544785272473601,0.826780004858426,
1.99962189707843));
#22786=CARTESIAN_POINT('Ctrl Pts',(0.425151261024703,0.95079820002532,1.99177134604075));
#22787=CARTESIAN_POINT('Ctrl Pts',(0.449973151490716,1.0622497573257,1.98653764534896));
#22788=CARTESIAN_POINT('Ctrl Pts',(0.483086340557483,1.10069600903591,1.98392079500307));
#22789=CARTESIAN_POINT('Ctrl Pts',(0.562546241758482,0.859903427576914,
2.40535973499898));
#22790=CARTESIAN_POINT('Ctrl Pts',(0.516476448777934,0.872219838026409,
2.40274288465309));
#22791=CARTESIAN_POINT('Ctrl Pts',(0.438184529507143,0.945611619266206,
2.3975091839613));
#22792=CARTESIAN_POINT('Ctrl Pts',(0.46540025856266,1.1052571836823,2.38965863292362));
#22793=CARTESIAN_POINT('Ctrl Pts',(0.613546068752483,1.17019122293655,2.38180808188594));
#22794=CARTESIAN_POINT('Ctrl Pts',(0.749434413113403,1.08264686286195,2.37395753084827));
#22795=CARTESIAN_POINT('Ctrl Pts',(0.751361756194339,0.920905501875057,
2.36610697981059));
#22796=CARTESIAN_POINT('Ctrl Pts',(0.617516127087842,0.830137273999053,
2.35825642877291));
#22797=CARTESIAN_POINT('Ctrl Pts',(0.467975946780819,0.891685974065206,
2.35040587773523));
#22798=CARTESIAN_POINT('Ctrl Pts',(0.436830782981619,1.050383449079,2.34255532669756));
#22799=CARTESIAN_POINT('Ctrl Pts',(0.552023364456505,1.16389066663247,2.33470477565987));
#22800=CARTESIAN_POINT('Ctrl Pts',(0.710240643620372,1.13041947607723,2.3268542246222));
#22801=CARTESIAN_POINT('Ctrl Pts',(0.769592454630765,0.979983656034563,
2.31900367358452));
#22802=CARTESIAN_POINT('Ctrl Pts',(0.676849230889565,0.847499652630768,
2.31115312254684));
#22803=CARTESIAN_POINT('Ctrl Pts',(0.515186039121242,0.851781238316293,
2.30330257150916));
#22804=CARTESIAN_POINT('Ctrl Pts',(0.429585896947362,0.988989110277028,
2.29545202047149));
#22805=CARTESIAN_POINT('Ctrl Pts',(0.496817238327747,1.13607171976393,2.28760146943381));
#22806=CARTESIAN_POINT('Ctrl Pts',(0.65658530053649,1.16112202193283,2.27975091839613));
#22807=CARTESIAN_POINT('Ctrl Pts',(0.765606336716589,1.04167424101854,2.27190036735845));
#22808=CARTESIAN_POINT('Ctrl Pts',(0.726107664547559,0.884852021899667,
2.26404981632077));
#22809=CARTESIAN_POINT('Ctrl Pts',(0.573512645109186,0.831297240975754,
2.2561992652831));
#22810=CARTESIAN_POINT('Ctrl Pts',(0.444672113031105,0.929039108103942,
2.24834871424542));
#22811=CARTESIAN_POINT('Ctrl Pts',(0.455133323819063,1.09042038851482,2.24049816320774));
#22812=CARTESIAN_POINT('Ctrl Pts',(0.595514413242444,1.17071051568267,2.23264761217006));
#22813=CARTESIAN_POINT('Ctrl Pts',(0.739918283799722,1.09790339356867,2.22479706113239));
#22814=CARTESIAN_POINT('Ctrl Pts',(0.758840110930535,0.9372941807914,2.21694651009471));
#22815=CARTESIAN_POINT('Ctrl Pts',(0.635310350446671,0.832921037316226,
2.20909595905703));
#22816=CARTESIAN_POINT('Ctrl Pts',(0.480113428188521,0.878388279713101,
2.20124540801935));
#22817=CARTESIAN_POINT('Ctrl Pts',(0.432433633690143,1.03291980397207,2.19339485698167));
#22818=CARTESIAN_POINT('Ctrl Pts',(0.535031340151599,1.15792806545277,2.185544305944));
#22819=CARTESIAN_POINT('Ctrl Pts',(0.695894485310114,1.14130268323763,2.17769375490632));
#22820=CARTESIAN_POINT('Ctrl Pts',(0.770757176282041,0.997953695549035,
2.16984320386864));
#22821=CARTESIAN_POINT('Ctrl Pts',(0.692480772040193,0.856439882084015,
2.16199265283096));
#22822=CARTESIAN_POINT('Ctrl Pts',(0.531265412839046,0.843674195813048,
2.15414210179328));
#22823=CARTESIAN_POINT('Ctrl Pts',(0.431692865452835,0.971105206188175,
2.1462915507556));
#22824=CARTESIAN_POINT('Ctrl Pts',(0.483062157645861,1.12444975651669,2.13844099971793));
#22825=CARTESIAN_POINT('Ctrl Pts',(0.639304086812941,1.16618480278905,2.13059044868025));
#22826=CARTESIAN_POINT('Ctrl Pts',(0.760297176696446,1.05888137454499,2.12273989764257));
#22827=CARTESIAN_POINT('Ctrl Pts',(0.73753194733446,0.898771715163604,2.11488934660489));
#22828=CARTESIAN_POINT('Ctrl Pts',(0.591424798629911,0.829446016911682,
2.10703879556722));
#22829=CARTESIAN_POINT('Ctrl Pts',(0.453008093077508,0.913077128953215,
2.09918824452954));
#22830=CARTESIAN_POINT('Ctrl Pts',(0.44641722674026,1.07466284908066,2.09133769349186));
#22831=CARTESIAN_POINT('Ctrl Pts',(0.577563037665274,1.16928893335727,2.08348714245418));
#22832=CARTESIAN_POINT('Ctrl Pts',(0.728830859679466,1.11209310544222,2.0756365914165));
#22833=CARTESIAN_POINT('Ctrl Pts',(0.76456008458585,0.954368675154091,2.06778604037883));
#22834=CARTESIAN_POINT('Ctrl Pts',(0.652707951494933,0.837569153125047,
2.05993548934115));
#22835=CARTESIAN_POINT('Ctrl Pts',(0.493585999689548,0.866438232036949,
2.05208493830347));
#22836=CARTESIAN_POINT('Ctrl Pts',(0.429898800067004,1.01509505296379,2.04423438726579));
#22837=CARTESIAN_POINT('Ctrl Pts',(0.518762111987321,1.15020175080161,2.03638383622811));
#22838=CARTESIAN_POINT('Ctrl Pts',(0.680482059638507,1.15062854625939,2.02853328519044));
#22839=CARTESIAN_POINT('Ctrl Pts',(0.770022673387457,1.01591974552719,2.02068273415276));
#22840=CARTESIAN_POINT('Ctrl Pts',(0.707085053854394,0.867028801673869,
2.01283218311508));
#22841=CARTESIAN_POINT('Ctrl Pts',(0.548107221407733,0.837201644229118,
2.0049816320774));
#22842=CARTESIAN_POINT('Ctrl Pts',(0.435670892436373,0.953758386089901,
1.99713108103972));
#22843=CARTESIAN_POINT('Ctrl Pts',(0.458999394158644,1.05850455157603,1.99189738034794));
#22844=CARTESIAN_POINT('Ctrl Pts',(0.490120355280909,1.09463771598849,1.98928053000205));
#22845=CARTESIAN_POINT('Ctrl Pts',(0.564943867702687,0.868871797975679,
2.41071946999795));
#22846=CARTESIAN_POINT('Ctrl Pts',(0.521823261561601,0.880399765646142,
2.40810261965206));
#22847=CARTESIAN_POINT('Ctrl Pts',(0.448543248857163,0.949093325744624,
2.40286891896027));
#22848=CARTESIAN_POINT('Ctrl Pts',(0.474016745860739,1.09851907871609,2.3950183679226));
#22849=CARTESIAN_POINT('Ctrl Pts',(0.612678908622024,1.15929632451388,2.38716781688491));
#22850=CARTESIAN_POINT('Ctrl Pts',(0.739868274956389,1.07735617183631,2.37931726584725));
#22851=CARTESIAN_POINT('Ctrl Pts',(0.741672237955028,0.925968786032693,
2.37146671480956));
#22852=CARTESIAN_POINT('Ctrl Pts',(0.616394821170369,0.841011143483312,
2.36361616377189));
#22853=CARTESIAN_POINT('Ctrl Pts',(0.476427549773933,0.898619764715207,
2.35576561273421));
#22854=CARTESIAN_POINT('Ctrl Pts',(0.447276163268855,1.04715812082513,2.34791506169653));
#22855=CARTESIAN_POINT('Ctrl Pts',(0.555094619024684,1.15339910229339,2.34006451065885));
#22856=CARTESIAN_POINT('Ctrl Pts',(0.703183519324712,1.12207059110137,2.33221395962117));
#22857=CARTESIAN_POINT('Ctrl Pts',(0.758735886738644,0.981265014911558,
2.3243634085835));
#22858=CARTESIAN_POINT('Ctrl Pts',(0.67192967892939,0.857262058501895,2.31651285754582));
#22859=CARTESIAN_POINT('Ctrl Pts',(0.52061545829254,0.861269555780702,2.30866230650814));
#22860=CARTESIAN_POINT('Ctrl Pts',(0.440495063181165,0.989693979323769,
2.30081175547046));
#22861=CARTESIAN_POINT('Ctrl Pts',(0.5034225478613,1.12736100284536,2.29296120443278));
#22862=CARTESIAN_POINT('Ctrl Pts',(0.652962956851991,1.15080769412952,2.28511065339511));
#22863=CARTESIAN_POINT('Ctrl Pts',(0.755004942675543,1.03900643820883,2.27726010235743));
#22864=CARTESIAN_POINT('Ctrl Pts',(0.718034802904875,0.892223292305585,
2.26940955131975));
#22865=CARTESIAN_POINT('Ctrl Pts',(0.575208249829814,0.84209685444277,2.26155900028207));
#22866=CARTESIAN_POINT('Ctrl Pts',(0.454615525632148,0.933581714331513,
2.25370844924439));
#22867=CARTESIAN_POINT('Ctrl Pts',(0.4644070554169,1.08463207034418,2.24585789820672));
#22868=CARTESIAN_POINT('Ctrl Pts',(0.595801560906386,1.1597823744075,2.23800734716904));
#22869=CARTESIAN_POINT('Ctrl Pts',(0.730961326659572,1.09163604611232,2.23015679613136));
#22870=CARTESIAN_POINT('Ctrl Pts',(0.748671861098526,0.941308333336992,
2.22230624509368));
#22871=CARTESIAN_POINT('Ctrl Pts',(0.63304993610363,0.843616702436886,2.214455694056));
#22872=CARTESIAN_POINT('Ctrl Pts',(0.487788042658006,0.886173330649751,
2.20660514301833));
#22873=CARTESIAN_POINT('Ctrl Pts',(0.443160500261181,1.03081242196857,2.19875459198065));
#22874=CARTESIAN_POINT('Ctrl Pts',(0.539190349867211,1.14781820078696,2.19090404094297));
#22875=CARTESIAN_POINT('Ctrl Pts',(0.689755739382323,1.13225710289476,2.18305348990529));
#22876=CARTESIAN_POINT('Ctrl Pts',(0.759826047999188,0.998084691018425,
2.17520293886762));
#22877=CARTESIAN_POINT('Ctrl Pts',(0.686560557119336,0.865629973530885,
2.16735238782994));
#22878=CARTESIAN_POINT('Ctrl Pts',(0.535665500765565,0.853681490713878,
2.15950183679226));
#22879=CARTESIAN_POINT('Ctrl Pts',(0.442467152769555,0.972954924628952,
2.15165128575459));
#22880=CARTESIAN_POINT('Ctrl Pts',(0.490548007340293,1.11648302690173,2.1438007347169));
#22881=CARTESIAN_POINT('Ctrl Pts',(0.636788010918814,1.15554637787772,2.13595018367923));
#22882=CARTESIAN_POINT('Ctrl Pts',(0.750035651880915,1.05511204623542,2.12809963264155));
#22883=CARTESIAN_POINT('Ctrl Pts',(0.728727753027451,0.905251907630433,
2.12024908160387));
#22884=CARTESIAN_POINT('Ctrl Pts',(0.591973745551315,0.840364137654146,
2.11239853056619));
#22885=CARTESIAN_POINT('Ctrl Pts',(0.462417872660985,0.918641551338351,
2.10454797952851));
#22886=CARTESIAN_POINT('Ctrl Pts',(0.456248924787112,1.06988325973025,2.09669742849084));
#22887=CARTESIAN_POINT('Ctrl Pts',(0.578999353953109,1.15845179557081,2.08884687745316));
#22888=CARTESIAN_POINT('Ctrl Pts',(0.720583670983745,1.10491739463527,2.08099632641548));
#22889=CARTESIAN_POINT('Ctrl Pts',(0.754025667034497,0.957289793179509,
2.0731457753778));
#22890=CARTESIAN_POINT('Ctrl Pts',(0.649333818753561,0.847967266182092,
2.06529522434013));
#22891=CARTESIAN_POINT('Ctrl Pts',(0.500398159001457,0.874988272808748,
2.05744467330245));
#22892=CARTESIAN_POINT('Ctrl Pts',(0.440787935610353,1.01412873363258,2.04959412226477));
#22893=CARTESIAN_POINT('Ctrl Pts',(0.523962606599787,1.14058649103877,2.04174357122709));
#22894=CARTESIAN_POINT('Ctrl Pts',(0.675329949855879,1.14098596491627,2.03389302018941));
#22895=CARTESIAN_POINT('Ctrl Pts',(0.759138564770422,1.01490063298166,2.02604246915174));
#22896=CARTESIAN_POINT('Ctrl Pts',(0.700229936626846,0.875541036758072,
2.01819191811406));
#22897=CARTESIAN_POINT('Ctrl Pts',(0.551429170341866,0.847623283599809,
2.01034136707638));
#22898=CARTESIAN_POINT('Ctrl Pts',(0.446190523848043,0.956718572154482,
2.0024908160387));
#22899=CARTESIAN_POINT('Ctrl Pts',(0.468025636826571,1.05475934582637,1.99725711534692));
#22900=CARTESIAN_POINT('Ctrl Pts',(0.497154370004336,1.08857942294107,1.99464026500102));
#22901=CARTESIAN_POINT('Ctrl Pts',(0.567341493646892,0.877840168374445,
2.41607920499693));
#22902=CARTESIAN_POINT('Ctrl Pts',(0.527170074345269,0.888579693265874,
2.41346235465104));
#22903=CARTESIAN_POINT('Ctrl Pts',(0.458901968207183,0.952575032223043,
2.40822865395925));
#22904=CARTESIAN_POINT('Ctrl Pts',(0.482633233158821,1.09178097374987,2.40037810292158));
#22905=CARTESIAN_POINT('Ctrl Pts',(0.611811748491563,1.14840142609121,2.3925275518839));
#22906=CARTESIAN_POINT('Ctrl Pts',(0.730302136799378,1.07206548081067,2.38467700084622));
#22907=CARTESIAN_POINT('Ctrl Pts',(0.731982719715716,0.931032070190328,
2.37682644980854));
#22908=CARTESIAN_POINT('Ctrl Pts',(0.615273515252898,0.85188501296757,2.36897589877086));
#22909=CARTESIAN_POINT('Ctrl Pts',(0.484879152767046,0.905553555365211,
2.36112534773319));
#22910=CARTESIAN_POINT('Ctrl Pts',(0.457721543556091,1.04393279257125,2.35327479669551));
#22911=CARTESIAN_POINT('Ctrl Pts',(0.558165873592863,1.14290753795432,2.34542424565783));
#22912=CARTESIAN_POINT('Ctrl Pts',(0.69612639502905,1.1137217061255,2.33757369462015));
#22913=CARTESIAN_POINT('Ctrl Pts',(0.747879318846525,0.982546373788555,
2.32972314358248));
#22914=CARTESIAN_POINT('Ctrl Pts',(0.667010126969215,0.86702446437302,2.32187259254479));
#22915=CARTESIAN_POINT('Ctrl Pts',(0.526044877463838,0.870757873245112,
2.31402204150712));
#22916=CARTESIAN_POINT('Ctrl Pts',(0.451404229414968,0.99039884837051,2.30617149046944));
#22917=CARTESIAN_POINT('Ctrl Pts',(0.510027857394853,1.11865028592679,2.29832093943177));
#22918=CARTESIAN_POINT('Ctrl Pts',(0.649340613167492,1.14049336632621,2.29047038839408));
#22919=CARTESIAN_POINT('Ctrl Pts',(0.744403548634497,1.03633863539911,2.28261983735641));
#22920=CARTESIAN_POINT('Ctrl Pts',(0.709961941262192,0.899594562711502,
2.27476928631873));
#22921=CARTESIAN_POINT('Ctrl Pts',(0.576903854550442,0.852896467909786,
2.26691873528105));
#22922=CARTESIAN_POINT('Ctrl Pts',(0.464558938233191,0.938124320559086,
2.25906818424337));
#22923=CARTESIAN_POINT('Ctrl Pts',(0.473680787014737,1.07884375217354,2.2512176332057));
#22924=CARTESIAN_POINT('Ctrl Pts',(0.596088708570328,1.14885423313233,2.24336708216801));
#22925=CARTESIAN_POINT('Ctrl Pts',(0.722004369519422,1.08536869865596,2.23551653113034));
#22926=CARTESIAN_POINT('Ctrl Pts',(0.738503611266517,0.945322485882583,
2.22766598009266));
#22927=CARTESIAN_POINT('Ctrl Pts',(0.63078952176059,0.854312367557547,2.21981542905498));
#22928=CARTESIAN_POINT('Ctrl Pts',(0.495462657127491,0.893958381586401,
2.21196487801731));
#22929=CARTESIAN_POINT('Ctrl Pts',(0.453887366832218,1.02870503996507,2.20411432697962));
#22930=CARTESIAN_POINT('Ctrl Pts',(0.543349359582825,1.13770833612116,2.19626377594195));
#22931=CARTESIAN_POINT('Ctrl Pts',(0.683616993454529,1.12321152255188,2.18841322490427));
#22932=CARTESIAN_POINT('Ctrl Pts',(0.748894919716335,0.998215686487819,
2.18056267386659));
#22933=CARTESIAN_POINT('Ctrl Pts',(0.680640342198477,0.874820064977753,
2.17271212282892));
#22934=CARTESIAN_POINT('Ctrl Pts',(0.540065588692086,0.863688785614711,
2.16486157179124));
#22935=CARTESIAN_POINT('Ctrl Pts',(0.453241440086272,0.974804643069725,
2.15701102075356));
#22936=CARTESIAN_POINT('Ctrl Pts',(0.498033857034726,1.10851629728676,2.14916046971588));
#22937=CARTESIAN_POINT('Ctrl Pts',(0.634271935024686,1.14490795296639,2.1413099186782));
#22938=CARTESIAN_POINT('Ctrl Pts',(0.739774127065386,1.05134271792586,2.13345936764053));
#22939=CARTESIAN_POINT('Ctrl Pts',(0.719923558720441,0.911732100097261,
2.12560881660285));
#22940=CARTESIAN_POINT('Ctrl Pts',(0.592522692472719,0.851282258396612,
2.11775826556517));
#22941=CARTESIAN_POINT('Ctrl Pts',(0.471827652244461,0.924205973723485,
2.10990771452749));
#22942=CARTESIAN_POINT('Ctrl Pts',(0.466080622833967,1.06510367037984,2.10205716348981));
#22943=CARTESIAN_POINT('Ctrl Pts',(0.580435670240942,1.14761465778435,2.09420661245214));
#22944=CARTESIAN_POINT('Ctrl Pts',(0.712336482288025,1.09774168382831,2.08635606141445));
#22945=CARTESIAN_POINT('Ctrl Pts',(0.743491249483144,0.960210911204929,
2.07850551037678));
#22946=CARTESIAN_POINT('Ctrl Pts',(0.645959686012189,0.858365379239137,
2.0706549593391));
#22947=CARTESIAN_POINT('Ctrl Pts',(0.507210318313367,0.883538313580547,
2.06280440830142));
#22948=CARTESIAN_POINT('Ctrl Pts',(0.451677071153702,1.01316241430137,2.05495385726375));
#22949=CARTESIAN_POINT('Ctrl Pts',(0.529163101212253,1.13097123127593,2.04710330622607));
#22950=CARTESIAN_POINT('Ctrl Pts',(0.670177840073251,1.13134338357315,2.03925275518839));
#22951=CARTESIAN_POINT('Ctrl Pts',(0.748254456153389,1.01388152043613,2.03140220415071));
#22952=CARTESIAN_POINT('Ctrl Pts',(0.693374819399297,0.884053271842277,
2.02355165311304));
#22953=CARTESIAN_POINT('Ctrl Pts',(0.554751119276,0.858044922970499,2.01570110207535));
#22954=CARTESIAN_POINT('Ctrl Pts',(0.456710155259713,0.959678758219065,
2.00785055103768));
#22955=CARTESIAN_POINT('Ctrl Pts',(0.477051879494498,1.0510141400767,2.00261685034589));
#22956=CARTESIAN_POINT('Ctrl Pts',(0.504188384727762,1.08252112989365,2.));
#22957=CARTESIAN_POINT('Ctrl Pts',(0.473630671680838,1.00010094048498,2.35565803263806));
#22958=CARTESIAN_POINT('Ctrl Pts',(0.473532439388447,1.01274184176985,2.35486362065721));
#22959=CARTESIAN_POINT('Ctrl Pts',(0.475280523076927,1.02535622997532,2.35406920867636));
#22960=CARTESIAN_POINT('Ctrl Pts',(0.478988533430712,1.03736537726742,2.35327479669551));
#22961=CARTESIAN_POINT('Ctrl Pts',(0.491202986901682,1.0769243743656,2.35065794634962));
#22962=CARTESIAN_POINT('Ctrl Pts',(0.524684430247273,1.10991595615996,2.34804109600373));
#22963=CARTESIAN_POINT('Ctrl Pts',(0.564418572159433,1.12154744175234,2.34542424565783));
#22964=CARTESIAN_POINT('Ctrl Pts',(0.604152714071593,1.13317892734471,2.34280739531194));
#22965=CARTESIAN_POINT('Ctrl Pts',(0.650139554550321,1.12345031673511,2.34019054496604));
#22966=CARTESIAN_POINT('Ctrl Pts',(0.681758462092598,1.09672345604081,2.33757369462015));
#22967=CARTESIAN_POINT('Ctrl Pts',(0.713377369634875,1.06999659534652,2.33495684427426));
#22968=CARTESIAN_POINT('Ctrl Pts',(0.7306283442407,1.02627148456754,2.33233999392837));
#22969=CARTESIAN_POINT('Ctrl Pts',(0.725775632897394,0.98515527760879,2.32972314358247));
#22970=CARTESIAN_POINT('Ctrl Pts',(0.720922921554088,0.944039070650043,
2.32710629323658));
#22971=CARTESIAN_POINT('Ctrl Pts',(0.693966524261651,0.905531767511531,
2.32448944289069));
#22972=CARTESIAN_POINT('Ctrl Pts',(0.656994117364537,0.886900350754291,
2.32187259254479));
#22973=CARTESIAN_POINT('Ctrl Pts',(0.620021710467422,0.86826893399705,2.3192557421989));
#22974=CARTESIAN_POINT('Ctrl Pts',(0.57303329396563,0.869513403621081,2.31663889185301));
#22975=CARTESIAN_POINT('Ctrl Pts',(0.537098977706589,0.890075800953996,
2.31402204150712));
#22976=CARTESIAN_POINT('Ctrl Pts',(0.501164661447548,0.910638198286911,
2.31140519116123));
#22977=CARTESIAN_POINT('Ctrl Pts',(0.476284445431258,0.95051852332871,2.30878834081533));
#22978=CARTESIAN_POINT('Ctrl Pts',(0.473614942086427,0.991833925442323,
2.30617149046944));
#22979=CARTESIAN_POINT('Ctrl Pts',(0.4734403457566,0.99453612006154,2.30600033785898));
#22980=CARTESIAN_POINT('Ctrl Pts',(0.4733607599644,0.997244453495218,2.30582918524852));
#22981=CARTESIAN_POINT('Ctrl Pts',(0.473373733146151,0.999953562449677,
2.30565803263806));
#22982=CARTESIAN_POINT('Ctrl Pts',(0.560148615814278,0.850935057178148,
2.4));
#22983=CARTESIAN_POINT('Ctrl Pts',(0.550119440006157,0.854599676739477,
2.4));
#22984=CARTESIAN_POINT('Ctrl Pts',(0.540564996368976,0.859362632124605,
2.4));
#22985=CARTESIAN_POINT('Ctrl Pts',(0.531596820053353,0.865074091447543,
2.4));
#22986=CARTESIAN_POINT('Ctrl Pts',(0.527131647122934,0.867917774785653,
2.4));
#22987=CARTESIAN_POINT('Ctrl Pts',(0.522812231247153,0.870997309268362,
2.4));
#22988=CARTESIAN_POINT('Ctrl Pts',(0.518655594653448,0.874297505825464,
2.4));
#22989=CARTESIAN_POINT('Ctrl Pts',(0.515850253684945,0.876524829864272,
2.4));
#22990=CARTESIAN_POINT('Ctrl Pts',(0.513119107067925,0.878852705294647,
2.4));
#22991=CARTESIAN_POINT('Ctrl Pts',(0.510468112479774,0.881276804671575,
2.4));
#22992=CARTESIAN_POINT('Ctrl Pts',(0.508096911905004,0.883445057244236,
2.4));
#22993=CARTESIAN_POINT('Ctrl Pts',(0.505796540173907,0.885684216423859,
2.4));
#22994=CARTESIAN_POINT('Ctrl Pts',(0.503571411911721,0.887989047157772,
2.4));
#22995=CARTESIAN_POINT('Ctrl Pts',(0.496344342241171,0.895474985193744,
2.4));
#22996=CARTESIAN_POINT('Ctrl Pts',(0.489902891057215,0.903656331605307,
2.4));
#22997=CARTESIAN_POINT('Ctrl Pts',(0.484380306519488,0.912413061717332,
2.4));
#22998=CARTESIAN_POINT('Ctrl Pts',(0.482085857904318,0.91605118932619,2.4));
#22999=CARTESIAN_POINT('Ctrl Pts',(0.479950575517979,0.919788877767087,
2.4));
#23000=CARTESIAN_POINT('Ctrl Pts',(0.477986676370491,0.923618156800881,
2.4));
#23001=CARTESIAN_POINT('Ctrl Pts',(0.476502903437523,0.92651126900086,2.4));
#23002=CARTESIAN_POINT('Ctrl Pts',(0.475117212818011,0.929456979534617,
2.4));
#23003=CARTESIAN_POINT('Ctrl Pts',(0.473840374483033,0.932438138949923,
2.4));
#23004=CARTESIAN_POINT('Ctrl Pts',(0.470678069804683,0.939821481153613,
2.4));
#23005=CARTESIAN_POINT('Ctrl Pts',(0.468171071299299,0.947441891244077,
2.4));
#23006=CARTESIAN_POINT('Ctrl Pts',(0.466390209012142,0.955243589562609,
2.4));
#23007=CARTESIAN_POINT('Ctrl Pts',(0.464752055683344,0.962420100718438,
2.4));
#23008=CARTESIAN_POINT('Ctrl Pts',(0.46372877679908,0.9697505149636,2.4));
#23009=CARTESIAN_POINT('Ctrl Pts',(0.463308980593947,0.977159382735458,
2.4));
#23010=CARTESIAN_POINT('Ctrl Pts',(0.463132836556449,0.980268100410063,
2.4));
#23011=CARTESIAN_POINT('Ctrl Pts',(0.463063518093533,0.983387131233213,
2.4));
#23012=CARTESIAN_POINT('Ctrl Pts',(0.463099417336848,0.986501004293148,
2.4));
#23013=CARTESIAN_POINT('Ctrl Pts',(0.463196741723633,0.994942847577307,
2.4));
#23014=CARTESIAN_POINT('Ctrl Pts',(0.464064109534936,1.00336872849097,2.4));
#23015=CARTESIAN_POINT('Ctrl Pts',(0.46567545593174,1.01166502412979,2.4));
#23016=CARTESIAN_POINT('Ctrl Pts',(0.466871287371351,1.0178219691398,2.4));
#23017=CARTESIAN_POINT('Ctrl Pts',(0.468477485851221,1.02390757093803,2.4));
#23018=CARTESIAN_POINT('Ctrl Pts',(0.47049181446679,1.02987017308613,2.4));
#23019=CARTESIAN_POINT('Ctrl Pts',(0.471677008778134,1.0333784597143,2.4));
#23020=CARTESIAN_POINT('Ctrl Pts',(0.473001300296321,1.03683670710464,2.4));
#23021=CARTESIAN_POINT('Ctrl Pts',(0.474460926720988,1.04022911545352,2.4));
#23022=CARTESIAN_POINT('Ctrl Pts',(0.476751356878834,1.04555244631317,2.4));
#23023=CARTESIAN_POINT('Ctrl Pts',(0.479376309757289,1.05071849279536,2.4));
#23024=CARTESIAN_POINT('Ctrl Pts',(0.482333049272134,1.05568492650343,2.4));
#23025=CARTESIAN_POINT('Ctrl Pts',(0.48437450467299,1.05911395799755,2.4));
#23026=CARTESIAN_POINT('Ctrl Pts',(0.486574676429565,1.06244757032586,2.4));
#23027=CARTESIAN_POINT('Ctrl Pts',(0.4889242778747,1.06565919855071,2.4));
#23028=CARTESIAN_POINT('Ctrl Pts',(0.492216707071327,1.07015956117947,2.4));
#23029=CARTESIAN_POINT('Ctrl Pts',(0.495805971455815,1.07442716938164,2.4));
#23030=CARTESIAN_POINT('Ctrl Pts',(0.499690943915119,1.07842077967776,2.4));
#23031=CARTESIAN_POINT('Ctrl Pts',(0.501092720341441,1.07986175482692,2.4));
#23032=CARTESIAN_POINT('Ctrl Pts',(0.502533036573698,1.08126699616446,2.4));
#23033=CARTESIAN_POINT('Ctrl Pts',(0.504010178078511,1.08263575731582,2.4));
#23034=CARTESIAN_POINT('Origin',(-0.6,1.,2.15));
#23035=CARTESIAN_POINT('Origin',(0.6,1.,2.15));
#23036=CARTESIAN_POINT('Origin',(0.,0.,7.8));
#23037=CARTESIAN_POINT('',(-0.6,-0.2,7.8));
#23038=CARTESIAN_POINT('Origin',(-0.6,0.,7.8));
#23039=CARTESIAN_POINT('',(-1.,-0.2,7.8));
#23040=CARTESIAN_POINT('',(0.,-0.2,7.8));
#23041=CARTESIAN_POINT('Origin',(-1.,0.,7.8));
#23042=CARTESIAN_POINT('Origin',(0.,0.,7.8));
#23043=CARTESIAN_POINT('',(1.,-0.2,7.8));
#23044=CARTESIAN_POINT('Origin',(1.,0.,7.8));
#23045=CARTESIAN_POINT('',(0.6,-0.2,7.8));
#23046=CARTESIAN_POINT('',(0.,-0.2,7.8));
#23047=CARTESIAN_POINT('Origin',(0.6,0.,7.8));
#23048=CARTESIAN_POINT('Origin',(0.6,0.6,6.8));
#23049=CARTESIAN_POINT('',(0.6,-0.6,7.));
#23050=CARTESIAN_POINT('',(0.6,0.6,7.));
#23051=CARTESIAN_POINT('',(0.6,0.3,7.));
#23052=CARTESIAN_POINT('',(0.6,-0.6,8.6));
#23053=CARTESIAN_POINT('',(0.6,-0.6,6.8));
#23054=CARTESIAN_POINT('',(0.6,0.6,8.6));
#23055=CARTESIAN_POINT('',(0.6,0.6,8.6));
#23056=CARTESIAN_POINT('',(0.6,0.6,6.8));
#23057=CARTESIAN_POINT('Origin',(0.8,0.,8.6));
#23058=CARTESIAN_POINT('',(1.,-0.6,8.6));
#23059=CARTESIAN_POINT('',(0.6,-0.6,8.6));
#23060=CARTESIAN_POINT('',(1.,0.6,8.6));
#23061=CARTESIAN_POINT('',(1.,-0.6,8.6));
#23062=CARTESIAN_POINT('',(1.,0.6,8.6));
#23063=CARTESIAN_POINT('Origin',(-1.,-0.6,6.6));
#23064=CARTESIAN_POINT('',(1.,-0.6,6.6));
#23065=CARTESIAN_POINT('',(1.,-0.6,6.6));
#23066=CARTESIAN_POINT('',(-0.6,-0.6,7.));
#23067=CARTESIAN_POINT('',(-1.,-0.6,7.));
#23068=CARTESIAN_POINT('',(-0.6,-0.6,8.6));
#23069=CARTESIAN_POINT('',(-0.6,-0.6,6.8));
#23070=CARTESIAN_POINT('',(-1.,-0.6,8.6));
#23071=CARTESIAN_POINT('',(-1.,-0.6,8.6));
#23072=CARTESIAN_POINT('',(-1.,-0.6,6.6));
#23073=CARTESIAN_POINT('',(-1.,-0.6,6.6));
#23074=CARTESIAN_POINT('',(0.,-0.6,6.6));
#23075=CARTESIAN_POINT('',(-1.,-0.6,6.6));
#23076=CARTESIAN_POINT('',(-1.,-0.6,6.6));
#23077=CARTESIAN_POINT('Origin',(0.,0.,7.));
#23078=CARTESIAN_POINT('',(-0.6,0.6,7.));
#23079=CARTESIAN_POINT('',(1.,0.6,7.));
#23080=CARTESIAN_POINT('',(-0.6,-0.3,7.));
#23081=CARTESIAN_POINT('Origin',(-0.6,-0.6,6.8));
#23082=CARTESIAN_POINT('',(-0.6,0.6,8.6));
#23083=CARTESIAN_POINT('',(-0.6,0.6,6.8));
#23084=CARTESIAN_POINT('',(-0.6,-0.6,8.6));
#23085=CARTESIAN_POINT('Origin',(-0.8,0.,8.6));
#23086=CARTESIAN_POINT('',(-1.,0.6,8.6));
#23087=CARTESIAN_POINT('',(-1.,0.6,8.6));
#23088=CARTESIAN_POINT('',(-0.6,0.6,8.6));
#23089=CARTESIAN_POINT('Origin',(0.,0.,6.6));
#23090=CARTESIAN_POINT('',(0.,0.6,6.6));
#23091=CARTESIAN_POINT('Origin',(0.,0.,6.6));
#23092=CARTESIAN_POINT('',(1.,0.6,6.6));
#23093=CARTESIAN_POINT('',(1.,0.6,6.6));
#23094=CARTESIAN_POINT('',(1.,-0.6,6.6));
#23095=CARTESIAN_POINT('Origin',(0.,0.,6.6));
#23096=CARTESIAN_POINT('',(-0.6,-7.34788079488412E-17,6.6));
#23097=CARTESIAN_POINT('Origin',(0.,0.,6.6));
#23098=CARTESIAN_POINT('',(-1.,0.6,6.6));
#23099=CARTESIAN_POINT('',(-1.,0.6,6.6));
#23100=CARTESIAN_POINT('',(1.,0.6,6.6));
#23101=CARTESIAN_POINT('Origin',(0.,0.,6.6));
#23102=CARTESIAN_POINT('Origin',(1.,0.6,6.6));
#23103=CARTESIAN_POINT('',(1.,0.6,6.6));
#23104=CARTESIAN_POINT('',(-1.,0.6,6.6));
#23105=CARTESIAN_POINT('Origin',(1.,-0.6,6.6));
#23106=CARTESIAN_POINT('Origin',(-1.,0.6,6.6));
#23107=CARTESIAN_POINT('Origin',(-1.8,0.6,2.));
#23108=CARTESIAN_POINT('',(0.8,0.6,2.4));
#23109=CARTESIAN_POINT('',(0.8,0.6,2.));
#23110=CARTESIAN_POINT('',(1.8,0.6,2.4));
#23111=CARTESIAN_POINT('',(1.8,0.6,2.));
#23112=CARTESIAN_POINT('',(-1.8,0.6,2.4));
#23113=CARTESIAN_POINT('Origin',(1.8,1.4,2.));
#23114=CARTESIAN_POINT('',(-1.8,1.4,2.4));
#23115=CARTESIAN_POINT('',(-1.8,1.4,2.));
#23116=CARTESIAN_POINT('',(1.8,1.4,2.4));
#23117=CARTESIAN_POINT('',(1.8,1.4,2.4));
#23118=CARTESIAN_POINT('',(1.8,1.4,2.));
#23119=CARTESIAN_POINT('Origin',(1.8,0.6,2.));
#23120=CARTESIAN_POINT('',(1.8,0.6,2.4));
#23121=CARTESIAN_POINT('Origin',(-1.8,0.6,2.));
#23122=CARTESIAN_POINT('',(-0.8,0.6,2.4));
#23123=CARTESIAN_POINT('',(-0.8,0.6,2.));
#23124=CARTESIAN_POINT('',(-1.8,0.6,2.4));
#23125=CARTESIAN_POINT('',(-1.8,0.6,2.4));
#23126=CARTESIAN_POINT('',(-1.8,0.6,2.));
#23127=CARTESIAN_POINT('Origin',(-1.8,1.4,2.));
#23128=CARTESIAN_POINT('',(-1.8,1.4,2.4));
#23129=CARTESIAN_POINT('Origin',(0.,0.,2.));
#23130=CARTESIAN_POINT('Origin',(0.,0.,2.4));
#23131=CARTESIAN_POINT('Origin',(0.,0.,2.4));
#23132=CARTESIAN_POINT('',(-0.6,-7.34788079488412E-17,2.4));
#23133=CARTESIAN_POINT('',(-0.6,-7.34788079488412E-17,2.4));
#23134=CARTESIAN_POINT('Origin',(0.,0.,2.4));
#23135=CARTESIAN_POINT('Origin',(0.,0.,2.4));
#23136=CARTESIAN_POINT('',(0.,0.,0.));
#23137=CARTESIAN_POINT('Origin',(-0.6,1.,2.5));
#23138=CARTESIAN_POINT('',(-0.8,1.,2.6));
#23139=CARTESIAN_POINT('Origin',(-0.6,1.,2.6));
#23140=CARTESIAN_POINT('',(-0.8,1.,2.4));
#23141=CARTESIAN_POINT('',(-0.8,1.,2.5));
#23142=CARTESIAN_POINT('Origin',(-0.6,1.,2.4));
#23143=CARTESIAN_POINT('Origin',(0.6,1.,2.5));
#23144=CARTESIAN_POINT('',(0.4,1.,2.6));
#23145=CARTESIAN_POINT('Origin',(0.6,1.,2.6));
#23146=CARTESIAN_POINT('',(0.4,1.,2.4));
#23147=CARTESIAN_POINT('',(0.4,1.,2.5));
#23148=CARTESIAN_POINT('Origin',(0.6,1.,2.4));
#23149=CARTESIAN_POINT('Origin',(1.8,1.4,2.4));
#23150=CARTESIAN_POINT('',(1.8,1.4,2.4));
#23151=CARTESIAN_POINT('',(-1.8,1.4,2.4));
#23152=CARTESIAN_POINT('',(1.8,1.4,2.4));
#23153=CARTESIAN_POINT('',(-1.8,1.4,2.6));
#23154=CARTESIAN_POINT('',(-1.8,1.4,2.4));
#23155=CARTESIAN_POINT('',(1.8,1.4,2.6));
#23156=CARTESIAN_POINT('',(1.8,1.4,2.6));
#23157=CARTESIAN_POINT('',(1.8,1.4,2.4));
#23158=CARTESIAN_POINT('Origin',(1.8,0.6,2.4));
#23159=CARTESIAN_POINT('',(1.8,0.6,2.4));
#23160=CARTESIAN_POINT('',(1.8,0.6,2.4));
#23161=CARTESIAN_POINT('',(1.8,0.6,2.6));
#23162=CARTESIAN_POINT('',(1.8,0.6,2.6));
#23163=CARTESIAN_POINT('',(1.8,0.6,2.4));
#23164=CARTESIAN_POINT('Origin',(-1.8,0.6,2.4));
#23165=CARTESIAN_POINT('',(-1.8,0.6,2.4));
#23166=CARTESIAN_POINT('',(-1.8,0.6,2.4));
#23167=CARTESIAN_POINT('',(-1.8,0.6,2.6));
#23168=CARTESIAN_POINT('',(-1.8,0.6,2.6));
#23169=CARTESIAN_POINT('',(-1.8,0.6,2.4));
#23170=CARTESIAN_POINT('Origin',(-1.8,1.4,2.4));
#23171=CARTESIAN_POINT('',(-1.8,1.4,2.4));
#23172=CARTESIAN_POINT('',(-1.8,1.4,2.6));
#23173=CARTESIAN_POINT('Origin',(0.,1.,2.6));
#23174=CARTESIAN_POINT('Origin',(0.,1.,2.4));
#23175=CARTESIAN_POINT('',(0.,0.,0.));
#23176=CARTESIAN_POINT('Origin',(0.,0.,0.05));
#23177=CARTESIAN_POINT('',(-0.7,8.57252759403147E-17,0.1));
#23178=CARTESIAN_POINT('Origin',(0.,0.,0.1));
#23179=CARTESIAN_POINT('',(-0.6,-7.34788079488412E-17,0.));
#23180=CARTESIAN_POINT('',(-0.65,-7.9602041944578E-17,0.05));
#23181=CARTESIAN_POINT('Origin',(0.,0.,0.));
#23182=CARTESIAN_POINT('Origin',(0.,0.,0.));
#23183=CARTESIAN_POINT('',(-0.7,-8.57252759403147E-17,0.9));
#23184=CARTESIAN_POINT('Origin',(0.,0.,0.9));
#23185=CARTESIAN_POINT('',(-0.7,-8.57252759403147E-17,0.));
#23186=CARTESIAN_POINT('Origin',(0.,0.,0.));
#23187=CARTESIAN_POINT('',(-0.4,4.89858719658941E-17,0.));
#23188=CARTESIAN_POINT('Origin',(0.,0.,0.));
#23189=CARTESIAN_POINT('Origin',(0.,0.,0.95));
#23190=CARTESIAN_POINT('',(-0.6,7.34788079488412E-17,1.));
#23191=CARTESIAN_POINT('Origin',(0.,0.,1.));
#23192=CARTESIAN_POINT('',(-0.65,-7.9602041944578E-17,0.95));
#23193=CARTESIAN_POINT('Origin',(0.,0.,1.));
#23194=CARTESIAN_POINT('',(-0.4,-4.89858719658941E-17,1.));
#23195=CARTESIAN_POINT('Origin',(0.,0.,1.));
#23196=CARTESIAN_POINT('Origin',(0.,0.,0.05));
#23197=CARTESIAN_POINT('',(-0.3,-3.67394039744206E-17,0.1));
#23198=CARTESIAN_POINT('Origin',(0.,0.,0.1));
#23199=CARTESIAN_POINT('',(-0.35,-4.28626379701574E-17,0.05));
#23200=CARTESIAN_POINT('Origin',(0.,0.,0.));
#23201=CARTESIAN_POINT('',(-0.3,3.67394039744206E-17,0.9));
#23202=CARTESIAN_POINT('Origin',(0.,0.,0.9));
#23203=CARTESIAN_POINT('',(-0.3,-3.67394039744206E-17,0.));
#23204=CARTESIAN_POINT('Origin',(0.,0.,0.95));
#23205=CARTESIAN_POINT('',(-0.35,-4.28626379701574E-17,0.95));
#23206=CARTESIAN_POINT('',(0.,0.,0.));
#23207=CARTESIAN_POINT('Origin',(0.,0.,1.3));
#23208=CARTESIAN_POINT('',(0.166752921449725,-0.000121400228749406,1.61285196366098));
#23209=CARTESIAN_POINT('',(0.166796959880497,9.66735530056473E-5,1.63214803633902));
#23210=CARTESIAN_POINT('',(0.1666,2.04026156737949E-17,1.3));
#23211=CARTESIAN_POINT('',(0.163512932725146,-0.0319230454628286,1.7));
#23212=CARTESIAN_POINT('Ctrl Pts',(0.166796959880497,9.66735530056473E-5,
1.63214803633902));
#23213=CARTESIAN_POINT('Ctrl Pts',(0.166837734552074,0.00590520031683778,
1.63253777944574));
#23214=CARTESIAN_POINT('Ctrl Pts',(0.166560755157907,0.0117098399368759,
1.63292752255246));
#23215=CARTESIAN_POINT('Ctrl Pts',(0.165953190799148,0.0174796970799782,
1.63331726565918));
#23216=CARTESIAN_POINT('Ctrl Pts',(0.160178154195734,0.0723234938194388,
1.63702186201144));
#23217=CARTESIAN_POINT('Ctrl Pts',(0.124534989745148,0.12402471730472,1.64072645836371));
#23218=CARTESIAN_POINT('Ctrl Pts',(0.0753220427557469,0.148912116862319,
1.64443105471598));
#23219=CARTESIAN_POINT('Ctrl Pts',(0.0261090957663466,0.173799516419917,
1.64813565106825));
#23220=CARTESIAN_POINT('Ctrl Pts',(-0.0366736337618685,0.171873092049834,
1.65184024742052));
#23221=CARTESIAN_POINT('Ctrl Pts',(-0.0842665124811252,0.144033445936741,
1.65554484377278));
#23222=CARTESIAN_POINT('Ctrl Pts',(-0.131859391200383,0.116193799823647,
1.65924944012505));
#23223=CARTESIAN_POINT('Ctrl Pts',(-0.164262419110682,0.0624409319675427,
1.66295403647732));
#23224=CARTESIAN_POINT('Ctrl Pts',(-0.16669782361829,0.00733866012848643,
1.66665863282959));
#23225=CARTESIAN_POINT('Ctrl Pts',(-0.169133228125899,-0.0477636117105698,
1.67036322918185));
#23226=CARTESIAN_POINT('Ctrl Pts',(-0.141601009230818,-0.104215287532578,
1.67406782553412));
#23227=CARTESIAN_POINT('Ctrl Pts',(-0.0965988342506402,-0.136109501609562,
1.67777242188639));
#23228=CARTESIAN_POINT('Ctrl Pts',(-0.0515966592704642,-0.168003715686544,
1.68147701823866));
#23229=CARTESIAN_POINT('Ctrl Pts',(0.0108754717948065,-0.175340468018505,
1.68518161459093));
#23230=CARTESIAN_POINT('Ctrl Pts',(0.0619990767693629,-0.154913285529167,
1.6888862109432));
#23231=CARTESIAN_POINT('Ctrl Pts',(0.11312268174392,-0.134486103039829,
1.69259080729546));
#23232=CARTESIAN_POINT('Ctrl Pts',(0.152897760627763,-0.0862949857291919,
1.69629540364773));
#23233=CARTESIAN_POINT('Ctrl Pts',(0.163512932725146,-0.0319230454628286,
1.7));
#23234=CARTESIAN_POINT('',(0.0052623718904234,0.166820541544646,1.7));
#23235=CARTESIAN_POINT('Origin',(0.,0.,1.7));
#23236=CARTESIAN_POINT('',(0.166340825374871,-6.57396331519428E-5,1.68285196366098));
#23237=CARTESIAN_POINT('Ctrl Pts',(0.00526237188778958,0.16682061735739,
1.7));
#23238=CARTESIAN_POINT('Ctrl Pts',(0.059315846276127,0.165049198896683,
1.69636770818144));
#23239=CARTESIAN_POINT('Ctrl Pts',(0.112514618214038,0.134574177622605,
1.69273541636289));
#23240=CARTESIAN_POINT('Ctrl Pts',(0.141280425894631,0.0887797885328044,
1.68910312454433));
#23241=CARTESIAN_POINT('Ctrl Pts',(0.157782375695069,0.0625091300380853,
1.68701940424988));
#23242=CARTESIAN_POINT('Ctrl Pts',(0.166243631438541,0.0311969895334432,
1.68493568395543));
#23243=CARTESIAN_POINT('Ctrl Pts',(0.166340825374871,-6.57396331519428E-5,
1.68285196366098));
#23244=CARTESIAN_POINT('',(0.1666,-2.04026156737949E-17,1.8));
#23245=CARTESIAN_POINT('',(0.1666,2.04026156737949E-17,1.3));
#23246=CARTESIAN_POINT('Origin',(0.,0.,1.8));
#23247=CARTESIAN_POINT('Ctrl Pts',(0.166340825374871,-6.57396331519428E-5,
1.68285196366098));
#23248=CARTESIAN_POINT('Ctrl Pts',(0.166416430207622,-0.024384267097259,
1.68123108760316));
#23249=CARTESIAN_POINT('Ctrl Pts',(0.161431015607884,-0.0486728962000426,
1.67961021154535));
#23250=CARTESIAN_POINT('Ctrl Pts',(0.151232376946182,-0.070535415398117,
1.67798933548753));
#23251=CARTESIAN_POINT('Ctrl Pts',(0.12792285898394,-0.120503337672002,
1.67428473913526));
#23252=CARTESIAN_POINT('Ctrl Pts',(0.0773807749454364,-0.157797874435697,
1.67058014278299));
#23253=CARTESIAN_POINT('Ctrl Pts',(0.0227482513872868,-0.165320125260105,
1.66687554643073));
#23254=CARTESIAN_POINT('Ctrl Pts',(-0.0318842721708627,-0.172842376084512,
1.66317095007846));
#23255=CARTESIAN_POINT('Ctrl Pts',(-0.0906072352486578,-0.150592340969633,
1.65946635372619));
#23256=CARTESIAN_POINT('Ctrl Pts',(-0.126551605667113,-0.108768963100728,
1.65576175737392));
#23257=CARTESIAN_POINT('Ctrl Pts',(-0.162495976085569,-0.0669455852318239,
1.65205716102165));
#23258=CARTESIAN_POINT('Ctrl Pts',(-0.175661753844685,-0.00554886460889432,
1.64835256466938));
#23259=CARTESIAN_POINT('Ctrl Pts',(-0.160020484350268,0.0473310422055452,
1.64464796831712));
#23260=CARTESIAN_POINT('Ctrl Pts',(-0.144379214855851,0.100210949019985,
1.64094337196485));
#23261=CARTESIAN_POINT('Ctrl Pts',(-0.0999308981078997,0.144574042025934,
1.63723877561258));
#23262=CARTESIAN_POINT('Ctrl Pts',(-0.0470191573240233,0.160112912591645,
1.63353417926031));
#23263=CARTESIAN_POINT('Ctrl Pts',(0.00589258345985309,0.175651783157355,
1.62982958290805));
#23264=CARTESIAN_POINT('Ctrl Pts',(0.067267748279655,0.162366431282826,
1.62612498655578));
#23265=CARTESIAN_POINT('Ctrl Pts',(0.109018480103692,0.126339265236092,
1.62242039020351));
#23266=CARTESIAN_POINT('Ctrl Pts',(0.144963809686008,0.0953216446845623,
1.61923091468933));
#23267=CARTESIAN_POINT('Ctrl Pts',(0.166362794628908,0.0474469630018487,
1.61604143917516));
#23268=CARTESIAN_POINT('Ctrl Pts',(0.166752921449725,-0.000121400228749406,
1.61285196366098));
#23269=CARTESIAN_POINT('Origin',(0.,0.,1.3));
#23270=CARTESIAN_POINT('',(0.166721717270512,0.00013247748987999,1.54285196366098));
#23271=CARTESIAN_POINT('',(0.166368100504911,8.32215516180224E-5,1.56214803633902));
#23272=CARTESIAN_POINT('',(0.1666,2.04026156737949E-17,1.3));
#23273=CARTESIAN_POINT('Ctrl Pts',(0.166368100504911,8.32215516180223E-5,
1.56214803633902));
#23274=CARTESIAN_POINT('Ctrl Pts',(0.166469575983711,0.0225191704554514,
1.56364353466546));
#23275=CARTESIAN_POINT('Ctrl Pts',(0.162248711501603,0.0449185271683059,
1.56513903299191));
#23276=CARTESIAN_POINT('Ctrl Pts',(0.153524147106197,0.0653993692500711,
1.56663453131835));
#23277=CARTESIAN_POINT('Ctrl Pts',(0.131911960142923,0.116133797718439,
1.57033912767062));
#23278=CARTESIAN_POINT('Ctrl Pts',(0.0826635066749161,0.155095554237362,
1.57404372402289));
#23279=CARTESIAN_POINT('Ctrl Pts',(0.028317337914343,0.164453369456362,
1.57774832037515));
#23280=CARTESIAN_POINT('Ctrl Pts',(-0.026028830846231,0.173811184675361,
1.58145291672742));
#23281=CARTESIAN_POINT('Ctrl Pts',(-0.0854727148993724,0.153565058594437,
1.58515751307969));
#23282=CARTESIAN_POINT('Ctrl Pts',(-0.122808942133701,0.11298112966685,
1.58886210943196));
#23283=CARTESIAN_POINT('Ctrl Pts',(-0.160145169368031,0.0723972007392629,
1.59256670578423));
#23284=CARTESIAN_POINT('Ctrl Pts',(-0.175373739783547,0.0114754689650147,
1.59627130213649));
#23285=CARTESIAN_POINT('Ctrl Pts',(-0.161526248741115,-0.041903625100424,
1.59997589848876));
#23286=CARTESIAN_POINT('Ctrl Pts',(-0.147678757698683,-0.0952827191658612,
1.60368049484103));
#23287=CARTESIAN_POINT('Ctrl Pts',(-0.1047552051983,-0.14111917552249,1.6073850911933));
#23288=CARTESIAN_POINT('Ctrl Pts',(-0.0523978126792817,-0.158434271662077,
1.61108968754557));
#23289=CARTESIAN_POINT('Ctrl Pts',(-4.04201602626775E-5,-0.175749367801665,
1.61479428389783));
#23290=CARTESIAN_POINT('Ctrl Pts',(0.0617508123773913,-0.164543103724215,
1.6184988802501));
#23291=CARTESIAN_POINT('Ctrl Pts',(0.104692974268098,-0.12994678668867,
1.62220347660237));
#23292=CARTESIAN_POINT('Ctrl Pts',(0.143117393875163,-0.0989901849689851,
1.62551832984792));
#23293=CARTESIAN_POINT('Ctrl Pts',(0.166450162079376,-0.0493061599110598,
1.62883318309347));
#23294=CARTESIAN_POINT('Ctrl Pts',(0.166796959880497,9.66735530056473E-5,
1.63214803633902));
#23295=CARTESIAN_POINT('Ctrl Pts',(0.166752921449725,-0.000121400228749406,
1.61285196366098));
#23296=CARTESIAN_POINT('Ctrl Pts',(0.166815929443988,-0.00780399726549495,
1.61233684282289));
#23297=CARTESIAN_POINT('Ctrl Pts',(0.166330935441723,-0.0154786041905287,
1.6118217219848));
#23298=CARTESIAN_POINT('Ctrl Pts',(0.165270714247807,-0.0230729153352646,
1.61130660114671));
#23299=CARTESIAN_POINT('Ctrl Pts',(0.157645917739612,-0.0776889496409508,
1.60760200479444));
#23300=CARTESIAN_POINT('Ctrl Pts',(0.120270025894947,-0.128152038033383,
1.60389740844217));
#23301=CARTESIAN_POINT('Ctrl Pts',(0.0702485553938763,-0.151366836780329,
1.6001928120899));
#23302=CARTESIAN_POINT('Ctrl Pts',(0.0202270848928061,-0.174581635527273,
1.59648821573763));
#23303=CARTESIAN_POINT('Ctrl Pts',(-0.0424399642646696,-0.170548144628732,
1.59278361938537));
#23304=CARTESIAN_POINT('Ctrl Pts',(-0.0890727806898626,-0.141112640607554,
1.5890790230331));
#23305=CARTESIAN_POINT('Ctrl Pts',(-0.135705597115056,-0.111677136586376,
1.58537442668083));
#23306=CARTESIAN_POINT('Ctrl Pts',(-0.166304180807966,-0.0568396194425618,
1.58166983032856));
#23307=CARTESIAN_POINT('Ctrl Pts',(-0.16686485427816,-0.00169661928996206,
1.57796523397629));
#23308=CARTESIAN_POINT('Ctrl Pts',(-0.167425527748354,0.0534463808626376,
1.57426063762402));
#23309=CARTESIAN_POINT('Ctrl Pts',(-0.137948290995833,0.108894864024023,
1.57055604127176));
#23310=CARTESIAN_POINT('Ctrl Pts',(-0.0919236010333964,0.139272428377062,
1.56685144491949));
#23311=CARTESIAN_POINT('Ctrl Pts',(-0.0458989110709602,0.169649992730101,
1.56314684856722));
#23312=CARTESIAN_POINT('Ctrl Pts',(0.0166732321013904,0.174956638274794,
1.55944225221495));
#23313=CARTESIAN_POINT('Ctrl Pts',(0.0671563493099001,0.152763795116617,
1.55573765586268));
#23314=CARTESIAN_POINT('Ctrl Pts',(0.117639466518409,0.13057095195844,1.55203305951042));
#23315=CARTESIAN_POINT('Ctrl Pts',(0.156033557763077,0.0808786200973942,
1.54832846315815));
#23316=CARTESIAN_POINT('Ctrl Pts',(0.164767340619488,0.0264287526812992,
1.54462386680588));
#23317=CARTESIAN_POINT('Ctrl Pts',(0.166159792575437,0.0177476547388351,
1.54403323242425));
#23318=CARTESIAN_POINT('Ctrl Pts',(0.166798314017023,0.0089456257803759,
1.54344259804261));
#23319=CARTESIAN_POINT('Ctrl Pts',(0.166721717270512,0.00013247748987999,
1.54285196366098));
#23320=CARTESIAN_POINT('Origin',(0.,0.,1.3));
#23321=CARTESIAN_POINT('',(0.166334949033457,3.80241454671915E-5,1.47285196366098));
#23322=CARTESIAN_POINT('',(0.166495616539739,-0.000143126867227327,1.49214803633902));
#23323=CARTESIAN_POINT('',(0.1666,2.04026156737949E-17,1.3));
#23324=CARTESIAN_POINT('Ctrl Pts',(0.166495616539739,-0.000143126867227327,
1.49214803633902));
#23325=CARTESIAN_POINT('Ctrl Pts',(0.166176505544999,0.0388065957770001,
1.49474928988519));
#23326=CARTESIAN_POINT('Ctrl Pts',(0.15254095518154,0.0779576027494656,
1.49735054343136));
#23327=CARTESIAN_POINT('Ctrl Pts',(0.127581990737563,0.107562045989894,
1.49995179697752));
#23328=CARTESIAN_POINT('Ctrl Pts',(0.0920364789316288,0.149723454131357,
1.50365639332979));
#23329=CARTESIAN_POINT('Ctrl Pts',(0.0335245204022979,0.172522270232617,
1.50736098968206));
#23330=CARTESIAN_POINT('Ctrl Pts',(-0.0211755609783529,0.165524482759979,
1.51106558603433));
#23331=CARTESIAN_POINT('Ctrl Pts',(-0.0758756423590036,0.158526695287341,
1.5147701823866));
#23332=CARTESIAN_POINT('Ctrl Pts',(-0.126763846590974,0.121732304240806,
1.51847477873887));
#23333=CARTESIAN_POINT('Ctrl Pts',(-0.150550887470885,0.0719804791091254,
1.52217937509113));
#23334=CARTESIAN_POINT('Ctrl Pts',(-0.174337928350795,0.0222286539774451,
1.5258839714434));
#23335=CARTESIAN_POINT('Ctrl Pts',(-0.171023805878645,-0.0404806052393804,
1.52958856779567));
#23336=CARTESIAN_POINT('Ctrl Pts',(-0.142125268024159,-0.0874480653886775,
1.53329316414794));
#23337=CARTESIAN_POINT('Ctrl Pts',(-0.113226730169674,-0.134415525537975,
1.5369977605002));
#23338=CARTESIAN_POINT('Ctrl Pts',(-0.058743776932853,-0.165641186619743,
1.54070235685247));
#23339=CARTESIAN_POINT('Ctrl Pts',(-0.00361080053401195,-0.166834419219364,
1.54440695320474));
#23340=CARTESIAN_POINT('Ctrl Pts',(0.0515221758648292,-0.168027651818985,
1.54811154955701));
#23341=CARTESIAN_POINT('Ctrl Pts',(0.10730517542569,-0.139188455936458,
1.55181614590928));
#23342=CARTESIAN_POINT('Ctrl Pts',(0.138208714976851,-0.0935153077862871,
1.55552074226154));
#23343=CARTESIAN_POINT('Ctrl Pts',(0.15663688952593,-0.0662798273674848,
1.55772984028737));
#23344=CARTESIAN_POINT('Ctrl Pts',(0.166218204462953,-0.0330583805181475,
1.5599389383132));
#23345=CARTESIAN_POINT('Ctrl Pts',(0.166368100504911,8.32215516180223E-5,
1.56214803633902));
#23346=CARTESIAN_POINT('Ctrl Pts',(0.166721717270512,0.00013247748987999,
1.54285196366098));
#23347=CARTESIAN_POINT('Ctrl Pts',(0.16631788138976,-0.0463324921623522,
1.53973800169035));
#23348=CARTESIAN_POINT('Ctrl Pts',(0.146036306492028,-0.0931065396480778,
1.53662403971971));
#23349=CARTESIAN_POINT('Ctrl Pts',(0.111564911721182,-0.124096839839778,
1.53351007774908));
#23350=CARTESIAN_POINT('Ctrl Pts',(0.0705552254983152,-0.160965161973612,
1.52980548139681));
#23351=CARTESIAN_POINT('Ctrl Pts',(0.00946237858443097,-0.175494403270137,
1.52610088504454));
#23352=CARTESIAN_POINT('Ctrl Pts',(-0.043754143626611,-0.161035180693733,
1.52239628869227));
#23353=CARTESIAN_POINT('Ctrl Pts',(-0.0969706658376549,-0.146575958117328,
1.51869169234));
#23354=CARTESIAN_POINT('Ctrl Pts',(-0.142310863345855,-0.103128271667992,
1.51498709598774));
#23355=CARTESIAN_POINT('Ctrl Pts',(-0.159024536403123,-0.0505761979513979,
1.51128249963547));
#23356=CARTESIAN_POINT('Ctrl Pts',(-0.175738209460389,0.00197587576519482,
1.5075779032832));
#23357=CARTESIAN_POINT('Ctrl Pts',(-0.163825358066725,0.0636323367490458,
1.50387330693093));
#23358=CARTESIAN_POINT('Ctrl Pts',(-0.128737966872089,0.106175754206211,
1.50016871057866));
#23359=CARTESIAN_POINT('Ctrl Pts',(-0.0936505756774527,0.148719171663375,
1.4964641142264));
#23360=CARTESIAN_POINT('Ctrl Pts',(-0.035388644681846,0.172149545593854,
1.49275951787413));
#23361=CARTESIAN_POINT('Ctrl Pts',(0.0193839233712769,0.165743833453852,
1.48905492152186));
#23362=CARTESIAN_POINT('Ctrl Pts',(0.0741564914244009,0.159338121313851,
1.48535032516959));
#23363=CARTESIAN_POINT('Ctrl Pts',(0.125439696535041,0.123096323103367,
1.48164572881732));
#23364=CARTESIAN_POINT('Ctrl Pts',(0.149763488908927,0.07360470278495,1.47794113246505));
#23365=CARTESIAN_POINT('Ctrl Pts',(0.160901714109468,0.0509417559807338,
1.4762447428637));
#23366=CARTESIAN_POINT('Ctrl Pts',(0.166386928169176,0.0255005071147636,
1.47454835326234));
#23367=CARTESIAN_POINT('Ctrl Pts',(0.166334949033457,3.80241454671915E-5,
1.47285196366098));
#23368=CARTESIAN_POINT('Origin',(0.,0.,1.3));
#23369=CARTESIAN_POINT('',(0.166582270817784,-0.000152340582006284,1.40285196366098));
#23370=CARTESIAN_POINT('',(0.166873478424592,6.71112968702338E-7,1.42214803633902));
#23371=CARTESIAN_POINT('',(0.1666,2.04026156737949E-17,1.3));
#23372=CARTESIAN_POINT('Ctrl Pts',(0.166873476951752,6.71109354370205E-7,
1.42214803633902));
#23373=CARTESIAN_POINT('Ctrl Pts',(0.166876772816304,0.0551824619258391,
1.42585504510491));
#23374=CARTESIAN_POINT('Ctrl Pts',(0.136792549878611,0.110361163623334,
1.42956205387081));
#23375=CARTESIAN_POINT('Ctrl Pts',(0.0904117910907898,0.140258570073462,
1.4332690626367));
#23376=CARTESIAN_POINT('Ctrl Pts',(0.0440612155535343,0.170136520159922,
1.43697365898897));
#23377=CARTESIAN_POINT('Ctrl Pts',(-0.0185646804667758,0.174766068965047,
1.44067825534124));
#23378=CARTESIAN_POINT('Ctrl Pts',(-0.0688048006597445,0.152028477144375,
1.4443828516935));
#23379=CARTESIAN_POINT('Ctrl Pts',(-0.119044920852713,0.129290885323702,
1.44808744804577));
#23380=CARTESIAN_POINT('Ctrl Pts',(-0.15689926521834,0.0791861528772324,
1.45179204439804));
#23381=CARTESIAN_POINT('Ctrl Pts',(-0.165043578186289,0.0246449948801753,
1.45549664075031));
#23382=CARTESIAN_POINT('Ctrl Pts',(-0.173187891154238,-0.0298961631168814,
1.45920123710258));
#23383=CARTESIAN_POINT('Ctrl Pts',(-0.15162217272451,-0.088873746664526,
1.46290583345484));
#23384=CARTESIAN_POINT('Ctrl Pts',(-0.110216096648825,-0.125296330528958,
1.46661042980711));
#23385=CARTESIAN_POINT('Ctrl Pts',(-0.0688100205731403,-0.16171891439339,
1.47031502615938));
#23386=CARTESIAN_POINT('Ctrl Pts',(-0.00756358685149875,-0.17558649857461,
1.47401962251165));
#23387=CARTESIAN_POINT('Ctrl Pts',(0.0454934276490607,-0.160552503958399,
1.47772421886392));
#23388=CARTESIAN_POINT('Ctrl Pts',(0.0985504421496201,-0.145518509342189,
1.48142881521618));
#23389=CARTESIAN_POINT('Ctrl Pts',(0.143418037429097,-0.101582935928549,
1.48513341156845));
#23390=CARTESIAN_POINT('Ctrl Pts',(0.159562302527567,-0.0488531491308943,
1.48883800792072));
#23391=CARTESIAN_POINT('Ctrl Pts',(0.164370561528649,-0.0331485958143723,
1.48994135072682));
#23392=CARTESIAN_POINT('Ctrl Pts',(0.166630970058396,-0.0166639678834416,
1.49104469353292));
#23393=CARTESIAN_POINT('Ctrl Pts',(0.166495616539739,-0.000143126867227327,
1.49214803633902));
#23394=CARTESIAN_POINT('Ctrl Pts',(0.166334949033457,3.80241454671915E-5,
1.47285196366098));
#23395=CARTESIAN_POINT('Ctrl Pts',(0.166273415497072,-0.0301047745093415,
1.47084375691007));
#23396=CARTESIAN_POINT('Ctrl Pts',(0.158451996361882,-0.0602773308783548,
1.46883555015916));
#23397=CARTESIAN_POINT('Ctrl Pts',(0.143062834518306,-0.085905647341766,
1.46682734340825));
#23398=CARTESIAN_POINT('Ctrl Pts',(0.114674008116665,-0.133182934723717,
1.46312274705598));
#23399=CARTESIAN_POINT('Ctrl Pts',(0.060531975676251,-0.16499606706127,
1.45941815070371));
#23400=CARTESIAN_POINT('Ctrl Pts',(0.00541514530056254,-0.166785584082033,
1.45571355435145));
#23401=CARTESIAN_POINT('Ctrl Pts',(-0.0497016850751255,-0.168575101102797,
1.45200895799918));
#23402=CARTESIAN_POINT('Ctrl Pts',(-0.105793313386088,-0.14034100280677,
1.44830436164691));
#23403=CARTESIAN_POINT('Ctrl Pts',(-0.137189087849022,-0.0950047843070436,
1.44459976529464));
#23404=CARTESIAN_POINT('Ctrl Pts',(-0.168584862311956,-0.0496685658073169,
1.44089516894238));
#23405=CARTESIAN_POINT('Ctrl Pts',(-0.175284782926862,0.0127697728961095,
1.43719057259011));
#23406=CARTESIAN_POINT('Ctrl Pts',(-0.154222593046579,0.0637349720094271,
1.43348597623784));
#23407=CARTESIAN_POINT('Ctrl Pts',(-0.133160403166296,0.114700171122744,
1.42978137988557));
#23408=CARTESIAN_POINT('Ctrl Pts',(-0.0843361027908238,0.154192230645953,
1.4260767835333));
#23409=CARTESIAN_POINT('Ctrl Pts',(-0.0300944098326194,0.16413738562223,
1.42237218718103));
#23410=CARTESIAN_POINT('Ctrl Pts',(0.0241472831255854,0.174082540598506,
1.41866759082877));
#23411=CARTESIAN_POINT('Ctrl Pts',(0.0838063686665219,0.154480791027852,
1.4149629944765));
#23412=CARTESIAN_POINT('Ctrl Pts',(0.121579527998707,0.114302988740736,
1.41125839812423));
#23413=CARTESIAN_POINT('Ctrl Pts',(0.150151024791829,0.0839126277146479,
1.40845625330315));
#23414=CARTESIAN_POINT('Ctrl Pts',(0.166200792747313,0.0417499637845381,
1.40565410848206));
#23415=CARTESIAN_POINT('Ctrl Pts',(0.166582270817784,-0.000152340582006284,
1.40285196366098));
#23416=CARTESIAN_POINT('Origin',(0.,0.,1.3));
#23417=CARTESIAN_POINT('',(0.16685129292948,5.5034311338048E-5,1.33285196366098));
#23418=CARTESIAN_POINT('',(0.166493658714001,0.000142704933107348,1.35214803633902));
#23419=CARTESIAN_POINT('',(0.1666,2.04026156737949E-17,1.3));
#23420=CARTESIAN_POINT('Ctrl Pts',(0.166493658714001,0.000142704933107348,
1.35214803633902));
#23421=CARTESIAN_POINT('Ctrl Pts',(0.166629086818581,0.0167362841743647,
1.35325620397237));
#23422=CARTESIAN_POINT('Ctrl Pts',(0.164348470273229,0.0332934752509887,
1.35436437160572));
#23423=CARTESIAN_POINT('Ctrl Pts',(0.159498696116421,0.0490604157264683,
1.35547253923907));
#23424=CARTESIAN_POINT('Ctrl Pts',(0.143285936322738,0.101769183257714,
1.35917713559134));
#23425=CARTESIAN_POINT('Ctrl Pts',(0.0983612975566499,0.145646425810988,
1.36288173194361));
#23426=CARTESIAN_POINT('Ctrl Pts',(0.0452847954907157,0.16061147453177,
1.36658632829587));
#23427=CARTESIAN_POINT('Ctrl Pts',(-0.00779170657521921,0.175576523252552,
1.37029092464814));
#23428=CARTESIAN_POINT('Ctrl Pts',(-0.0690200719410003,0.161629378140841,
1.37399552100041));
#23429=CARTESIAN_POINT('Ctrl Pts',(-0.11037879201089,0.125153029241032,
1.37770011735268));
#23430=CARTESIAN_POINT('Ctrl Pts',(-0.151737512080778,0.0886766803412233,
1.38140471370495));
#23431=CARTESIAN_POINT('Ctrl Pts',(-0.173226586854776,0.0296711276533176,
1.38510931005721));
#23432=CARTESIAN_POINT('Ctrl Pts',(-0.165011419406707,-0.0248594030476235,
1.38881390640948));
#23433=CARTESIAN_POINT('Ctrl Pts',(-0.156796251958638,-0.0793899337485655,
1.39251850276175));
#23434=CARTESIAN_POINT('Ctrl Pts',(-0.1188768422885,-0.129445442462543,
1.39622309911402));
#23435=CARTESIAN_POINT('Ctrl Pts',(-0.0686072232581569,-0.152117741798697,
1.39992769546629));
#23436=CARTESIAN_POINT('Ctrl Pts',(-0.0183376042278136,-0.174790041134852,
1.40363229181856));
#23437=CARTESIAN_POINT('Ctrl Pts',(0.0442822241627354,-0.170079131093183,
1.40733688817082));
#23438=CARTESIAN_POINT('Ctrl Pts',(0.0905939423885369,-0.140140986355195,
1.41104148452309));
#23439=CARTESIAN_POINT('Ctrl Pts',(0.136875502667449,-0.110222337179314,
1.41474366846173));
#23440=CARTESIAN_POINT('Ctrl Pts',(0.166870185376906,-0.0551092982940088,
1.41844585240038));
#23441=CARTESIAN_POINT('Ctrl Pts',(0.166873476951752,6.71109354370205E-7,
1.42214803633902));
#23442=CARTESIAN_POINT('Ctrl Pts',(0.166582270817784,-0.000152340582006284,
1.40285196366098));
#23443=CARTESIAN_POINT('Ctrl Pts',(0.166705128660898,-0.0136472886129686,
1.4019495121298));
#23444=CARTESIAN_POINT('Ctrl Pts',(0.165202856095667,-0.0271152318944043,
1.40104706059861));
#23445=CARTESIAN_POINT('Ctrl Pts',(0.161970345045233,-0.0401542300245841,
1.40014460906743));
#23446=CARTESIAN_POINT('Ctrl Pts',(0.148700769636142,-0.0936797914992128,
1.39644001271516));
#23447=CARTESIAN_POINT('Ctrl Pts',(0.106274385694529,-0.139977059444894,
1.39273541636289));
#23448=CARTESIAN_POINT('Ctrl Pts',(0.054107868404235,-0.157857826665655,
1.38903082001062));
#23449=CARTESIAN_POINT('Ctrl Pts',(0.00194135111394122,-0.175738593886417,
1.38532622365835));
#23450=CARTESIAN_POINT('Ctrl Pts',(-0.0599652995250327,-0.165202860382259,
1.38162162730609));
#23451=CARTESIAN_POINT('Ctrl Pts',(-0.103280153812656,-0.131072364331603,
1.37791703095382));
#23452=CARTESIAN_POINT('Ctrl Pts',(-0.146595008100279,-0.0969418682809483,
1.37421243460155));
#23453=CARTESIAN_POINT('Ctrl Pts',(-0.171318066036552,-0.0392166096837955,
1.37050783824928));
#23454=CARTESIAN_POINT('Ctrl Pts',(-0.166134679967937,0.0156851195376423,
1.36680324189701));
#23455=CARTESIAN_POINT('Ctrl Pts',(-0.160951293899322,0.0705868487590808,
1.36309864554474));
#23456=CARTESIAN_POINT('Ctrl Pts',(-0.12586146382582,0.122665048604804,
1.35939404919248));
#23457=CARTESIAN_POINT('Ctrl Pts',(-0.0769242494532953,0.14808583561233,
1.35568945284021));
#23458=CARTESIAN_POINT('Ctrl Pts',(-0.0279870350807717,0.173506622619856,
1.35198485648794));
#23459=CARTESIAN_POINT('Ctrl Pts',(0.0347975635907744,0.172269996789183,
1.34828026013567));
#23460=CARTESIAN_POINT('Ctrl Pts',(0.0826958189663461,0.144941906943662,
1.3445756637834));
#23461=CARTESIAN_POINT('Ctrl Pts',(0.130594074341918,0.117613817098141,
1.34087106743114));
#23462=CARTESIAN_POINT('Ctrl Pts',(0.163605986421516,0.0641942632377707,
1.33716647107887));
#23463=CARTESIAN_POINT('Ctrl Pts',(0.166623466451679,0.00913100709632859,
1.3334618747266));
#23464=CARTESIAN_POINT('Ctrl Pts',(0.166789062042101,0.00610920336601207,
1.33325857103806));
#23465=CARTESIAN_POINT('Ctrl Pts',(0.16686432402183,0.00308244933152886,
1.33305526734952));
#23466=CARTESIAN_POINT('Ctrl Pts',(0.16685129292948,5.5034311338048E-5,
1.33285196366098));
#23467=CARTESIAN_POINT('Origin',(0.,0.,1.3));
#23468=CARTESIAN_POINT('',(0.166419792426106,0.000117644517947116,1.26285196366098));
#23469=CARTESIAN_POINT('',(0.166369239667266,-8.42498788368234E-5,1.28214803633902));
#23470=CARTESIAN_POINT('',(0.1666,2.04026156737949E-17,1.3));
#23471=CARTESIAN_POINT('Ctrl Pts',(0.166369239667266,-8.42498788368234E-5,
1.28214803633902));
#23472=CARTESIAN_POINT('Ctrl Pts',(0.166217137033255,0.0331292003521081,
1.2843619591921));
#23473=CARTESIAN_POINT('Ctrl Pts',(0.156590960021794,0.0664238537129591,
1.28657588204517));
#23474=CARTESIAN_POINT('Ctrl Pts',(0.138087078302622,0.093694809140457,
1.28878980489824));
#23475=CARTESIAN_POINT('Ctrl Pts',(0.107124205036991,0.139327782240334,
1.29249440125051));
#23476=CARTESIAN_POINT('Ctrl Pts',(0.051303827751912,0.168094448054701,
1.29619899760278));
#23477=CARTESIAN_POINT('Ctrl Pts',(-0.00382754136500674,0.166829578855541,
1.29990359395505));
#23478=CARTESIAN_POINT('Ctrl Pts',(-0.0589589104819255,0.16556470965638,
1.30360819030732));
#23479=CARTESIAN_POINT('Ctrl Pts',(-0.113401271430684,0.134268305443692,
1.30731278665959));
#23480=CARTESIAN_POINT('Ctrl Pts',(-0.142238769013948,0.0872633430680612,
1.31101738301185));
#23481=CARTESIAN_POINT('Ctrl Pts',(-0.171076266597211,0.0402583806924305,
1.31472197936412));
#23482=CARTESIAN_POINT('Ctrl Pts',(-0.17430890081498,-0.0224551398461431,
1.31842657571639));
#23483=CARTESIAN_POINT('Ctrl Pts',(-0.150457238287118,-0.0721760202632685,
1.32213117206866));
#23484=CARTESIAN_POINT('Ctrl Pts',(-0.126605575759256,-0.121896900680394,
1.32583576842093));
#23485=CARTESIAN_POINT('Ctrl Pts',(-0.0756696164857624,-0.158625140976071,
1.32954036477319));
#23486=CARTESIAN_POINT('Ctrl Pts',(-0.0209604910548609,-0.165551853715821,
1.33324496112546));
#23487=CARTESIAN_POINT('Ctrl Pts',(0.0337486343760406,-0.17247856645557,
1.33694955747773));
#23488=CARTESIAN_POINT('Ctrl Pts',(0.0922309259643503,-0.149603751639392,
1.34065415383));
#23489=CARTESIAN_POINT('Ctrl Pts',(0.127721631347866,-0.107396197976694,
1.34435875018227));
#23490=CARTESIAN_POINT('Ctrl Pts',(0.152595889688052,-0.0778143234445287,
1.34695517890118));
#23491=CARTESIAN_POINT('Ctrl Pts',(0.166176351648266,-0.038735930748939,
1.3495516076201));
#23492=CARTESIAN_POINT('Ctrl Pts',(0.166493658714001,0.000142704933107348,
1.35214803633902));
#23493=CARTESIAN_POINT('Ctrl Pts',(0.16685129292948,5.5034311338048E-5,
1.33285196366098));
#23494=CARTESIAN_POINT('Ctrl Pts',(0.16662687167882,-0.0520830556384961,
1.32935067099725));
#23495=CARTESIAN_POINT('Ctrl Pts',(0.140215016815216,-0.104417191766459,
1.32584937833352));
#23496=CARTESIAN_POINT('Ctrl Pts',(0.0980387654551791,-0.135037607098881,
1.3223480856698));
#23497=CARTESIAN_POINT('Ctrl Pts',(0.0534135364477915,-0.167436006730135,
1.31864348931753));
#23498=CARTESIAN_POINT('Ctrl Pts',(-0.00885996954770948,-0.175525847570128,
1.31493889296526));
#23499=CARTESIAN_POINT('Ctrl Pts',(-0.0602819293976768,-0.155604768085892,
1.31123429661299));
#23500=CARTESIAN_POINT('Ctrl Pts',(-0.111703889247644,-0.135683688601655,
1.30752970026073));
#23501=CARTESIAN_POINT('Ctrl Pts',(-0.152274302952078,-0.0877516887931891,
1.30382510390846));
#23502=CARTESIAN_POINT('Ctrl Pts',(-0.163425890629257,-0.0337451201657775,
1.30012050755619));
#23503=CARTESIAN_POINT('Ctrl Pts',(-0.174577478306436,0.0202614484616345,
1.29641591120392));
#23504=CARTESIAN_POINT('Ctrl Pts',(-0.15631023995636,0.0803425859079921,
1.29271131485165));
#23505=CARTESIAN_POINT('Ctrl Pts',(-0.116984280792225,0.119001818937757,
1.28900671849938));
#23506=CARTESIAN_POINT('Ctrl Pts',(-0.077658321628091,0.157661051967521,
1.28530212214712));
#23507=CARTESIAN_POINT('Ctrl Pts',(-0.0172736416498982,0.174898380580693,
1.28159752579485));
#23508=CARTESIAN_POINT('Ctrl Pts',(0.0365343679459083,0.162825043595149,
1.27789292944258));
#23509=CARTESIAN_POINT('Ctrl Pts',(0.090342377541716,0.150751706609605,
1.27418833309031));
#23510=CARTESIAN_POINT('Ctrl Pts',(0.137573716755137,0.109367704025345,
1.27048373673804));
#23511=CARTESIAN_POINT('Ctrl Pts',(0.15661269537524,0.0576126592883118,
1.26677914038578));
#23512=CARTESIAN_POINT('Ctrl Pts',(0.163340322948393,0.0393244583837232,
1.26547008147751));
#23513=CARTESIAN_POINT('Ctrl Pts',(0.166547744893355,0.0197412896159237,
1.26416102256925));
#23514=CARTESIAN_POINT('Ctrl Pts',(0.166419792426106,0.000117644517947116,
1.26285196366098));
#23515=CARTESIAN_POINT('Origin',(0.,0.,1.3));
#23516=CARTESIAN_POINT('',(0.166426142970557,-0.000120642765556289,1.19285196366098));
#23517=CARTESIAN_POINT('',(0.16680112293357,-9.74720745467285E-5,1.21214803633902));
#23518=CARTESIAN_POINT('',(0.1666,2.04026156737949E-17,1.3));
#23519=CARTESIAN_POINT('Ctrl Pts',(0.16680112293357,-9.74720745467285E-5,
1.21214803633902));
#23520=CARTESIAN_POINT('Ctrl Pts',(0.166457232615762,0.0493755335317627,
1.21546771441182));
#23521=CARTESIAN_POINT('Ctrl Pts',(0.143044424972525,0.0991312161213854,
1.21878739248462));
#23522=CARTESIAN_POINT('Ctrl Pts',(0.104522946124804,0.130083481608585,
1.22210707055742));
#23523=CARTESIAN_POINT('Ctrl Pts',(0.0615348831579396,0.164624677261814,
1.22581166690969));
#23524=CARTESIAN_POINT('Ctrl Pts',(-0.000268695245690821,0.175749122363903,
1.22951626326196));
#23525=CARTESIAN_POINT('Ctrl Pts',(-0.0526030309795398,0.15836565153399,
1.23322085961422));
#23526=CARTESIAN_POINT('Ctrl Pts',(-0.104937366713389,0.140982180704076,
1.23692545596649));
#23527=CARTESIAN_POINT('Ctrl Pts',(-0.147802459777456,0.0950907939421611,
1.24063005231876));
#23528=CARTESIAN_POINT('Ctrl Pts',(-0.161580857269364,0.0416939446216941,
1.24433464867103));
#23529=CARTESIAN_POINT('Ctrl Pts',(-0.175359254761272,-0.0117029046987729,
1.2480392450233));
#23530=CARTESIAN_POINT('Ctrl Pts',(-0.16005095668102,-0.0726052165777916,
1.25174384137556));
#23531=CARTESIAN_POINT('Ctrl Pts',(-0.122661892448987,-0.113140702644331,
1.25544843772783));
#23532=CARTESIAN_POINT('Ctrl Pts',(-0.0852728282169544,-0.15367618871087,
1.2591530340801));
#23533=CARTESIAN_POINT('Ctrl Pts',(-0.0258029978331414,-0.17384484896493,
1.26285763043237));
#23534=CARTESIAN_POINT('Ctrl Pts',(0.0285308936104228,-0.164416381677161,
1.26656222678464));
#23535=CARTESIAN_POINT('Ctrl Pts',(0.0828647850539866,-0.154987914389393,
1.2702668231369));
#23536=CARTESIAN_POINT('Ctrl Pts',(0.132062737557302,-0.115962319559795,
1.27397141948917));
#23537=CARTESIAN_POINT('Ctrl Pts',(0.153609029185868,-0.0651998819523026,
1.27767601584144));
#23538=CARTESIAN_POINT('Ctrl Pts',(0.162278930811433,-0.044773845401895,
1.27916668934063));
#23539=CARTESIAN_POINT('Ctrl Pts',(0.166471653066795,-0.022447454634266,
1.28065736283983));
#23540=CARTESIAN_POINT('Ctrl Pts',(0.166369239667266,-8.42498788368234E-5,
1.28214803633902));
#23541=CARTESIAN_POINT('Ctrl Pts',(0.166419792426106,0.000117644517947116,
1.26285196366098));
#23542=CARTESIAN_POINT('Ctrl Pts',(0.166185643355799,-0.0357930210168177,
1.26045642621698));
#23543=CARTESIAN_POINT('Ctrl Pts',(0.154782035268061,-0.0718392331665093,
1.25806088877297));
#23544=CARTESIAN_POINT('Ctrl Pts',(0.133341646618848,-0.100333245437109,
1.25566535132897));
#23545=CARTESIAN_POINT('Ctrl Pts',(0.100185001215565,-0.144398018535696,
1.2519607549767));
#23546=CARTESIAN_POINT('Ctrl Pts',(0.0430250923822119,-0.170401477843065,
1.24825615862443));
#23547=CARTESIAN_POINT('Ctrl Pts',(-0.0119785234848996,-0.166442992757554,
1.24455156227217));
#23548=CARTESIAN_POINT('Ctrl Pts',(-0.0669821393520106,-0.162484507672042,
1.2408469659199));
#23549=CARTESIAN_POINT('Ctrl Pts',(-0.11982946225288,-0.12856407819365,
1.23714236956763));
#23550=CARTESIAN_POINT('Ctrl Pts',(-0.146334615197223,-0.0802055812150856,
1.23343777321536));
#23551=CARTESIAN_POINT('Ctrl Pts',(-0.172839768141565,-0.0318470842365214,
1.22973317686309));
#23552=CARTESIAN_POINT('Ctrl Pts',(-0.17300275112938,0.0309494802422141,
1.22602858051083));
#23553=CARTESIAN_POINT('Ctrl Pts',(-0.14674897407212,0.0794449084066994,
1.22232398415856));
#23554=CARTESIAN_POINT('Ctrl Pts',(-0.12049519701486,0.127940336571185,
1.21861938780629));
#23555=CARTESIAN_POINT('Ctrl Pts',(-0.0678246599125219,0.162134628421419,
1.21491479145402));
#23556=CARTESIAN_POINT('Ctrl Pts',(-0.01284233273225,0.166378572397304,
1.21121019510176));
#23557=CARTESIAN_POINT('Ctrl Pts',(0.0421399944480223,0.170622516373188,
1.20750559874949));
#23558=CARTESIAN_POINT('Ctrl Pts',(0.0994341117062293,0.144916112474723,
1.20380100239722));
#23559=CARTESIAN_POINT('Ctrl Pts',(0.132819041399409,0.101024042211295,
1.20009640604495));
#23560=CARTESIAN_POINT('Ctrl Pts',(0.154580764464244,0.0724133161563545,
1.19768159191696));
#23561=CARTESIAN_POINT('Ctrl Pts',(0.166183499569454,0.0360755201147432,
1.19526677778897));
#23562=CARTESIAN_POINT('Ctrl Pts',(0.166426142970557,-0.000120642765556289,
1.19285196366098));
#23563=CARTESIAN_POINT('Origin',(0.,0.,1.3));
#23564=CARTESIAN_POINT('',(0.166855124306607,-5.00565220619177E-5,1.12285196366098));
#23565=CARTESIAN_POINT('',(0.166664543572935,0.000145872469707454,1.14214803633902));
#23566=CARTESIAN_POINT('',(0.1666,2.04026156737949E-17,1.3));
#23567=CARTESIAN_POINT('Ctrl Pts',(0.166664543572935,0.000145872469707454,
1.14214803633902));
#23568=CARTESIAN_POINT('Ctrl Pts',(0.166763206461382,0.0109113832732099,
1.14286887327928));
#23569=CARTESIAN_POINT('Ctrl Pts',(0.165809417829237,0.0216594859626649,
1.14358971021953));
#23570=CARTESIAN_POINT('Ctrl Pts',(0.163739663996808,0.0321882103916611,
1.14431054715979));
#23571=CARTESIAN_POINT('Ctrl Pts',(0.153102580809897,0.0862984701957669,
1.14801514351206));
#23572=CARTESIAN_POINT('Ctrl Pts',(0.112990188231545,0.134614425572516,
1.15171973986433));
#23573=CARTESIAN_POINT('Ctrl Pts',(0.0617601501778567,0.155024005573456,
1.1554243362166));
#23574=CARTESIAN_POINT('Ctrl Pts',(0.010530112124168,0.175433585574396,
1.15912893256886));
#23575=CARTESIAN_POINT('Ctrl Pts',(-0.0518175714048562,0.167936790199525,
1.16283352892113));
#23576=CARTESIAN_POINT('Ctrl Pts',(-0.0967491295066884,0.135964570361971,
1.1665381252734));
#23577=CARTESIAN_POINT('Ctrl Pts',(-0.14168068760852,0.103992350524416,
1.17024272162567));
#23578=CARTESIAN_POINT('Ctrl Pts',(-0.16919612028316,0.0475447062241783,
1.17394731797794));
#23579=CARTESIAN_POINT('Ctrl Pts',(-0.166702833743975,-0.00754477804487655,
1.1776519143302));
#23580=CARTESIAN_POINT('Ctrl Pts',(-0.16420954720479,-0.0626342623139314,
1.18135651068247));
#23581=CARTESIAN_POINT('Ctrl Pts',(-0.131707541451779,-0.116365586551803,
1.18506110703474));
#23582=CARTESIAN_POINT('Ctrl Pts',(-0.0840715437167003,-0.144148305543673,
1.18876570338701));
#23583=CARTESIAN_POINT('Ctrl Pts',(-0.0364355459816213,-0.171931024535542,
1.19247029973928));
#23584=CARTESIAN_POINT('Ctrl Pts',(0.0263344437355261,-0.17376513828141,
1.19617489609154));
#23585=CARTESIAN_POINT('Ctrl Pts',(0.0755113837106313,-0.148811254225361,
1.19987949244381));
#23586=CARTESIAN_POINT('Ctrl Pts',(0.124688323685737,-0.123857370169311,
1.20358408879608));
#23587=CARTESIAN_POINT('Ctrl Pts',(0.1602722139188,-0.0721154883113449,
1.20728868514835));
#23588=CARTESIAN_POINT('Ctrl Pts',(0.165977885270282,-0.0172655742801778,
1.21099328150062));
#23589=CARTESIAN_POINT('Ctrl Pts',(0.166570721031857,-0.011566509515692,
1.21137819978008));
#23590=CARTESIAN_POINT('Ctrl Pts',(0.166840997182384,-0.00583389102255577,
1.21176311805955));
#23591=CARTESIAN_POINT('Ctrl Pts',(0.16680112293357,-9.74720745467285E-5,
1.21214803633902));
#23592=CARTESIAN_POINT('Ctrl Pts',(0.166426142970557,-0.000120642765556289,
1.19285196366098));
#23593=CARTESIAN_POINT('Ctrl Pts',(0.166555741825373,-0.0194534630140944,
1.1915621814367));
#23594=CARTESIAN_POINT('Ctrl Pts',(0.163444578249431,-0.0387458787095636,
1.19027239921243));
#23595=CARTESIAN_POINT('Ctrl Pts',(0.156909640667809,-0.0567989395012422,
1.18898261698815));
#23596=CARTESIAN_POINT('Ctrl Pts',(0.138139568114877,-0.108652114321963,
1.18527802063588));
#23597=CARTESIAN_POINT('Ctrl Pts',(0.0911236808808596,-0.150280727335013,
1.18157342428361));
#23598=CARTESIAN_POINT('Ctrl Pts',(0.0373790663566119,-0.162633207744568,
1.17786882793134));
#23599=CARTESIAN_POINT('Ctrl Pts',(-0.0163655481676351,-0.174985688154123,
1.17416423157907));
#23600=CARTESIAN_POINT('Ctrl Pts',(-0.0768388899821125,-0.158062035960183,
1.17045963522681));
#23601=CARTESIAN_POINT('Ctrl Pts',(-0.116364991298242,-0.119607456553155,
1.16675503887454));
#23602=CARTESIAN_POINT('Ctrl Pts',(-0.155891092614372,-0.0811528771461272,
1.16305044252227));
#23603=CARTESIAN_POINT('Ctrl Pts',(-0.174469953432153,-0.0211673705260111,
1.15934584617));
#23604=CARTESIAN_POINT('Ctrl Pts',(-0.163598852749046,0.0328963560619538,
1.15564124981773));
#23605=CARTESIAN_POINT('Ctrl Pts',(-0.152727752065939,0.0869600826499182,
1.15193665346547));
#23606=CARTESIAN_POINT('Ctrl Pts',(-0.112406689881943,0.135102029205731,
1.1482320571132));
#23607=CARTESIAN_POINT('Ctrl Pts',(-0.061088828941493,0.155289760903929,
1.14452746076093));
#23608=CARTESIAN_POINT('Ctrl Pts',(-0.00977096800104246,0.175477492602127,
1.14082286440866));
#23609=CARTESIAN_POINT('Ctrl Pts',(0.0525436916958626,0.16771100944271,
1.13711826805639));
#23610=CARTESIAN_POINT('Ctrl Pts',(0.0973364927906947,0.135544686484056,
1.13341367170413));
#23611=CARTESIAN_POINT('Ctrl Pts',(0.139904197214479,0.10497623587064,1.12989310235641));
#23612=CARTESIAN_POINT('Ctrl Pts',(0.166647613265987,0.0523718751412305,
1.12637253300869));
#23613=CARTESIAN_POINT('Ctrl Pts',(0.166855124306607,-5.00565220619177E-5,
1.12285196366098));
#23614=CARTESIAN_POINT('Origin',(0.,0.,1.3));
#23615=CARTESIAN_POINT('',(0.166573628657937,0.000152187718365226,1.05285196366098));
#23616=CARTESIAN_POINT('',(0.166327182499917,6.33242585386815E-6,1.07214803633902));
#23617=CARTESIAN_POINT('',(0.1666,2.04026156737949E-17,1.3));
#23618=CARTESIAN_POINT('Ctrl Pts',(0.166327182499917,6.33242585386815E-6,
1.07214803633902));
#23619=CARTESIAN_POINT('Ctrl Pts',(0.166336479007403,0.0274263312352492,
1.073974628499));
#23620=CARTESIAN_POINT('Ctrl Pts',(0.159932481000657,0.0548422420648042,
1.07580122065898));
#23621=CARTESIAN_POINT('Ctrl Pts',(0.147091342637332,0.0788092340673142,
1.07762781281897));
#23622=CARTESIAN_POINT('Ctrl Pts',(0.121047633821556,0.127417803124253,
1.08133240917123));
#23623=CARTESIAN_POINT('Ctrl Pts',(0.0685255340861956,0.161839665678967,
1.0850370055235));
#23624=CARTESIAN_POINT('Ctrl Pts',(0.0135620801901698,0.166321461139012,
1.08874160187577));
#23625=CARTESIAN_POINT('Ctrl Pts',(-0.0414013737058552,0.170803256599056,
1.09244619822804));
#23626=CARTESIAN_POINT('Ctrl Pts',(-0.0988061817625453,0.145344984964431,
1.09615079458031));
#23627=CARTESIAN_POINT('Ctrl Pts',(-0.132380708062468,0.101597768611665,
1.09985539093257));
#23628=CARTESIAN_POINT('Ctrl Pts',(-0.165955234362392,0.0578505522588977,
1.10355998728484));
#23629=CARTESIAN_POINT('Ctrl Pts',(-0.175699478905547,-0.00418560881201081,
1.10726458363711));
#23630=CARTESIAN_POINT('Ctrl Pts',(-0.157153932924644,-0.0561195137204682,
1.11096917998938));
#23631=CARTESIAN_POINT('Ctrl Pts',(-0.13860838694374,-0.108053418628926,
1.11467377634165));
#23632=CARTESIAN_POINT('Ctrl Pts',(-0.0917730504387764,-0.149885067374932,
1.11837837269391));
#23633=CARTESIAN_POINT('Ctrl Pts',(-0.0380823807348833,-0.162469968707007,
1.12208296904618));
#23634=CARTESIAN_POINT('Ctrl Pts',(0.0156082889690095,-0.175054870039082,
1.12578756539845));
#23635=CARTESIAN_POINT('Ctrl Pts',(0.076154291871832,-0.158393023957226,
1.12949216175072));
#23636=CARTESIAN_POINT('Ctrl Pts',(0.115846406425509,-0.120109818800568,
1.13319675810299));
#23637=CARTESIAN_POINT('Ctrl Pts',(0.147815265950422,-0.0892757243821015,
1.136180517515));
#23638=CARTESIAN_POINT('Ctrl Pts',(0.16625614840673,-0.044415792438328,
1.13916427692701));
#23639=CARTESIAN_POINT('Ctrl Pts',(0.166664543572935,0.000145872469707454,
1.14214803633902));
#23640=CARTESIAN_POINT('Ctrl Pts',(0.166855124306607,-5.00565220619177E-5,
1.12285196366098));
#23641=CARTESIAN_POINT('Ctrl Pts',(0.166865971312146,-0.00279025280966625,
1.12266793665643));
#23642=CARTESIAN_POINT('Ctrl Pts',(0.166804312774377,-0.00552995063608946,
1.12248390965187));
#23643=CARTESIAN_POINT('Ctrl Pts',(0.166668618800564,-0.00826597665440976,
1.12229988264732));
#23644=CARTESIAN_POINT('Ctrl Pts',(0.163937001222843,-0.0633441540763332,
1.11859528629505));
#23645=CARTESIAN_POINT('Ctrl Pts',(0.131202823574641,-0.116934346162291,
1.11489068994278));
#23646=CARTESIAN_POINT('Ctrl Pts',(0.0834470678717536,-0.144510697621526,
1.11118609359052));
#23647=CARTESIAN_POINT('Ctrl Pts',(0.035691312168866,-0.172087049080761,
1.10748149723825));
#23648=CARTESIAN_POINT('Ctrl Pts',(-0.0270860215887074,-0.173649559913274,
1.10377690088598));
#23649=CARTESIAN_POINT('Ctrl Pts',(-0.0761545306345133,-0.148483138187173,
1.10007230453371));
#23650=CARTESIAN_POINT('Ctrl Pts',(-0.125223039680319,-0.123316716461072,
1.09636770818145));
#23651=CARTESIAN_POINT('Ctrl Pts',(-0.160582724014357,-0.0714213621763564,
1.09266311182918));
#23652=CARTESIAN_POINT('Ctrl Pts',(-0.166051023599269,-0.0165472784677163,
1.08895851547691));
#23653=CARTESIAN_POINT('Ctrl Pts',(-0.171519323184182,0.0383268052409238,
1.08525391912464));
#23654=CARTESIAN_POINT('Ctrl Pts',(-0.147096238019968,0.0961796183734885,
1.08154932277237));
#23655=CARTESIAN_POINT('Ctrl Pts',(-0.103959131518119,0.130534492913072,
1.0778447264201));
#23656=CARTESIAN_POINT('Ctrl Pts',(-0.0608220250162706,0.164889367452656,
1.07414013006784));
#23657=CARTESIAN_POINT('Ctrl Pts',(0.0010291028232132,0.175746303399259,
1.07043553371557));
#23658=CARTESIAN_POINT('Ctrl Pts',(0.0532877326205867,0.15813656252862,
1.0667309373633));
#23659=CARTESIAN_POINT('Ctrl Pts',(0.10554636241796,0.140526821657981,1.06302634101103));
#23660=CARTESIAN_POINT('Ctrl Pts',(0.148212494173223,0.0944504039700999,
1.05932174465876));
#23661=CARTESIAN_POINT('Ctrl Pts',(0.161759730763308,0.0409944431478461,
1.0556171483065));
#23662=CARTESIAN_POINT('Ctrl Pts',(0.165130373342236,0.0276942445097812,
1.05469542009132));
#23663=CARTESIAN_POINT('Ctrl Pts',(0.16669841799434,0.0139372170985273,
1.05377369187615));
#23664=CARTESIAN_POINT('Ctrl Pts',(0.166573628657937,0.000152187718365227,
1.05285196366098));
#23665=CARTESIAN_POINT('Origin',(0.,0.,1.3));
#23666=CARTESIAN_POINT('',(0.16633703813182,-4.26131537097363E-5,0.982851963660979));
#23667=CARTESIAN_POINT('',(0.166641299058679,-0.000149160109009599,1.00214803633902));
#23668=CARTESIAN_POINT('',(0.1666,2.04026156737949E-17,1.3));
#23669=CARTESIAN_POINT('Ctrl Pts',(0.166641299058679,-0.000149160109009599,
1.00214803633902));
#23670=CARTESIAN_POINT('Ctrl Pts',(0.166236990763482,0.0436603970157784,
1.00508038371873));
#23671=CARTESIAN_POINT('Ctrl Pts',(0.148493576846311,0.0877597158867868,
1.00801273109843));
#23672=CARTESIAN_POINT('Ctrl Pts',(0.117498076053599,0.118494559065924,
1.01094507847814));
#23673=CARTESIAN_POINT('Ctrl Pts',(0.0783397485075339,0.157323583456734,
1.01464967483041));
#23674=CARTESIAN_POINT('Ctrl Pts',(0.0180302104029479,0.174822017275825,
1.01835427118268));
#23675=CARTESIAN_POINT('Ctrl Pts',(-0.0358295364409326,0.162981602616999,
1.02205886753494));
#23676=CARTESIAN_POINT('Ctrl Pts',(-0.089689283284813,0.151141187958173,
1.02576346388721));
#23677=CARTESIAN_POINT('Ctrl Pts',(-0.137099238867988,0.10996192482143,
1.02946806023948));
#23678=CARTESIAN_POINT('Ctrl Pts',(-0.156361968042692,0.0582897367165174,
1.03317265659175));
#23679=CARTESIAN_POINT('Ctrl Pts',(-0.175624697217396,0.00661754861160513,
1.03687725294402));
#23680=CARTESIAN_POINT('Ctrl Pts',(-0.166740199983629,-0.0555475644614757,
1.04058184929629));
#23681=CARTESIAN_POINT('Ctrl Pts',(-0.133774516953309,-0.0997553861262926,
1.04428644564855));
#23682=CARTESIAN_POINT('Ctrl Pts',(-0.100808833922988,-0.143963207791109,
1.04799104200082));
#23683=CARTESIAN_POINT('Ctrl Pts',(-0.0437619650961137,-0.170213738047662,
1.05169563835309));
#23684=CARTESIAN_POINT('Ctrl Pts',(0.0112582665697782,-0.166493272809894,
1.05540023470536));
#23685=CARTESIAN_POINT('Ctrl Pts',(0.0662784982356701,-0.162772807572126,
1.05910483105763));
#23686=CARTESIAN_POINT('Ctrl Pts',(0.11927209274058,-0.129081346840038,
1.06280942740989));
#23687=CARTESIAN_POINT('Ctrl Pts',(0.145986231044939,-0.0808379786944121,
1.06651402376216));
#23688=CARTESIAN_POINT('Ctrl Pts',(0.159528668319701,-0.0563815362072228,
1.06839202795445));
#23689=CARTESIAN_POINT('Ctrl Pts',(0.166317624329016,-0.0281854412194699,
1.07027003214673));
#23690=CARTESIAN_POINT('Ctrl Pts',(0.166327182499917,6.33242585386815E-6,
1.07214803633902));
#23691=CARTESIAN_POINT('Ctrl Pts',(0.166573628657937,0.000152187718365227,
1.05285196366098));
#23692=CARTESIAN_POINT('Ctrl Pts',(0.166196866546928,-0.0414673682413184,
1.05006909552388));
#23693=CARTESIAN_POINT('Ctrl Pts',(0.150389111841613,-0.0833421755592448,
1.04728622738679));
#23694=CARTESIAN_POINT('Ctrl Pts',(0.122171212866625,-0.113670355101641,
1.04450335924969));
#23695=CARTESIAN_POINT('Ctrl Pts',(0.0846071169549502,-0.154043688572246,
1.04079876289742));
#23696=CARTESIAN_POINT('Ctrl Pts',(0.0250505837066941,-0.173954851556829,
1.03709416654516));
#23697=CARTESIAN_POINT('Ctrl Pts',(-0.0292420016986911,-0.164291387935873,
1.03338957019289));
#23698=CARTESIAN_POINT('Ctrl Pts',(-0.0835345871040766,-0.154627924314917,
1.02968497384062));
#23699=CARTESIAN_POINT('Ctrl Pts',(-0.132563224666591,-0.115389834088422,
1.02598037748835));
#23700=CARTESIAN_POINT('Ctrl Pts',(-0.153889680451665,-0.0645346507397467,
1.02227578113608));
#23701=CARTESIAN_POINT('Ctrl Pts',(-0.175216136236738,-0.0136794673910717,
1.01857118478382));
#23702=CARTESIAN_POINT('Ctrl Pts',(-0.16884041024437,0.0487928090797828,
1.01486658843155));
#23703=CARTESIAN_POINT('Ctrl Pts',(-0.137680389518285,0.0942913851820011,
1.01116199207928));
#23704=CARTESIAN_POINT('Ctrl Pts',(-0.106520368792199,0.139789961284219,
1.00745739572701));
#23705=CARTESIAN_POINT('Ctrl Pts',(-0.0505760533323975,0.168314837017802,
1.00375279937474));
#23706=CARTESIAN_POINT('Ctrl Pts',(0.00454932345543924,0.166811444936069,
1.00004820302248));
#23707=CARTESIAN_POINT('Ctrl Pts',(0.0596747002432758,0.165308052854335,
0.996343606670208));
#23708=CARTESIAN_POINT('Ctrl Pts',(0.113981138359147,0.133776392957287,
0.992639010317939));
#23709=CARTESIAN_POINT('Ctrl Pts',(0.142614988862282,0.0866471011481969,
0.988934413965671));
#23710=CARTESIAN_POINT('Ctrl Pts',(0.158285969463688,0.0608537759501981,
0.986906930530773));
#23711=CARTESIAN_POINT('Ctrl Pts',(0.166267372459907,0.0303885726052033,
0.984879447095876));
#23712=CARTESIAN_POINT('Ctrl Pts',(0.16633703813182,-4.26131537097363E-5,
0.982851963660979));
#23713=CARTESIAN_POINT('Origin',(0.,0.,1.3));
#23714=CARTESIAN_POINT('',(0.166729862742343,-0.000130123946020723,0.912851963660979));
#23715=CARTESIAN_POINT('',(0.16681765906064,8.64047405809373E-5,0.93214803633902));
#23716=CARTESIAN_POINT('',(0.1666,2.04026156737949E-17,1.3));
#23717=CARTESIAN_POINT('Ctrl Pts',(0.16681765906064,8.64047405809373E-5,
0.93214803633902));
#23718=CARTESIAN_POINT('Ctrl Pts',(0.166849023174239,0.00505533653555562,
0.932481542586184));
#23719=CARTESIAN_POINT('Ctrl Pts',(0.166646252238729,0.0100216728157887,
0.932815048833348));
#23720=CARTESIAN_POINT('Ctrl Pts',(0.166201007638075,0.0149661744225974,
0.933148555080512));
#23721=CARTESIAN_POINT('Ctrl Pts',(0.161255218653678,0.0698898310921401,
0.93685315143278));
#23722=CARTESIAN_POINT('Ctrl Pts',(0.126391025843356,0.122119345383236,
0.940557747785048));
#23723=CARTESIAN_POINT('Ctrl Pts',(0.0775642504900456,0.147751626038697,
0.944262344137316));
#23724=CARTESIAN_POINT('Ctrl Pts',(0.0287374751367354,0.173383906694158,
0.947966940489584));
#23725=CARTESIAN_POINT('Ctrl Pts',(-0.0340518827595631,0.172418953713984,
0.951671536841852));
#23726=CARTESIAN_POINT('Ctrl Pts',(-0.0820679309643883,0.145298361306226,
0.95537613319412));
#23727=CARTESIAN_POINT('Ctrl Pts',(-0.130083979169214,0.118177768898468,
0.959080729546388));
#23728=CARTESIAN_POINT('Ctrl Pts',(-0.163326717682566,0.0649015370631265,
0.962785325898656));
#23729=CARTESIAN_POINT('Ctrl Pts',(-0.166582411702781,0.00985184688226562,
0.966489922250924));
#23730=CARTESIAN_POINT('Ctrl Pts',(-0.169838105722997,-0.045197843298595,
0.970194518603192));
#23731=CARTESIAN_POINT('Ctrl Pts',(-0.143106755250076,-0.102020991824975,
0.97389911495546));
#23732=CARTESIAN_POINT('Ctrl Pts',(-0.0986221180718627,-0.134612168562546,
0.977603711307728));
#23733=CARTESIAN_POINT('Ctrl Pts',(-0.054137480893649,-0.167203345300117,
0.981308307659997));
#23734=CARTESIAN_POINT('Ctrl Pts',(0.00810044298985758,-0.175562550248879,
0.985012904012265));
#23735=CARTESIAN_POINT('Ctrl Pts',(0.0596081167151753,-0.155864142731977,
0.988717500364533));
#23736=CARTESIAN_POINT('Ctrl Pts',(0.111115790440493,-0.136165735215075,
0.992422096716801));
#23737=CARTESIAN_POINT('Ctrl Pts',(0.151893214007622,-0.0884097152325082,
0.996126693069068));
#23738=CARTESIAN_POINT('Ctrl Pts',(0.163278367297414,-0.0344518977599609,
0.999831289421336));
#23739=CARTESIAN_POINT('Ctrl Pts',(0.165651681983942,-0.0232040140116242,
1.0006035383939));
#23740=CARTESIAN_POINT('Ctrl Pts',(0.166747775756401,-0.0116866354136458,
1.00137578736646));
#23741=CARTESIAN_POINT('Ctrl Pts',(0.166641299058679,-0.000149160109009599,
1.00214803633902));
#23742=CARTESIAN_POINT('Ctrl Pts',(0.16633703813182,-4.26131537097363E-5,
0.982851963660979));
#23743=CARTESIAN_POINT('Ctrl Pts',(0.166394664840996,-0.0252149691141755,
0.981174850743608));
#23744=CARTESIAN_POINT('Ctrl Pts',(0.161038745460081,-0.0503640488000913,
0.979497737826238));
#23745=CARTESIAN_POINT('Ctrl Pts',(0.150143538011669,-0.0728263241997442,
0.977820624908867));
#23746=CARTESIAN_POINT('Ctrl Pts',(0.126076973767522,-0.122443534017465,
0.974116028556599));
#23747=CARTESIAN_POINT('Ctrl Pts',(0.0749825823888285,-0.158951029931774,
0.970411432204331));
#23748=CARTESIAN_POINT('Ctrl Pts',(0.0202440032863241,-0.165640975250716,
0.966706835852062));
#23749=CARTESIAN_POINT('Ctrl Pts',(-0.0344945758161804,-0.172330920569658,
0.963002239499794));
#23750=CARTESIAN_POINT('Ctrl Pts',(-0.0928773426424964,-0.149203315293232,
0.959297643147526));
#23751=CARTESIAN_POINT('Ctrl Pts',(-0.128185095718787,-0.106842589675449,
0.955593046795258));
#23752=CARTESIAN_POINT('Ctrl Pts',(-0.163492848795077,-0.064481864057666,
0.95188845044299));
#23753=CARTESIAN_POINT('Ctrl Pts',(-0.175725588121342,-0.00288801809852563,
0.948183854090722));
#23754=CARTESIAN_POINT('Ctrl Pts',(-0.159284925787188,0.0497500806758803,
0.944479257738454));
#23755=CARTESIAN_POINT('Ctrl Pts',(-0.142844263453034,0.102388179450286,
0.940774661386186));
#23756=CARTESIAN_POINT('Ctrl Pts',(-0.097730199458461,0.146070531039958,
0.937070065033918));
#23757=CARTESIAN_POINT('Ctrl Pts',(-0.0445894513306832,0.160805840780395,
0.93336546868165));
#23758=CARTESIAN_POINT('Ctrl Pts',(0.00855129679709463,0.175541150520831,
0.929660872329382));
#23759=CARTESIAN_POINT('Ctrl Pts',(0.0697187290580771,0.161329418412033,
0.925956275977114));
#23760=CARTESIAN_POINT('Ctrl Pts',(0.110919243004777,0.124674377251528,
0.922251679624846));
#23761=CARTESIAN_POINT('Ctrl Pts',(0.145765426127824,0.093672621343478,
0.919118440970224));
#23762=CARTESIAN_POINT('Ctrl Pts',(0.16632871557528,0.0466165403829395,
0.915985202315602));
#23763=CARTESIAN_POINT('Ctrl Pts',(0.166729862742343,-0.000130123946020723,
0.912851963660979));
#23764=CARTESIAN_POINT('Origin',(0.,0.,1.3));
#23765=CARTESIAN_POINT('',(0.166745353727506,0.000120148921586877,0.842851963660979));
#23766=CARTESIAN_POINT('',(0.166381444272219,9.40568719243839E-5,0.86214803633902));
#23767=CARTESIAN_POINT('',(0.1666,2.04026156737949E-17,1.3));
#23768=CARTESIAN_POINT('',(-0.126907087985236,0.107935865304853,0.8));
#23769=CARTESIAN_POINT('Ctrl Pts',(0.166745353727506,0.000120148921586877,
0.842851963660979));
#23770=CARTESIAN_POINT('Ctrl Pts',(0.166350216338014,-0.0471541035618327,
0.83968176483079));
#23771=CARTESIAN_POINT('Ctrl Pts',(0.14523873930488,-0.0947247812496833,
0.836511566000602));
#23772=CARTESIAN_POINT('Ctrl Pts',(0.109671969299941,-0.125754000901643,
0.833341367170413));
#23773=CARTESIAN_POINT('Ctrl Pts',(0.0681097413514803,-0.162013787777386,
0.829636770818145));
#23774=CARTESIAN_POINT('Ctrl Pts',(0.00680803444401046,-0.175685325249421,
0.825932174465876));
#23775=CARTESIAN_POINT('Ctrl Pts',(-0.0461862781086293,-0.160386912096395,
0.822227578113608));
#23776=CARTESIAN_POINT('Ctrl Pts',(-0.0991805906612692,-0.14508849894337,
0.81852298176134));
#23777=CARTESIAN_POINT('Ctrl Pts',(-0.143867508859079,-0.100820135165284,
0.814818385409072));
#23778=CARTESIAN_POINT('Ctrl Pts',(-0.159771943968926,-0.0481139506034528,
0.811113789056804));
#23779=CARTESIAN_POINT('Ctrl Pts',(-0.175676379078773,0.00459223395837816,
0.807409192704537));
#23780=CARTESIAN_POINT('Ctrl Pts',(-0.162798331100657,0.0657362393039545,
0.803704596352268));
#23781=CARTESIAN_POINT('Ctrl Pts',(-0.126907087985236,0.107935865304854,
0.8));
#23782=CARTESIAN_POINT('',(0.127144529223414,0.10812516429919,0.8));
#23783=CARTESIAN_POINT('Origin',(0.,0.,0.8));
#23784=CARTESIAN_POINT('Ctrl Pts',(0.127144588893496,0.108125211870903,
0.8));
#23785=CARTESIAN_POINT('Ctrl Pts',(0.0920578520263333,0.149281442964014,
0.803632291818556));
#23786=CARTESIAN_POINT('Ctrl Pts',(0.0350626176413565,0.171873117908773,
0.807264583637111));
#23787=CARTESIAN_POINT('Ctrl Pts',(-0.0186760721562392,0.165810809841732,
0.810896875455666));
#23788=CARTESIAN_POINT('Ctrl Pts',(-0.0734844862772781,0.159627825248711,
0.814601471807934));
#23789=CARTESIAN_POINT('Ctrl Pts',(-0.124905415613006,0.123638729028309,
0.818306068160202));
#23790=CARTESIAN_POINT('Ctrl Pts',(-0.14943866399484,0.0742601129650432,
0.82201066451247));
#23791=CARTESIAN_POINT('Ctrl Pts',(-0.173971912376674,0.0248814969017771,
0.825715260864738));
#23792=CARTESIAN_POINT('Ctrl Pts',(-0.171617479804614,-0.0378866390043534,
0.829419857217006));
#23793=CARTESIAN_POINT('Ctrl Pts',(-0.143435789399569,-0.0852901107552215,
0.833124453569274));
#23794=CARTESIAN_POINT('Ctrl Pts',(-0.115254098994523,-0.132693582506089,
0.836829049921542));
#23795=CARTESIAN_POINT('Ctrl Pts',(-0.0612451507564931,-0.164732390101695,
0.84053364627381));
#23796=CARTESIAN_POINT('Ctrl Pts',(-0.00613536544337925,-0.166758384009028,
0.844238242626078));
#23797=CARTESIAN_POINT('Ctrl Pts',(0.0489744198697346,-0.168784377916361,
0.847942838978346));
#23798=CARTESIAN_POINT('Ctrl Pts',(0.105185042257932,-0.140797558135422,
0.851647435330614));
#23799=CARTESIAN_POINT('Ctrl Pts',(0.136776048425978,-0.0955986339274043,
0.855352031682883));
#23800=CARTESIAN_POINT('Ctrl Pts',(0.156093728823978,-0.0679598063592257,
0.857617366568262));
#23801=CARTESIAN_POINT('Ctrl Pts',(0.166205550297931,-0.0338849643656092,
0.859882701453641));
#23802=CARTESIAN_POINT('Ctrl Pts',(0.166381444272219,9.40568719243839E-5,
0.86214803633902));
#23803=CARTESIAN_POINT('Origin',(0.,0.,0.645407471946233));
#23804=CARTESIAN_POINT('',(0.205717919156333,0.000119231682504745,1.65459252805377));
#23805=CARTESIAN_POINT('',(0.20515534870289,-8.10795385496472E-5,1.66040747194623));
#23806=CARTESIAN_POINT('',(0.205475,1.17874941047504E-14,0.645407471946233));
#23807=CARTESIAN_POINT('',(-0.188262750966373,-0.0823232180103128,1.7));
#23808=CARTESIAN_POINT('Ctrl Pts',(0.20515534870289,-8.1079538549661E-5,
1.66040747194623));
#23809=CARTESIAN_POINT('Ctrl Pts',(0.205035475209089,0.0384765991859779,
1.66249119224068));
#23810=CARTESIAN_POINT('Ctrl Pts',(0.176046579400947,0.14575433740106,1.6682795088874));
#23811=CARTESIAN_POINT('Ctrl Pts',(0.00300247275662535,0.243001989931863,
1.67777242188639));
#23812=CARTESIAN_POINT('Ctrl Pts',(-0.202554499717183,0.133854462473394,
1.6888862109432));
#23813=CARTESIAN_POINT('Ctrl Pts',(-0.215637179506013,-0.0197213743559566,
1.69629540364773));
#23814=CARTESIAN_POINT('Ctrl Pts',(-0.188262750966373,-0.0823232180103128,
1.7));
#23815=CARTESIAN_POINT('',(-0.122364587709818,-0.165532040449643,1.7));
#23816=CARTESIAN_POINT('Origin',(0.,0.,1.7));
#23817=CARTESIAN_POINT('Ctrl Pts',(0.205717919156333,0.000119231682504748,
1.65459252805377));
#23818=CARTESIAN_POINT('Ctrl Pts',(0.205768208325854,0.00728313946640584,
1.65498227116049));
#23819=CARTESIAN_POINT('Ctrl Pts',(0.202179510783538,0.0824912465572326,
1.65907661061947));
#23820=CARTESIAN_POINT('Ctrl Pts',(0.109634140470589,0.216730418270261,
1.66687554643072));
#23821=CARTESIAN_POINT('Ctrl Pts',(-0.122663843019391,0.209602590285094,
1.67798933548753));
#23822=CARTESIAN_POINT('Ctrl Pts',(-0.24177601945125,0.0120092944511596,
1.68903082001062));
#23823=CARTESIAN_POINT('Ctrl Pts',(-0.175954082167323,-0.125816077227026,
1.69636770818144));
#23824=CARTESIAN_POINT('Ctrl Pts',(-0.122364641233049,-0.165532117868825,
1.7));
#23825=CARTESIAN_POINT('Origin',(0.,0.,0.645407471946233));
#23826=CARTESIAN_POINT('',(0.2051889883028,0.000102640746213675,1.58459252805377));
#23827=CARTESIAN_POINT('',(0.205663604651154,-0.000149728163284854,1.59040747194623));
#23828=CARTESIAN_POINT('',(0.205475,1.17874941047504E-14,0.645407471946233));
#23829=CARTESIAN_POINT('Ctrl Pts',(0.205663604651154,-0.000149728163284867,
1.59040747194623));
#23830=CARTESIAN_POINT('Ctrl Pts',(0.205182444335985,0.0585183956951034,
1.59359694746041));
#23831=CARTESIAN_POINT('Ctrl Pts',(0.148135327616145,0.186146531383155,
1.60049101932685));
#23832=CARTESIAN_POINT('Ctrl Pts',(-0.0684290720584363,0.233024356666725,
1.61108968754557));
#23833=CARTESIAN_POINT('Ctrl Pts',(-0.23288917800895,0.0688795811193509,
1.62220347660237));
#23834=CARTESIAN_POINT('Ctrl Pts',(-0.184175405168835,-0.158290127824162,
1.63331726565918));
#23835=CARTESIAN_POINT('Ctrl Pts',(0.0331013206128567,-0.240615925517378,
1.64443105471598));
#23836=CARTESIAN_POINT('Ctrl Pts',(0.185046630854554,-0.128496885183325,
1.65346112347833));
#23837=CARTESIAN_POINT('Ctrl Pts',(0.205248595419634,-0.0300741733602017,
1.65878659588842));
#23838=CARTESIAN_POINT('Ctrl Pts',(0.20515534870289,-8.1079538549661E-5,
1.66040747194623));
#23839=CARTESIAN_POINT('Ctrl Pts',(0.2051889883028,0.000102640746213654,
1.58459252805377));
#23840=CARTESIAN_POINT('Ctrl Pts',(0.205314142408481,0.0277738688435417,
1.58608802638021));
#23841=CARTESIAN_POINT('Ctrl Pts',(0.187212802641802,0.123834372120327,
1.59128812105892));
#23842=CARTESIAN_POINT('Ctrl Pts',(0.041212233239435,0.2393392912824,1.6001928120899));
#23843=CARTESIAN_POINT('Ctrl Pts',(-0.178731921787321,0.164428017156146,
1.6113066011467));
#23844=CARTESIAN_POINT('Ctrl Pts',(-0.235078089364662,-0.0609842187918821,
1.62242039020351));
#23845=CARTESIAN_POINT('Ctrl Pts',(-0.0762596568913861,-0.230580482955351,
1.63353417926032));
#23846=CARTESIAN_POINT('Ctrl Pts',(0.144352083897931,-0.190571029763675,
1.6442582252104));
#23847=CARTESIAN_POINT('Ctrl Pts',(0.205290198398921,-0.0608114238158697,
1.65127767480822));
#23848=CARTESIAN_POINT('Ctrl Pts',(0.205717919156333,0.000119231682504748,
1.65459252805377));
#23849=CARTESIAN_POINT('Origin',(0.,0.,0.645407471946233));
#23850=CARTESIAN_POINT('',(0.205346259354759,-0.00017652456807675,1.51459252805377));
#23851=CARTESIAN_POINT('',(0.205625119184624,0.000163390229490382,1.52040747194623));
#23852=CARTESIAN_POINT('',(0.205475,1.17874941047504E-14,0.645407471946233));
#23853=CARTESIAN_POINT('Ctrl Pts',(0.205625119184624,0.000163390229490371,
1.52040747194623));
#23854=CARTESIAN_POINT('Ctrl Pts',(0.205719589271595,0.0110330279545173,
1.52099810632787));
#23855=CARTESIAN_POINT('Ctrl Pts',(0.199992588366042,0.0899798330776656,
1.52529333706177));
#23856=CARTESIAN_POINT('Ctrl Pts',(0.0977367556084749,0.222326520064881,
1.53329316414794));
#23857=CARTESIAN_POINT('Ctrl Pts',(-0.133782052044684,0.202691772286445,
1.54440695320474));
#23858=CARTESIAN_POINT('Ctrl Pts',(-0.242848712699985,-0.00246927953082339,
1.55552074226155));
#23859=CARTESIAN_POINT('Ctrl Pts',(-0.129633034711377,-0.205369738746763,
1.56663453131835));
#23860=CARTESIAN_POINT('Ctrl Pts',(0.102236927935064,-0.220293776124516,
1.57774832037515));
#23861=CARTESIAN_POINT('Ctrl Pts',(0.20084133199376,-0.0871629660671419,
1.58567263391778));
#23862=CARTESIAN_POINT('Ctrl Pts',(0.205741315141077,-0.00962500803198312,
1.58989235110814));
#23863=CARTESIAN_POINT('Ctrl Pts',(0.205663604651154,-0.000149728163284867,
1.59040747194623));
#23864=CARTESIAN_POINT('Ctrl Pts',(0.205346259354759,-0.000176524568076758,
1.51459252805377));
#23865=CARTESIAN_POINT('Ctrl Pts',(0.204952685935524,0.0478618563462208,
1.51719378159994));
#23866=CARTESIAN_POINT('Ctrl Pts',(0.164184854806731,0.1649162911311,1.52349963149837));
#23867=CARTESIAN_POINT('Ctrl Pts',(-0.0308180903310451,0.240897960470908,
1.53351007774908));
#23868=CARTESIAN_POINT('Ctrl Pts',(-0.219105973246366,0.104757609325286,
1.54462386680588));
#23869=CARTESIAN_POINT('Ctrl Pts',(-0.206843620635952,-0.127268531807556,
1.55573765586268));
#23870=CARTESIAN_POINT('Ctrl Pts',(-0.00525505851706014,-0.242804414954791,
1.56685144491949));
#23871=CARTESIAN_POINT('Ctrl Pts',(0.173370196153793,-0.15045712725832,
1.57646973564985));
#23872=CARTESIAN_POINT('Ctrl Pts',(0.20500411501816,-0.0407723333551383,
1.58238343002794));
#23873=CARTESIAN_POINT('Ctrl Pts',(0.2051889883028,0.000102640746213654,
1.58459252805377));
#23874=CARTESIAN_POINT('Origin',(0.,0.,0.645407471946233));
#23875=CARTESIAN_POINT('',(0.205812292792875,8.2771271442428E-7,1.44459252805377));
#23876=CARTESIAN_POINT('',(0.20514810115636,4.68968264668604E-5,1.45040747194623));
#23877=CARTESIAN_POINT('',(0.205475,1.17874941047504E-14,0.645407471946233));
#23878=CARTESIAN_POINT('Ctrl Pts',(0.20514810115636,4.68968264668648E-5,
1.45040747194623));
#23879=CARTESIAN_POINT('Ctrl Pts',(0.205212209277079,0.0314508805486537,
1.45210386154759));
#23880=CARTESIAN_POINT('Ctrl Pts',(0.183673234943095,0.131351887215635,
1.45750484750122));
#23881=CARTESIAN_POINT('Ctrl Pts',(0.028210615278035,0.241217190661839,
1.46661042980711));
#23882=CARTESIAN_POINT('Ctrl Pts',(-0.187360277963068,0.154524103926572,
1.47772421886392));
#23883=CARTESIAN_POINT('Ctrl Pts',(-0.23143818564818,-0.0736066521476796,
1.48883800792072));
#23884=CARTESIAN_POINT('Ctrl Pts',(-0.0636780941176189,-0.234364395962394,
1.49995179697753));
#23885=CARTESIAN_POINT('Ctrl Pts',(0.15035425339619,-0.183462731047792,
1.51047495165269));
#23886=CARTESIAN_POINT('Ctrl Pts',(0.205127050891722,-0.0571438705105598,
1.5172935099756));
#23887=CARTESIAN_POINT('Ctrl Pts',(0.205625119184624,0.000163390229490371,
1.52040747194623));
#23888=CARTESIAN_POINT('Ctrl Pts',(0.205812290976358,8.27708256686491E-7,
1.44459252805377));
#23889=CARTESIAN_POINT('Ctrl Pts',(0.205812293621698,4.5117938930396E-5,
1.44459494046739));
#23890=CARTESIAN_POINT('Ctrl Pts',(0.205792223959932,0.0681032095145843,
1.44830194923329));
#23891=CARTESIAN_POINT('Ctrl Pts',(0.13158183823911,0.204126920402922,1.45571355435144));
#23892=CARTESIAN_POINT('Ctrl Pts',(-0.10013585656473,0.221256389923926,
1.46682734340825));
#23893=CARTESIAN_POINT('Ctrl Pts',(-0.240198066802314,0.0358673761285168,
1.47794113246505));
#23894=CARTESIAN_POINT('Ctrl Pts',(-0.160404261381875,-0.182351453033287,
1.48905492152186));
#23895=CARTESIAN_POINT('Ctrl Pts',(0.0662093815164626,-0.233661930697804,
1.50016871057866));
#23896=CARTESIAN_POINT('Ctrl Pts',(0.193364787149743,-0.109147888339539,
1.5086812460893));
#23897=CARTESIAN_POINT('Ctrl Pts',(0.20551319671518,-0.0205523937625982,
1.51348918524767));
#23898=CARTESIAN_POINT('Ctrl Pts',(0.205346259354759,-0.000176524568076758,
1.51459252805377));
#23899=CARTESIAN_POINT('Origin',(0.,0.,0.645407471946233));
#23900=CARTESIAN_POINT('',(0.205343844683429,0.000176004178461642,1.37459252805377));
#23901=CARTESIAN_POINT('',(0.205453133831238,-0.000187888241826064,1.38040747194623));
#23902=CARTESIAN_POINT('',(0.205475,1.17874941047504E-14,0.645407471946233));
#23903=CARTESIAN_POINT('Ctrl Pts',(0.205453133831238,-0.000187888241826079,
1.38040747194623));
#23904=CARTESIAN_POINT('Ctrl Pts',(0.204982640394683,0.0514920396676331,
1.38320961676732));
#23905=CARTESIAN_POINT('Ctrl Pts',(0.159017805479884,0.172241441932577,
1.38971635794067));
#23906=CARTESIAN_POINT('Ctrl Pts',(-0.0437982449057285,0.238879228826581,
1.39992769546629));
#23907=CARTESIAN_POINT('Ctrl Pts',(-0.224449621610114,0.0927574233548304,
1.41104148452309));
#23908=CARTESIAN_POINT('Ctrl Pts',(-0.199659714256911,-0.13826630374757,
1.42215527357989));
#23909=CARTESIAN_POINT('Ctrl Pts',(0.00788099391586731,-0.242733314804761,
1.4332690626367));
#23910=CARTESIAN_POINT('Ctrl Pts',(0.177630548818419,-0.142990752308629,
1.44268646209214));
#23911=CARTESIAN_POINT('Ctrl Pts',(0.205072209179237,-0.037129523063069,
1.44839926519532));
#23912=CARTESIAN_POINT('Ctrl Pts',(0.20514810115636,4.68968264668648E-5,
1.45040747194623));
#23913=CARTESIAN_POINT('Ctrl Pts',(0.205343844683429,0.000176004178461609,
1.37459252805377));
#23914=CARTESIAN_POINT('Ctrl Pts',(0.2055108740339,0.0206415845782027,1.37570069568712));
#23915=CARTESIAN_POINT('Ctrl Pts',(0.193294976926761,0.109328542053589,
1.38051345967274));
#23916=CARTESIAN_POINT('Ctrl Pts',(0.0659057470887793,0.233747753644337,
1.38903082001062));
#23917=CARTESIAN_POINT('Ctrl Pts',(-0.160641042350602,0.182142898149225,
1.40014460906743));
#23918=CARTESIAN_POINT('Ctrl Pts',(-0.240151263944613,-0.0361794176709605,
1.41125839812423));
#23919=CARTESIAN_POINT('Ctrl Pts',(-0.0998483101275995,-0.221386302178844,
1.42237218718103));
#23920=CARTESIAN_POINT('Ctrl Pts',(0.131796641356581,-0.203959577192589,
1.43348356382421));
#23921=CARTESIAN_POINT('Ctrl Pts',(0.205808231334455,-0.0679686858761153,
1.44089034411512));
#23922=CARTESIAN_POINT('Ctrl Pts',(0.205812290976358,8.27708256686491E-7,
1.44459252805377));
#23923=CARTESIAN_POINT('Origin',(0.,0.,0.645407471946233));
#23924=CARTESIAN_POINT('',(0.205190393281102,-0.000103909026722956,1.30459252805377));
#23925=CARTESIAN_POINT('',(0.205784930460293,6.78762012092915E-5,1.31040747194623));
#23926=CARTESIAN_POINT('',(0.205475,1.17874941047504E-14,0.645407471946233));
#23927=CARTESIAN_POINT('Ctrl Pts',(0.205784930460293,6.78762012092937E-5,
1.31040747194623));
#23928=CARTESIAN_POINT('Ctrl Pts',(0.205801002271222,0.00380171834571078,
1.31061077563477));
#23929=CARTESIAN_POINT('Ctrl Pts',(0.204016743590097,0.0755578983061786,
1.31451867567558));
#23930=CARTESIAN_POINT('Ctrl Pts',(0.120352309668968,0.210942868533614,
1.32213117206866));
#23931=CARTESIAN_POINT('Ctrl Pts',(-0.111952589707427,0.215518421220722,
1.33324496112546));
#23932=CARTESIAN_POINT('Ctrl Pts',(-0.241786014095534,0.0228275188203595,
1.34435875018226));
#23933=CARTESIAN_POINT('Ctrl Pts',(-0.150309957742793,-0.190757670439842,
1.35547253923907));
#23934=CARTESIAN_POINT('Ctrl Pts',(0.0787465075641072,-0.229740200603712,
1.36658632829588));
#23935=CARTESIAN_POINT('Ctrl Pts',(0.196145957186436,-0.101629499882189,
1.37489797253159));
#23936=CARTESIAN_POINT('Ctrl Pts',(0.205604659733481,-0.0168317924834936,
1.37950502041505));
#23937=CARTESIAN_POINT('Ctrl Pts',(0.205453133831238,-0.000187888241826079,
1.38040747194623));
#23938=CARTESIAN_POINT('Ctrl Pts',(0.205190393281102,-0.000103909026722949,
1.30459252805377));
#23939=CARTESIAN_POINT('Ctrl Pts',(0.205002798510851,0.0408596785255145,
1.30680645090684));
#23940=CARTESIAN_POINT('Ctrl Pts',(0.173264151191812,0.15063609956695,1.31272497011219));
#23941=CARTESIAN_POINT('Ctrl Pts',(-0.00557045627447471,0.242797343170749,
1.3223480856698));
#23942=CARTESIAN_POINT('Ctrl Pts',(-0.207008825709279,0.126999708315969,
1.3334618747266));
#23943=CARTESIAN_POINT('Ctrl Pts',(-0.218969669332857,-0.105042199835232,
1.3445756637834));
#23944=CARTESIAN_POINT('Ctrl Pts',(-0.0305050913306782,-0.240937791217362,
1.35568945284021));
#23945=CARTESIAN_POINT('Ctrl Pts',(0.164305043004325,-0.164739584440547,
1.36569507426366));
#23946=CARTESIAN_POINT('Ctrl Pts',(0.204952496128017,-0.0477747021046654,
1.37199609933485));
#23947=CARTESIAN_POINT('Ctrl Pts',(0.205343844683429,0.000176004178461609,
1.37459252805377));
#23948=CARTESIAN_POINT('Origin',(0.,0.,0.645407471946233));
#23949=CARTESIAN_POINT('',(0.205723053630104,-0.00012021653370823,1.23459252805377));
#23950=CARTESIAN_POINT('',(0.2052527421894,0.000145096082381024,1.24040747194623));
#23951=CARTESIAN_POINT('',(0.205475,1.17874941047504E-14,0.645407471946233));
#23952=CARTESIAN_POINT('Ctrl Pts',(0.2052527421894,0.000145096082381054,
1.24040747194623));
#23953=CARTESIAN_POINT('Ctrl Pts',(0.205410551512377,0.0243477880181972,
1.2417165308545));
#23954=CARTESIAN_POINT('Ctrl Pts',(0.19025975845005,0.116852155262949,1.24673018611503));
#23955=CARTESIAN_POINT('Ctrl Pts',(0.053170711887795,0.236969296798376,
1.25544843772783));
#23956=CARTESIAN_POINT('Ctrl Pts',(-0.170254416296827,0.17319066360285,
1.26656222678464));
#23957=CARTESIAN_POINT('Ctrl Pts',(-0.237843746428552,-0.0491113481040567,
1.27767601584144));
#23958=CARTESIAN_POINT('Ctrl Pts',(-0.0877319981226961,-0.226461185930791,
1.28878980489824));
#23959=CARTESIAN_POINT('Ctrl Pts',(0.138466900336863,-0.197076087766382,
1.29970029026651));
#23960=CARTESIAN_POINT('Ctrl Pts',(0.205508142006035,-0.0642362896597867,
1.3069061792825));
#23961=CARTESIAN_POINT('Ctrl Pts',(0.205784930460293,6.78762012092937E-5,
1.31040747194623));
#23962=CARTESIAN_POINT('Ctrl Pts',(0.205723053630104,-0.000120216533708221,
1.23459252805377));
#23963=CARTESIAN_POINT('Ctrl Pts',(0.205298918797858,0.0608969853087639,
1.23791220612657));
#23964=CARTESIAN_POINT('Ctrl Pts',(0.144198668474879,0.190744063350028,
1.24493648055164));
#23965=CARTESIAN_POINT('Ctrl Pts',(-0.0765564251386213,0.230479269358191,
1.25566535132897));
#23966=CARTESIAN_POINT('Ctrl Pts',(-0.23515855594305,0.0606797610465845,
1.26677914038578));
#23967=CARTESIAN_POINT('Ctrl Pts',(-0.178517393613401,-0.164660620706261,
1.27789292944258));
#23968=CARTESIAN_POINT('Ctrl Pts',(0.0415227636155418,-0.239285268948212,
1.28900671849938));
#23969=CARTESIAN_POINT('Ctrl Pts',(0.187294592944535,-0.123653783093607,
1.29790658470311));
#23970=CARTESIAN_POINT('Ctrl Pts',(0.205316704165066,-0.0276854186132918,
1.30310185455457));
#23971=CARTESIAN_POINT('Ctrl Pts',(0.205190393281102,-0.000103909026722949,
1.30459252805377));
#23972=CARTESIAN_POINT('Origin',(0.,0.,0.645407471946233));
#23973=CARTESIAN_POINT('',(0.205554604385647,0.000179910838621594,1.16459252805377));
#23974=CARTESIAN_POINT('',(0.205260574591088,-0.000148793951100861,1.17040747194623));
#23975=CARTESIAN_POINT('',(0.205475,1.17874941047504E-14,0.645407471946233));
#23976=CARTESIAN_POINT('Ctrl Pts',(0.205260574591088,-0.000148793951100864,
1.17040747194623));
#23977=CARTESIAN_POINT('Ctrl Pts',(0.204961311968991,0.044493502374408,
1.17282228607422));
#23978=CARTESIAN_POINT('Ctrl Pts',(0.168697767785137,0.158064764697474,
1.17894169655448));
#23979=CARTESIAN_POINT('Ctrl Pts',(-0.0186902364010947,0.242140965743205,
1.18876570338701));
#23980=CARTESIAN_POINT('Ctrl Pts',(-0.213572804428157,0.115621059658089,
1.19987949244381));
#23981=CARTESIAN_POINT('Ctrl Pts',(-0.212969762481792,-0.116728113564033,
1.21099328150062));
#23982=CARTESIAN_POINT('Ctrl Pts',(-0.0174330816944656,-0.242234720654174,
1.22210707055742));
#23983=CARTESIAN_POINT('Ctrl Pts',(0.169149144270981,-0.157353841391122,
1.23191180070596));
#23984=CARTESIAN_POINT('Ctrl Pts',(0.204963955993594,-0.0441450839941835,
1.23801193450223));
#23985=CARTESIAN_POINT('Ctrl Pts',(0.2052527421894,0.000145096082381054,
1.24040747194623));
#23986=CARTESIAN_POINT('Ctrl Pts',(0.205554604385647,0.00017991083862162,
1.16459252805377));
#23987=CARTESIAN_POINT('Ctrl Pts',(0.205676289601756,0.0134574818611262,
1.16531336499402));
#23988=CARTESIAN_POINT('Ctrl Pts',(0.198454332603713,0.094840644563722,
1.16973879828655));
#23989=CARTESIAN_POINT('Ctrl Pts',(0.0898833437085198,0.225615966539919,
1.17786882793134));
#23990=CARTESIAN_POINT('Ctrl Pts',(-0.140804956527845,0.197877598659039,
1.18898261698814));
#23991=CARTESIAN_POINT('Ctrl Pts',(-0.242612883217311,-0.0109803793588139,
1.20009640604495));
#23992=CARTESIAN_POINT('Ctrl Pts',(-0.12235448648082,-0.2097878916237,1.21121019510175));
#23993=CARTESIAN_POINT('Ctrl Pts',(0.109896359325859,-0.21657416752884,
1.22232398415856));
#23994=CARTESIAN_POINT('Ctrl Pts',(0.202230669468777,-0.082312541395209,
1.23011809514256));
#23995=CARTESIAN_POINT('Ctrl Pts',(0.20577223226921,-0.00719519062340044,
1.2342076097743));
#23996=CARTESIAN_POINT('Ctrl Pts',(0.205723053630104,-0.000120216533708221,
1.23459252805377));
#23997=CARTESIAN_POINT('Origin',(0.,0.,0.645407471946233));
#23998=CARTESIAN_POINT('',(0.205138522353965,7.81005524626288E-6,1.09459252805377));
#23999=CARTESIAN_POINT('',(0.205789655863746,-6.17368779781373E-5,1.10040747194623));
#24000=CARTESIAN_POINT('',(0.205475,1.17874941047504E-14,0.645407471946233));
#24001=CARTESIAN_POINT('Ctrl Pts',(0.205789655863746,-6.17368779781361E-5,
1.10040747194623));
#24002=CARTESIAN_POINT('Ctrl Pts',(0.205533723504375,0.0645925032691717,
1.10392804129395));
#24003=CARTESIAN_POINT('Ctrl Pts',(0.137841967409279,0.197742342810066,
1.11115320699393));
#24004=CARTESIAN_POINT('Ctrl Pts',(-0.0889063286388705,0.226002736612265,
1.12208296904618));
#24005=CARTESIAN_POINT('Ctrl Pts',(-0.238095468835566,0.0478760895194249,
1.13319675810299));
#24006=CARTESIAN_POINT('Ctrl Pts',(-0.169353126220915,-0.174072085260317,
1.14431054715979));
#24007=CARTESIAN_POINT('Ctrl Pts',(0.0544000534188783,-0.236690106290626,
1.1554243362166));
#24008=CARTESIAN_POINT('Ctrl Pts',(0.190562019135808,-0.116130140045317,
1.16412331114541));
#24009=CARTESIAN_POINT('Ctrl Pts',(0.2054204144752,-0.0239927989965278,
1.16911768972195));
#24010=CARTESIAN_POINT('Ctrl Pts',(0.205260574591088,-0.000148793951100864,
1.17040747194623));
#24011=CARTESIAN_POINT('Ctrl Pts',(0.205138522353965,7.81005524630105E-6,
1.09459252805377));
#24012=CARTESIAN_POINT('Ctrl Pts',(0.205149988139531,0.033826082896543,
1.09641912021375));
#24013=CARTESIAN_POINT('Ctrl Pts',(0.181232693643337,0.1362174972132,1.101950308726));
#24014=CARTESIAN_POINT('Ctrl Pts',(0.019737729131079,0.242057848222183,
1.11118609359052));
#24015=CARTESIAN_POINT('Ctrl Pts',(-0.192661783512051,0.147861479120299,
1.12229988264732));
#24016=CARTESIAN_POINT('Ctrl Pts',(-0.228715780766039,-0.0816741786716276,
1.13341367170413));
#24017=CARTESIAN_POINT('Ctrl Pts',(-0.0554236300753314,-0.236452534483491,
1.14452746076093));
#24018=CARTESIAN_POINT('Ctrl Pts',(0.15406839794226,-0.178801760545413,
1.15492041287748));
#24019=CARTESIAN_POINT('Ctrl Pts',(0.205050912928411,-0.0547799216762583,
1.16160876864176));
#24020=CARTESIAN_POINT('Ctrl Pts',(0.205554604385647,0.00017991083862162,
1.16459252805377));
#24021=CARTESIAN_POINT('Origin',(0.,0.,0.645407471946233));
#24022=CARTESIAN_POINT('',(0.20552593591886,-0.000183965626637278,1.02459252805377));
#24023=CARTESIAN_POINT('',(0.20544247508097,0.000187699708462681,1.03040747194623));
#24024=CARTESIAN_POINT('',(0.205475,1.17874941047504E-14,0.645407471946233));
#24025=CARTESIAN_POINT('Ctrl Pts',(0.20544247508097,0.000187699708462687,
1.03040747194623));
#24026=CARTESIAN_POINT('Ctrl Pts',(0.205596383177594,0.0171893738494543,
1.0313292001614));
#24027=CARTESIAN_POINT('Ctrl Pts',(0.195889593181661,0.102350581389175,
1.03595552472885));
#24028=CARTESIAN_POINT('Ctrl Pts',(0.0775529135379212,0.230145861972334,
1.04428644564855));
#24029=CARTESIAN_POINT('Ctrl Pts',(-0.151298115744515,0.18997487313149,
1.05540023470536));
#24030=CARTESIAN_POINT('Ctrl Pts',(-0.241664263837854,-0.0240822717379046,
1.06651402376216));
#24031=CARTESIAN_POINT('Ctrl Pts',(-0.110832370586897,-0.216096640074974,
1.07762781281897));
#24032=CARTESIAN_POINT('Ctrl Pts',(0.121445648389767,-0.210315303100593,
1.08874160187577));
#24033=CARTESIAN_POINT('Ctrl Pts',(0.204196124007957,-0.074841794914668,
1.09633482158486));
#24034=CARTESIAN_POINT('Ctrl Pts',(0.205803033945758,-0.00344133971228389,
1.10022344494168));
#24035=CARTESIAN_POINT('Ctrl Pts',(0.205789655863746,-6.17368779781361E-5,
1.10040747194623));
#24036=CARTESIAN_POINT('Ctrl Pts',(0.20552593591886,-0.000183965626637285,
1.02459252805377));
#24037=CARTESIAN_POINT('Ctrl Pts',(0.205027284976747,0.0538482597648122,
1.02752487543347));
#24038=CARTESIAN_POINT('Ctrl Pts',(0.155496650182077,0.176951247041673,
1.03416181916545));
#24039=CARTESIAN_POINT('Ctrl Pts',(-0.0521449271278155,0.237197146991165,
1.04450335924969));
#24040=CARTESIAN_POINT('Ctrl Pts',(-0.227563185653378,0.0848326375129703,
1.0556171483065));
#24041=CARTESIAN_POINT('Ctrl Pts',(-0.194690279246867,-0.145180146557101,
1.0667309373633));
#24042=CARTESIAN_POINT('Ctrl Pts',(0.0163848475034698,-0.242307896337387,
1.0778447264201));
#24043=CARTESIAN_POINT('Ctrl Pts',(0.180236614284166,-0.138136714556845,
1.08713192331693));
#24044=CARTESIAN_POINT('Ctrl Pts',(0.205126733847568,-0.0347623261378718,
1.09271452386148));
#24045=CARTESIAN_POINT('Ctrl Pts',(0.205138522353965,7.81005524630105E-6,
1.09459252805377));
#24046=CARTESIAN_POINT('Origin',(0.,0.,0.645407471946233));
#24047=CARTESIAN_POINT('',(0.205743448352251,0.000106566711118361,0.954592528053768));
#24048=CARTESIAN_POINT('',(0.205150677731907,-5.25566492129599E-5,0.960407471946232));
#24049=CARTESIAN_POINT('',(0.205475,1.17874941047504E-14,0.645407471946233));
#24050=CARTESIAN_POINT('Ctrl Pts',(0.205150677731907,-5.25566492129668E-5,
0.960407471946232));
#24051=CARTESIAN_POINT('Ctrl Pts',(0.205064756039612,0.0374795435537448,
0.962434955381129));
#24052=CARTESIAN_POINT('Ctrl Pts',(0.177234439623409,0.143708517228788,
0.968167035168295));
#24053=CARTESIAN_POINT('Ctrl Pts',(0.00662091032790181,0.242770948244842,
0.977603711307729));
#24054=CARTESIAN_POINT('Ctrl Pts',(-0.200374735874429,0.13722805194188,
0.988717500364533));
#24055=CARTESIAN_POINT('Ctrl Pts',(-0.223965113394512,-0.0939212459185429,
0.999831289421336));
#24056=CARTESIAN_POINT('Ctrl Pts',(-0.0425576829655005,-0.239103357370329,
1.01094507847814));
#24057=CARTESIAN_POINT('Ctrl Pts',(0.159527519870246,-0.171541476398135,
1.02113713931977));
#24058=CARTESIAN_POINT('Ctrl Pts',(0.204977798041595,-0.0511435023372491,
1.02762460380914));
#24059=CARTESIAN_POINT('Ctrl Pts',(0.20544247508097,0.000187699708462687,
1.03040747194623));
#24060=CARTESIAN_POINT('Ctrl Pts',(0.205743448352251,0.000106566711118368,
0.954592528053768));
#24061=CARTESIAN_POINT('Ctrl Pts',(0.205782131072789,0.00623496563411944,
0.954926034300931));
#24062=CARTESIAN_POINT('Ctrl Pts',(0.202754080859383,0.0803990246761448,
0.958964136900363));
#24063=CARTESIAN_POINT('Ctrl Pts',(0.112884009708659,0.215032004451281,
0.966706835852063));
#24064=CARTESIAN_POINT('Ctrl Pts',(-0.119438498942156,0.211461649464463,
0.977820624908867));
#24065=CARTESIAN_POINT('Ctrl Pts',(-0.242437629122786,0.0143379927471741,
0.988934413965671));
#24066=CARTESIAN_POINT('Ctrl Pts',(-0.143530830111561,-0.195909362177039,
1.00004820302247));
#24067=CARTESIAN_POINT('Ctrl Pts',(0.086751356142284,-0.226838671363958,
1.01116199207928));
#24068=CARTESIAN_POINT('Ctrl Pts',(0.19782031948766,-0.0967615068704032,
1.01934343375638));
#24069=CARTESIAN_POINT('Ctrl Pts',(0.205657258244577,-0.0144136339232786,
1.02382027908121));
#24070=CARTESIAN_POINT('Ctrl Pts',(0.20552593591886,-0.000183965626637285,
1.02459252805377));
#24071=CARTESIAN_POINT('Origin',(0.,0.,0.645407471946233));
#24072=CARTESIAN_POINT('',(0.205205445749305,0.000116004416325019,0.884592528053768));
#24073=CARTESIAN_POINT('',(0.205635165348036,-0.000160487501855341,0.890407471946233));
#24074=CARTESIAN_POINT('',(0.205475,1.17874941047504E-14,0.645407471946233));
#24075=CARTESIAN_POINT('Ctrl Pts',(0.205635165348036,-0.000160487501855345,
0.890407471946233));
#24076=CARTESIAN_POINT('Ctrl Pts',(0.20514041316225,0.0574941994909011,
0.893540710600855));
#24077=CARTESIAN_POINT('Ctrl Pts',(0.149792439928844,0.184149942781777,
0.900378545607745));
#24078=CARTESIAN_POINT('Ctrl Pts',(-0.0648937601106981,0.234030453531351,
0.910920976966904));
#24079=CARTESIAN_POINT('Ctrl Pts',(-0.231817150854124,0.0724044416546206,
0.922034766023707));
#24080=CARTESIAN_POINT('Ctrl Pts',(-0.186555648217912,-0.155494636948999,
0.933148555080512));
#24081=CARTESIAN_POINT('Ctrl Pts',(0.029462341223335,-0.241067470577576,
0.944262344137316));
#24082=CARTESIAN_POINT('Ctrl Pts',(0.184024675492061,-0.130631009068519,
0.953348649759223));
#24083=CARTESIAN_POINT('Ctrl Pts',(0.205221751249722,-0.031098714158076,
0.958730359028861));
#24084=CARTESIAN_POINT('Ctrl Pts',(0.205150677731907,-5.25566492129668E-5,
0.960407471946232));
#24085=CARTESIAN_POINT('Ctrl Pts',(0.205205445749305,0.000116004416325009,
0.884592528053768));
#24086=CARTESIAN_POINT('Ctrl Pts',(0.205343275267841,0.0267417723340512,
0.886031789520656));
#24087=CARTESIAN_POINT('Ctrl Pts',(0.188156931475396,0.121730614284078,
0.891175647339813));
#24088=CARTESIAN_POINT('Ctrl Pts',(0.0448304764247631,0.238686010114805,
0.900024101511237));
#24089=CARTESIAN_POINT('Ctrl Pts',(-0.176220286722883,0.167116974718297,
0.911137890568042));
#24090=CARTESIAN_POINT('Ctrl Pts',(-0.235976306336092,-0.0574188764093974,
0.922251679624847));
#24091=CARTESIAN_POINT('Ctrl Pts',(-0.0797396575425977,-0.229397140881452,
0.933365468681649));
#24092=CARTESIAN_POINT('Ctrl Pts',(0.142604551604849,-0.192546391773689,
0.944145751491291));
#24093=CARTESIAN_POINT('Ctrl Pts',(0.205352442373934,-0.0618394542260256,
0.951221437948663));
#24094=CARTESIAN_POINT('Ctrl Pts',(0.205743448352251,0.000106566711118368,
0.954592528053768));
#24095=CARTESIAN_POINT('Origin',(0.,0.,0.645407471946233));
#24096=CARTESIAN_POINT('',(0.205269394176581,-0.000252214316689744,0.814592528053768));
#24097=CARTESIAN_POINT('',(0.205654271051376,0.000148184871923512,0.820407471946232));
#24098=CARTESIAN_POINT('',(0.205475,1.17874941047504E-14,0.645407471946233));
#24099=CARTESIAN_POINT('',(0.0530170217188605,-0.198517432567172,0.8));
#24100=CARTESIAN_POINT('Ctrl Pts',(0.0530170217188587,-0.198517432567173,
0.8));
#24101=CARTESIAN_POINT('Ctrl Pts',(0.119028790974553,-0.18088801151799,
0.803704596352268));
#24102=CARTESIAN_POINT('Ctrl Pts',(0.192500600447326,-0.111310459456284,
0.80856877237019));
#24103=CARTESIAN_POINT('Ctrl Pts',(0.205431969941924,-0.0216798251681207,
0.813432948388113));
#24104=CARTESIAN_POINT('Ctrl Pts',(0.205269394176581,-0.000252214316689755,
0.814592528053767));
#24105=CARTESIAN_POINT('',(-0.0531250535940746,-0.19887604744663,0.8));
#24106=CARTESIAN_POINT('Origin',(0.,0.,0.8));
#24107=CARTESIAN_POINT('Ctrl Pts',(-0.053125080564462,-0.198876136975597,
0.8));
#24108=CARTESIAN_POINT('Ctrl Pts',(0.0113386551506616,-0.21601151578625,
0.803632291818556));
#24109=CARTESIAN_POINT('Ctrl Pts',(0.149296237339328,-0.184051126983177,
0.810434782467299));
#24110=CARTESIAN_POINT('Ctrl Pts',(0.205166930984713,-0.0581571994559903,
0.817237273116043));
#24111=CARTESIAN_POINT('Ctrl Pts',(0.205654271051376,0.000148184871923506,
0.820407471946232));
#24112=CARTESIAN_POINT('Origin',(0.,0.,3.1));
#24113=CARTESIAN_POINT('',(-0.126245549239308,1.45328325776573E-5,2.71934196736194));
#24114=CARTESIAN_POINT('',(-0.126374981062586,-0.000161346902988299,2.70565803263806));
#24115=CARTESIAN_POINT('',(-0.12645,1.54856587752183E-17,3.1));
#24116=CARTESIAN_POINT('',(-0.0958116152722464,0.0825211298936403,2.7));
#24117=CARTESIAN_POINT('Ctrl Pts',(-0.126374981062586,-0.000161346902988299,
2.70565803263806));
#24118=CARTESIAN_POINT('Ctrl Pts',(-0.126107573254536,0.0297492098111863,
2.70377202175871));
#24119=CARTESIAN_POINT('Ctrl Pts',(-0.115369380269341,0.0598134784363487,
2.70188601087935));
#24120=CARTESIAN_POINT('Ctrl Pts',(-0.0958116152722464,0.0825211298936403,
2.7));
#24121=CARTESIAN_POINT('',(-0.12645,1.54856587752183E-17,2.7));
#24122=CARTESIAN_POINT('Origin',(0.,0.,2.7));
#24123=CARTESIAN_POINT('',(-0.12645,-1.54856587752183E-17,2.6));
#24124=CARTESIAN_POINT('',(-0.12645,1.54856587752183E-17,3.1));
#24125=CARTESIAN_POINT('Origin',(0.,0.,2.6));
#24126=CARTESIAN_POINT('',(0.095991445127536,0.0826500758460347,2.7));
#24127=CARTESIAN_POINT('Origin',(0.,0.,2.7));
#24128=CARTESIAN_POINT('Ctrl Pts',(0.0959918005672157,0.0826503307119909,
2.7));
#24129=CARTESIAN_POINT('Ctrl Pts',(0.0697118516972522,0.11301027640157,
2.70253749952686));
#24130=CARTESIAN_POINT('Ctrl Pts',(0.0277082938822606,0.129939474688335,
2.70507499905372));
#24131=CARTESIAN_POINT('Ctrl Pts',(-0.0122513412479025,0.126048724837631,
2.70761249858058));
#24132=CARTESIAN_POINT('Ctrl Pts',(-0.0537056163258554,0.122012446376998,
2.71024491008919));
#24133=CARTESIAN_POINT('Ctrl Pts',(-0.092960208469122,0.0955696038330054,
2.7128773215978));
#24134=CARTESIAN_POINT('Ctrl Pts',(-0.1122448026076,0.0586681233168463,
2.71550973310641));
#24135=CARTESIAN_POINT('Ctrl Pts',(-0.121602899042457,0.0407612070094829,
2.71678714452492));
#24136=CARTESIAN_POINT('Ctrl Pts',(-0.126258460357629,0.0203914906379236,
2.71806455594343));
#24137=CARTESIAN_POINT('Ctrl Pts',(-0.126245549239308,1.45328325776573E-5,
2.71934196736194));
#24138=CARTESIAN_POINT('Origin',(0.,0.,3.1));
#24139=CARTESIAN_POINT('',(-0.126511755116174,-0.000105182036976022,2.76934196736194));
#24140=CARTESIAN_POINT('',(-0.12664039552615,3.66938896950461E-5,2.75565803263806));
#24141=CARTESIAN_POINT('',(-0.12645,1.54856587752183E-17,3.1));
#24142=CARTESIAN_POINT('Ctrl Pts',(-0.12664039552615,3.66938896950461E-5,
2.75565803263806));
#24143=CARTESIAN_POINT('Ctrl Pts',(-0.126647890342436,0.00202721792373194,
2.75553223565232));
#24144=CARTESIAN_POINT('Ctrl Pts',(-0.126604975133189,0.00401740611511355,
2.75540643866659));
#24145=CARTESIAN_POINT('Ctrl Pts',(-0.126510633504476,0.00600514734308786,
2.75528064168085));
#24146=CARTESIAN_POINT('Ctrl Pts',(-0.124536452742414,0.0476003640650105,
2.75264823017224));
#24147=CARTESIAN_POINT('Ctrl Pts',(-0.10004305012127,0.0881240748873803,
2.75001581866363));
#24148=CARTESIAN_POINT('Ctrl Pts',(-0.064133889095878,0.109212690295602,
2.74738340715501));
#24149=CARTESIAN_POINT('Ctrl Pts',(-0.0282247280704852,0.130301305703824,
2.7447509956464));
#24150=CARTESIAN_POINT('Ctrl Pts',(0.0191001913591554,0.131954825697897,
2.74211858413779));
#24151=CARTESIAN_POINT('Ctrl Pts',(0.0563882647159258,0.113411365221879,
2.73948617262918));
#24152=CARTESIAN_POINT('Ctrl Pts',(0.0936763380726957,0.0948679047458623,
2.73685376112057));
#24153=CARTESIAN_POINT('Ctrl Pts',(0.120927565356595,0.0561274637997562,
2.73422134961196));
#24154=CARTESIAN_POINT('Ctrl Pts',(0.125787645771127,0.0147753877020813,
2.73158893810334));
#24155=CARTESIAN_POINT('Ctrl Pts',(0.13064772618566,-0.0265766883955932,
2.72895652659473));
#24156=CARTESIAN_POINT('Ctrl Pts',(0.113116659730824,-0.0705403996448371,
2.72632411508612));
#24157=CARTESIAN_POINT('Ctrl Pts',(0.0811433928446468,-0.0972323182667412,
2.72369170357751));
#24158=CARTESIAN_POINT('Ctrl Pts',(0.0491701259584694,-0.123924236888645,
2.7210592920689));
#24159=CARTESIAN_POINT('Ctrl Pts',(0.00275465864095025,-0.133344362883211,
2.71842688056028));
#24160=CARTESIAN_POINT('Ctrl Pts',(-0.0370665720412133,-0.121131225367919,
2.71579446905167));
#24161=CARTESIAN_POINT('Ctrl Pts',(-0.0768878027233769,-0.108918087852628,
2.71316205754306));
#24162=CARTESIAN_POINT('Ctrl Pts',(-0.110114796770184,-0.0750716868274789,
2.71052964603445));
#24163=CARTESIAN_POINT('Ctrl Pts',(-0.121670218183899,-0.0351354691109218,
2.70789723452584));
#24164=CARTESIAN_POINT('Ctrl Pts',(-0.124946671651124,-0.023811852747613,
2.70715083389658));
#24165=CARTESIAN_POINT('Ctrl Pts',(-0.126480809379052,-0.0119986372375087,
2.70640443326732));
#24166=CARTESIAN_POINT('Ctrl Pts',(-0.126374981062586,-0.000161346902988299,
2.70565803263806));
#24167=CARTESIAN_POINT('Ctrl Pts',(-0.126245549239308,1.45328325776573E-5,
2.71934196736194));
#24168=CARTESIAN_POINT('Ctrl Pts',(-0.126231853912779,-0.0216001006849982,
2.72069696745204));
#24169=CARTESIAN_POINT('Ctrl Pts',(-0.120965346567412,-0.0432228820262939,
2.72205196754215));
#24170=CARTESIAN_POINT('Ctrl Pts',(-0.110486681315658,-0.0619230805928583,
2.72340696763225));
#24171=CARTESIAN_POINT('Ctrl Pts',(-0.0901293697515468,-0.0982526854980795,
2.72603937914086));
#24172=CARTESIAN_POINT('Ctrl Pts',(-0.0501001504896328,-0.123551776820195,
2.72867179064947));
#24173=CARTESIAN_POINT('Ctrl Pts',(-0.00855140384117574,-0.126362344661561,
2.73130420215808));
#24174=CARTESIAN_POINT('Ctrl Pts',(0.0329973428072813,-0.129172912502927,
2.7339366136667));
#24175=CARTESIAN_POINT('Ctrl Pts',(0.076065616842282,-0.109494956863544,
2.73656902517531));
#24176=CARTESIAN_POINT('Ctrl Pts',(0.10113334277539,-0.0762433600374486,
2.73920143668392));
#24177=CARTESIAN_POINT('Ctrl Pts',(0.126201068708497,-0.0429917632113539,
2.74183384819253));
#24178=CARTESIAN_POINT('Ctrl Pts',(0.133268246539712,0.00383347480145232,
2.74446625970114));
#24179=CARTESIAN_POINT('Ctrl Pts',(0.119129452671912,0.0430029706396828,
2.74709867120975));
#24180=CARTESIAN_POINT('Ctrl Pts',(0.104990658804112,0.0821724664779139,
2.74973108271837));
#24181=CARTESIAN_POINT('Ctrl Pts',(0.0696458932372969,0.113686220141568,
2.75236349422698));
#24182=CARTESIAN_POINT('Ctrl Pts',(0.0291183743037611,0.123260050517998,
2.75499590573559));
#24183=CARTESIAN_POINT('Ctrl Pts',(-0.0114091446297752,0.132833880894428,
2.7576283172442));
#24184=CARTESIAN_POINT('Ctrl Pts',(-0.0571194169300318,0.120467787983633,
2.76026072875281));
#24185=CARTESIAN_POINT('Ctrl Pts',(-0.0872917850925406,0.0917667415677358,
2.76289314026143));
#24186=CARTESIAN_POINT('Ctrl Pts',(-0.111930332277198,0.0683296655464438,
2.76504274929493));
#24187=CARTESIAN_POINT('Ctrl Pts',(-0.126207827945274,0.0340000461494869,
2.76719235832844));
#24188=CARTESIAN_POINT('Ctrl Pts',(-0.126511755116174,-0.000105182036976022,
2.76934196736194));
#24189=CARTESIAN_POINT('Origin',(0.,0.,3.1));
#24190=CARTESIAN_POINT('',(-0.126553655479795,9.34644642624216E-5,2.81934196736194));
#24191=CARTESIAN_POINT('',(-0.126295222915983,7.47437243418914E-5,2.80565803263806));
#24192=CARTESIAN_POINT('',(-0.12645,1.54856587752183E-17,3.1));
#24193=CARTESIAN_POINT('Ctrl Pts',(-0.126295222915983,7.47437243418914E-5,
2.80565803263806));
#24194=CARTESIAN_POINT('Ctrl Pts',(-0.126381902901803,0.0159778826374278,
2.80466003803733));
#24195=CARTESIAN_POINT('Ctrl Pts',(-0.12359488800886,0.0318517555514631,
2.8036620434366));
#24196=CARTESIAN_POINT('Ctrl Pts',(-0.117794192788123,0.0465350551086,2.80266404883586));
#24197=CARTESIAN_POINT('Ctrl Pts',(-0.102493692318657,0.0852652112740412,
2.80003163732725));
#24198=CARTESIAN_POINT('Ctrl Pts',(-0.0662256093040858,0.115711992156929,
2.79739922581864));
#24199=CARTESIAN_POINT('Ctrl Pts',(-0.0254308011719313,0.124073552736451,
2.79476681431003));
#24200=CARTESIAN_POINT('Ctrl Pts',(0.0153640069602226,0.132435113315973,
2.79213440280142));
#24201=CARTESIAN_POINT('Ctrl Pts',(0.0606855402099605,0.11871145359213,
2.78950199129281));
#24202=CARTESIAN_POINT('Ctrl Pts',(0.089988893871543,0.0891234665506248,
2.78686957978419));
#24203=CARTESIAN_POINT('Ctrl Pts',(0.119292247533126,0.0595354795091193,
2.78423716827558));
#24204=CARTESIAN_POINT('Ctrl Pts',(0.132577421606553,0.0140831651499525,
2.78160475676697));
#24205=CARTESIAN_POINT('Ctrl Pts',(0.123822034418855,-0.0266288104888323,
2.77897234525835));
#24206=CARTESIAN_POINT('Ctrl Pts',(0.115066647231157,-0.067340786127616,
2.77633993374974));
#24207=CARTESIAN_POINT('Ctrl Pts',(0.084270698782333,-0.103312423046018,
2.77370752224113));
#24208=CARTESIAN_POINT('Ctrl Pts',(0.045394477490254,-0.11823815061478,
2.77107511073252));
#24209=CARTESIAN_POINT('Ctrl Pts',(0.00651825619817509,-0.133163878183541,
2.76844269922391));
#24210=CARTESIAN_POINT('Ctrl Pts',(-0.0404382379371578,-0.127043696402664,
2.7658102877153));
#24211=CARTESIAN_POINT('Ctrl Pts',(-0.0741890055533361,-0.102650244201489,
2.76317787620668));
#24212=CARTESIAN_POINT('Ctrl Pts',(-0.106326900403039,-0.0794224998497761,
2.76067126168381));
#24213=CARTESIAN_POINT('Ctrl Pts',(-0.126491054782899,-0.0396262314391609,
2.75816464716093));
#24214=CARTESIAN_POINT('Ctrl Pts',(-0.12664039552615,3.66938896950461E-5,
2.75565803263806));
#24215=CARTESIAN_POINT('Ctrl Pts',(-0.126511755116174,-0.000105182036976022,
2.76934196736194));
#24216=CARTESIAN_POINT('Ctrl Pts',(-0.12658001719922,-0.00776522082814862,
2.76982476983705));
#24217=CARTESIAN_POINT('Ctrl Pts',(-0.125943379547996,-0.015413940155386,
2.77030757231215));
#24218=CARTESIAN_POINT('Ctrl Pts',(-0.124560912333973,-0.022925385115547,
2.77079037478726));
#24219=CARTESIAN_POINT('Ctrl Pts',(-0.117023207388135,-0.0638804654619373,
2.77342278629587));
#24220=CARTESIAN_POINT('Ctrl Pts',(-0.0873133334716985,-0.100754626233721,
2.77605519780449));
#24221=CARTESIAN_POINT('Ctrl Pts',(-0.0488993400374831,-0.116832476461904,
2.7786876093131));
#24222=CARTESIAN_POINT('Ctrl Pts',(-0.0104853466032667,-0.132910326690088,
2.78132002082171));
#24223=CARTESIAN_POINT('Ctrl Pts',(0.0366327663487292,-0.128191866374669,
2.78395243233032));
#24224=CARTESIAN_POINT('Ctrl Pts',(0.0710957359713387,-0.104815935790865,
2.78658484383893));
#24225=CARTESIAN_POINT('Ctrl Pts',(0.105558705593947,-0.0814400052070627,
2.78921725534754));
#24226=CARTESIAN_POINT('Ctrl Pts',(0.12736653188717,-0.0394066043548766,
2.79184966685616));
#24227=CARTESIAN_POINT('Ctrl Pts',(0.126633373335447,0.00222985575585417,
2.79448207836477));
#24228=CARTESIAN_POINT('Ctrl Pts',(0.125900214783723,0.0438663158665862,
2.79711448987338));
#24229=CARTESIAN_POINT('Ctrl Pts',(0.102626071387052,0.0851058352358628,
2.79974690138199));
#24230=CARTESIAN_POINT('Ctrl Pts',(0.067361470922124,0.107253965297467,
2.8023793128906));
#24231=CARTESIAN_POINT('Ctrl Pts',(0.032096870457197,0.12940209535907,2.80501172439922));
#24232=CARTESIAN_POINT('Ctrl Pts',(-0.0151581870759861,0.132458836113002,
2.80764413590783));
#24233=CARTESIAN_POINT('Ctrl Pts',(-0.052982302223486,0.115038507268346,
2.81027654741644));
#24234=CARTESIAN_POINT('Ctrl Pts',(-0.0908064173709864,0.0976181784236899,
2.81290895892505));
#24235=CARTESIAN_POINT('Ctrl Pts',(-0.119199590132803,0.059720779980445,
2.81554137043366));
#24236=CARTESIAN_POINT('Ctrl Pts',(-0.12529077505034,0.0185257648347912,
2.81817378194227));
#24237=CARTESIAN_POINT('Ctrl Pts',(-0.126191803554164,0.0124320600196876,
2.81856317708216));
#24238=CARTESIAN_POINT('Ctrl Pts',(-0.126604835154177,0.00626619900254654,
2.81895257222205));
#24239=CARTESIAN_POINT('Ctrl Pts',(-0.126553655479795,9.34644642624216E-5,
2.81934196736194));
#24240=CARTESIAN_POINT('Origin',(0.,0.,3.1));
#24241=CARTESIAN_POINT('',(-0.126249156657861,1.39511119994357E-5,2.86934196736194));
#24242=CARTESIAN_POINT('',(-0.126382098607383,-0.000107526861324363,2.85565803263806));
#24243=CARTESIAN_POINT('',(-0.12645,1.54856587752183E-17,3.1));
#24244=CARTESIAN_POINT('Ctrl Pts',(-0.126382098607383,-0.000107526861324363,
2.85565803263806));
#24245=CARTESIAN_POINT('Ctrl Pts',(-0.126136963881609,0.0296424659657165,
2.85378784042233));
#24246=CARTESIAN_POINT('Ctrl Pts',(-0.115629819550324,0.0595483512746711,
2.8519176482066));
#24247=CARTESIAN_POINT('Ctrl Pts',(-0.0964566207792818,0.0820798491866498,
2.85004745599088));
#24248=CARTESIAN_POINT('Ctrl Pts',(-0.0694691546368386,0.113794329607957,
2.84741504448226));
#24249=CARTESIAN_POINT('Ctrl Pts',(-0.0253122344935349,0.130898446561428,
2.84478263297365));
#24250=CARTESIAN_POINT('Ctrl Pts',(0.0159971616939493,0.125638656106515,
2.84215022146504));
#24251=CARTESIAN_POINT('Ctrl Pts',(0.0573065578814334,0.120378865651602,
2.83951780995643));
#24252=CARTESIAN_POINT('Ctrl Pts',(0.0957684301130981,0.0927551677883048,
2.83688539844782));
#24253=CARTESIAN_POINT('Ctrl Pts',(0.113947449240963,0.0552897840743664,
2.83425298693921));
#24254=CARTESIAN_POINT('Ctrl Pts',(0.132126468368828,0.017824400360428,
2.83162057543059));
#24255=CARTESIAN_POINT('Ctrl Pts',(0.130022634392893,-0.0294826692041511,
2.82898816392198));
#24256=CARTESIAN_POINT('Ctrl Pts',(0.108589645677727,-0.0651864287383833,
2.82635575241337));
#24257=CARTESIAN_POINT('Ctrl Pts',(0.0871566569625619,-0.100890188272616,
2.82372334090476));
#24258=CARTESIAN_POINT('Ctrl Pts',(0.0463945135081664,-0.124990637776501,
2.82109092939615));
#24259=CARTESIAN_POINT('Ctrl Pts',(0.00478129192095443,-0.126562708640517,
2.81845851788753));
#24260=CARTESIAN_POINT('Ctrl Pts',(-0.036831929666257,-0.128134779504533,
2.81582610637892));
#24261=CARTESIAN_POINT('Ctrl Pts',(-0.0792962293862848,-0.10717847172868,
2.81319369487031));
#24262=CARTESIAN_POINT('Ctrl Pts',(-0.103361920284118,-0.0731935521167569,
2.8105612833617));
#24263=CARTESIAN_POINT('Ctrl Pts',(-0.118303874448411,-0.0520929274442991,
2.80892686645382));
#24264=CARTESIAN_POINT('Ctrl Pts',(-0.126153267003299,-0.0259698452031535,
2.80729244954594));
#24265=CARTESIAN_POINT('Ctrl Pts',(-0.126295222915983,7.47437243418914E-5,
2.80565803263806));
#24266=CARTESIAN_POINT('Ctrl Pts',(-0.126553655479795,9.34644642624216E-5,
2.81934196736194));
#24267=CARTESIAN_POINT('Ctrl Pts',(-0.126258847364269,-0.0354630774409815,
2.82158498373066));
#24268=CARTESIAN_POINT('Ctrl Pts',(-0.110561244917173,-0.0712476866904275,
2.82382800009939));
#24269=CARTESIAN_POINT('Ctrl Pts',(-0.0840069629213228,-0.0947829738698732,
2.82607101646811));
#24270=CARTESIAN_POINT('Ctrl Pts',(-0.0528427688015115,-0.122404065580821,
2.82870342797672));
#24271=CARTESIAN_POINT('Ctrl Pts',(-0.00672518348863185,-0.133153617154654,
2.83133583948533));
#24272=CARTESIAN_POINT('Ctrl Pts',(0.0334400182730099,-0.122158697506542,
2.83396825099395));
#24273=CARTESIAN_POINT('Ctrl Pts',(0.0736052200346521,-0.111163777858429,
2.83660066250256));
#24274=CARTESIAN_POINT('Ctrl Pts',(0.107818038245057,-0.0784243869883676,
2.83923307401117));
#24275=CARTESIAN_POINT('Ctrl Pts',(0.120569301232658,-0.0387817708073496,
2.84186548551978));
#24276=CARTESIAN_POINT('Ctrl Pts',(0.13332056422026,0.000860845373668366,
2.84449789702839));
#24277=CARTESIAN_POINT('Ctrl Pts',(0.124610271985061,0.0474066868656423,
2.847130308537));
#24278=CARTESIAN_POINT('Ctrl Pts',(0.0983869277745218,0.0797558433812344,
2.84976272004562));
#24279=CARTESIAN_POINT('Ctrl Pts',(0.0721635835639831,0.112104999896826,
2.85239513155423));
#24280=CARTESIAN_POINT('Ctrl Pts',(0.0284271873781034,0.130257471436035,
2.85502754306284));
#24281=CARTESIAN_POINT('Ctrl Pts',(-0.0129959127687897,0.125984476806968,
2.85765995457145));
#24282=CARTESIAN_POINT('Ctrl Pts',(-0.0544190129156822,0.121711482177902,
2.86029236608007));
#24283=CARTESIAN_POINT('Ctrl Pts',(-0.0935288170235893,0.0950130213805616,
2.86292477758868));
#24284=CARTESIAN_POINT('Ctrl Pts',(-0.11259627866674,0.0579918974128127,
2.86555718909729));
#24285=CARTESIAN_POINT('Ctrl Pts',(-0.121734428756244,0.0402493895934286,
2.86681878185217));
#24286=CARTESIAN_POINT('Ctrl Pts',(-0.126269172738684,0.0201359308353815,
2.86808037460706));
#24287=CARTESIAN_POINT('Ctrl Pts',(-0.126249156657861,1.39511119994357E-5,
2.86934196736194));
#24288=CARTESIAN_POINT('Origin',(0.,0.,3.1));
#24289=CARTESIAN_POINT('',(-0.126504381589359,-0.000106615302056266,2.91934196736194));
#24290=CARTESIAN_POINT('',(-0.126643227510109,3.12951648517141E-5,2.90565803263806));
#24291=CARTESIAN_POINT('',(-0.12645,1.54856587752183E-17,3.1));
#24292=CARTESIAN_POINT('Ctrl Pts',(-0.126643227510109,3.12951648517141E-5,
2.90565803263806));
#24293=CARTESIAN_POINT('Ctrl Pts',(-0.126649060558016,0.00177143581201147,
2.90554805431595));
#24294=CARTESIAN_POINT('Ctrl Pts',(-0.126616264808321,0.00351135171962892,
2.90543807599384));
#24295=CARTESIAN_POINT('Ctrl Pts',(-0.126544152713349,0.00524963660346066,
2.90532809767173));
#24296=CARTESIAN_POINT('Ctrl Pts',(-0.124818097022822,0.0468567555849086,
2.90269568616312));
#24297=CARTESIAN_POINT('Ctrl Pts',(-0.100566951953931,0.0875294297116145,
2.9000632746545));
#24298=CARTESIAN_POINT('Ctrl Pts',(-0.0647841163292417,0.1088301407863,
2.89743086314589));
#24299=CARTESIAN_POINT('Ctrl Pts',(-0.0290012807045523,0.130130851860986,
2.89479845163728));
#24300=CARTESIAN_POINT('Ctrl Pts',(0.0183132454759347,0.13205959988365,
2.89216604012867));
#24301=CARTESIAN_POINT('Ctrl Pts',(0.0557110953405879,0.113742055209456,
2.88953362862006));
#24302=CARTESIAN_POINT('Ctrl Pts',(0.0931089452052417,0.0954245105352619,
2.88690121711144));
#24303=CARTESIAN_POINT('Ctrl Pts',(0.120590118754061,0.0568606731642085,
2.88426880560283));
#24304=CARTESIAN_POINT('Ctrl Pts',(0.125696998005905,0.0155320946228576,
2.88163639409422));
#24305=CARTESIAN_POINT('Ctrl Pts',(0.130803877257748,-0.025796483918492,
2.87900398258561));
#24306=CARTESIAN_POINT('Ctrl Pts',(0.113536462212617,-0.0698898036301388,
2.87637157107699));
#24307=CARTESIAN_POINT('Ctrl Pts',(0.081722324704119,-0.0967597174754642,
2.87373915956838));
#24308=CARTESIAN_POINT('Ctrl Pts',(0.0499081871956208,-0.12362963132079,
2.87110674805977));
#24309=CARTESIAN_POINT('Ctrl Pts',(0.0035473272237559,-0.133276139299794,
2.86847433655116));
#24310=CARTESIAN_POINT('Ctrl Pts',(-0.0363441991716402,-0.12132633857832,
2.86584192504255));
#24311=CARTESIAN_POINT('Ctrl Pts',(-0.0762357255670363,-0.109376537856846,
2.86320951353394));
#24312=CARTESIAN_POINT('Ctrl Pts',(-0.109657918385963,-0.0758304284348936,
2.86057710202533));
#24313=CARTESIAN_POINT('Ctrl Pts',(-0.121460008724635,-0.035894951779346,
2.85794469051671));
#24314=CARTESIAN_POINT('Ctrl Pts',(-0.124877324339263,-0.0243315656302484,
2.85718247122383));
#24315=CARTESIAN_POINT('Ctrl Pts',(-0.126482006208201,-0.0122324936456281,
2.85642025193094));
#24316=CARTESIAN_POINT('Ctrl Pts',(-0.126382098607383,-0.000107526861324363,
2.85565803263806));
#24317=CARTESIAN_POINT('Ctrl Pts',(-0.126249156657861,1.39511119994357E-5,
2.86934196736194));
#24318=CARTESIAN_POINT('Ctrl Pts',(-0.126227407627626,-0.0218501465218449,
2.87071278611567));
#24319=CARTESIAN_POINT('Ctrl Pts',(-0.120828074559444,-0.0437243044457016,
2.8720836048694));
#24320=CARTESIAN_POINT('Ctrl Pts',(-0.110113563989691,-0.0625778327914941,
2.87345442362312));
#24321=CARTESIAN_POINT('Ctrl Pts',(-0.0895382684910942,-0.0987826518898959,
2.87608683513174));
#24322=CARTESIAN_POINT('Ctrl Pts',(-0.049362558315506,-0.12384850294854,
2.87871924664035));
#24323=CARTESIAN_POINT('Ctrl Pts',(-0.00779867057972899,-0.126412668959158,
2.88135165814896));
#24324=CARTESIAN_POINT('Ctrl Pts',(0.0337652171560469,-0.128976834969775,
2.88398406965757));
#24325=CARTESIAN_POINT('Ctrl Pts',(0.0767172824520115,-0.109039315932365,
2.88661648116618));
#24326=CARTESIAN_POINT('Ctrl Pts',(0.101586725761179,-0.0756380809090063,
2.88924889267479));
#24327=CARTESIAN_POINT('Ctrl Pts',(0.126456169070347,-0.0422368458856463,
2.89188130418341));
#24328=CARTESIAN_POINT('Ctrl Pts',(0.133242990392717,0.00462810512366429,
2.89451371569202));
#24329=CARTESIAN_POINT('Ctrl Pts',(0.118870624347205,0.0437122042621813,
2.89714612720063));
#24330=CARTESIAN_POINT('Ctrl Pts',(0.104498258301693,0.0827963034006972,
2.89977853870924));
#24331=CARTESIAN_POINT('Ctrl Pts',(0.0689667048882996,0.11409955066842,
2.90241095021785));
#24332=CARTESIAN_POINT('Ctrl Pts',(0.0283829370476986,0.123431726145854,
2.90504336172646));
#24333=CARTESIAN_POINT('Ctrl Pts',(-0.0122008307929037,0.132763901623287,
2.90767577323508));
#24334=CARTESIAN_POINT('Ctrl Pts',(-0.0578368130607139,0.120125005310431,
2.91030818474369));
#24335=CARTESIAN_POINT('Ctrl Pts',(-0.0878375513946906,0.0912444338001155,
2.9129405962523));
#24336=CARTESIAN_POINT('Ctrl Pts',(-0.112155666680576,0.0678343076994951,
2.91507438662218));
#24337=CARTESIAN_POINT('Ctrl Pts',(-0.126200703597521,0.0337526498432798,
2.91720817699206));
#24338=CARTESIAN_POINT('Ctrl Pts',(-0.126504381589359,-0.000106615302056266,
2.91934196736194));
#24339=CARTESIAN_POINT('Origin',(0.,0.,3.1));
#24340=CARTESIAN_POINT('',(-0.126560384998288,9.09688539718206E-5,2.96934196736194));
#24341=CARTESIAN_POINT('',(-0.126299886768127,7.7729991388234E-5,2.95565803263806));
#24342=CARTESIAN_POINT('',(-0.12645,1.54856587752183E-17,3.1));
#24343=CARTESIAN_POINT('Ctrl Pts',(-0.126299886768127,7.7729991388234E-5,
2.95565803263806));
#24344=CARTESIAN_POINT('Ctrl Pts',(-0.126388830708229,0.0157273402429332,
2.95467585670095));
#24345=CARTESIAN_POINT('Ctrl Pts',(-0.123692081773928,0.0313473916688532,
2.95369368076385));
#24346=CARTESIAN_POINT('Ctrl Pts',(-0.118069607334697,0.0458317476680533,
2.95271150482674));
#24347=CARTESIAN_POINT('Ctrl Pts',(-0.103000345442256,0.0846524762021514,
2.95007909331813));
#24348=CARTESIAN_POINT('Ctrl Pts',(-0.066914478664464,0.115315070279254,
2.94744668180952));
#24349=CARTESIAN_POINT('Ctrl Pts',(-0.0261702583026162,0.123919727448441,
2.9448142703009));
#24350=CARTESIAN_POINT('Ctrl Pts',(0.0145739620592316,0.132524384617628,
2.94218185879229));
#24351=CARTESIAN_POINT('Ctrl Pts',(0.0599765360051347,0.119071104878899,
2.93954944728368));
#24352=CARTESIAN_POINT('Ctrl Pts',(0.0894558125827043,0.0896584567433833,
2.93691703577507));
#24353=CARTESIAN_POINT('Ctrl Pts',(0.118935089160275,0.0602458086078669,
2.93428462426646));
#24354=CARTESIAN_POINT('Ctrl Pts',(0.13249106836951,0.0148737920755634,
2.93165221275785));
#24355=CARTESIAN_POINT('Ctrl Pts',(0.123978626527973,-0.0258897940256335,
2.92901980124923));
#24356=CARTESIAN_POINT('Ctrl Pts',(0.115466184686436,-0.0666533801268299,
2.92638738974062));
#24357=CARTESIAN_POINT('Ctrl Pts',(0.0848853217941264,-0.10280853579692,
2.92375497823201));
#24358=CARTESIAN_POINT('Ctrl Pts',(0.0460987903596358,-0.117965600062524,
2.9211225667234));
#24359=CARTESIAN_POINT('Ctrl Pts',(0.00731225892514568,-0.133122664328129,
2.91849015521479));
#24360=CARTESIAN_POINT('Ctrl Pts',(-0.0396799410515272,-0.127281637189249,
2.91585774370617));
#24361=CARTESIAN_POINT('Ctrl Pts',(-0.0735755578837821,-0.103090341701714,
2.91322533219756));
#24362=CARTESIAN_POINT('Ctrl Pts',(-0.106055065170122,-0.0799097233361643,
2.91070289901106));
#24363=CARTESIAN_POINT('Ctrl Pts',(-0.126509442293762,-0.0398801022208299,
2.90818046582456));
#24364=CARTESIAN_POINT('Ctrl Pts',(-0.126643227510109,3.12951648517141E-5,
2.90565803263806));
#24365=CARTESIAN_POINT('Ctrl Pts',(-0.126504381589359,-0.000106615302056266,
2.91934196736194));
#24366=CARTESIAN_POINT('Ctrl Pts',(-0.126575344636262,-0.00801880085773389,
2.91984058850067));
#24367=CARTESIAN_POINT('Ctrl Pts',(-0.125895951346516,-0.0159188425067759,
2.9203392096394));
#24368=CARTESIAN_POINT('Ctrl Pts',(-0.124421945835367,-0.0236677318103004,
2.92083783077814));
#24369=CARTESIAN_POINT('Ctrl Pts',(-0.116640107541925,-0.0645770792026294,
2.92347024228675));
#24370=CARTESIAN_POINT('Ctrl Pts',(-0.0867109365548968,-0.101273527279515,
2.92610265379536));
#24371=CARTESIAN_POINT('Ctrl Pts',(-0.0482017639084,-0.117122039303909,
2.92873506530397));
#24372=CARTESIAN_POINT('Ctrl Pts',(-0.0096925912619021,-0.132970551328304,
2.93136747681259));
#24373=CARTESIAN_POINT('Ctrl Pts',(0.0373965830440653,-0.127971127300206,
2.9339998883212));
#24374=CARTESIAN_POINT('Ctrl Pts',(0.071719547440819,-0.104390079267275,
2.93663229982981));
#24375=CARTESIAN_POINT('Ctrl Pts',(0.106042511837572,-0.0808090312343449,
2.93926471133842));
#24376=CARTESIAN_POINT('Ctrl Pts',(0.127599266325111,-0.0386463591965834,
2.94189712284703));
#24377=CARTESIAN_POINT('Ctrl Pts',(0.126617818746111,0.00298498082453686,
2.94452953435564));
#24378=CARTESIAN_POINT('Ctrl Pts',(0.125636371167111,0.0446163208456583,
2.94716194586426));
#24379=CARTESIAN_POINT('Ctrl Pts',(0.10211672152157,0.0857163288501385,
2.94979435737287));
#24380=CARTESIAN_POINT('Ctrl Pts',(0.0667206710566959,0.107653769967896,
2.95242676888148));
#24381=CARTESIAN_POINT('Ctrl Pts',(0.0313246205918224,0.129591211085654,
2.95505918039009));
#24382=CARTESIAN_POINT('Ctrl Pts',(-0.0159478306923833,0.13236608531669,
2.9576915918987));
#24383=CARTESIAN_POINT('Ctrl Pts',(-0.0536673890921198,0.114720501579208,
2.96032400340732));
#24384=CARTESIAN_POINT('Ctrl Pts',(-0.0913869474918552,0.0970749178417258,
2.96295641491593));
#24385=CARTESIAN_POINT('Ctrl Pts',(-0.119553613007122,0.059008876135727,
2.96558882642454));
#24386=CARTESIAN_POINT('Ctrl Pts',(-0.125399024116903,0.0177782700249248,
2.96822123793315));
#24387=CARTESIAN_POINT('Ctrl Pts',(-0.12622857074271,0.0119270630632909,
2.96859481440941));
#24388=CARTESIAN_POINT('Ctrl Pts',(-0.126608575570408,0.00601212294639071,
2.96896839088568));
#24389=CARTESIAN_POINT('Ctrl Pts',(-0.126560384998288,9.09688539718206E-5,
2.96934196736194));
#24390=CARTESIAN_POINT('Origin',(0.,0.,3.1));
#24391=CARTESIAN_POINT('',(-0.126250113253048,1.79623087654263E-5,3.01934196736194));
#24392=CARTESIAN_POINT('',(-0.126375290424941,-0.000106230050797054,3.00565803263806));
#24393=CARTESIAN_POINT('',(-0.12645,1.54856587752183E-17,3.1));
#24394=CARTESIAN_POINT('Ctrl Pts',(-0.126375290424941,-0.000106230050797054,
3.00565803263806));
#24395=CARTESIAN_POINT('Ctrl Pts',(-0.126136144258534,0.0293961593132966,
3.00380365908596));
#24396=CARTESIAN_POINT('Ctrl Pts',(-0.115821844223656,0.0590492800488679,
3.00194928553385));
#24397=CARTESIAN_POINT('Ctrl Pts',(-0.0969443855366137,0.0815031740695626,
3.00009491198175));
#24398=CARTESIAN_POINT('Ctrl Pts',(-0.0701465273355013,0.11337802957871,
2.99746250047314));
#24399=CARTESIAN_POINT('Ctrl Pts',(-0.0260923921578653,0.130745171841498,
2.99483008896453));
#24400=CARTESIAN_POINT('Ctrl Pts',(0.0152476360635642,0.125731821210699,
2.99219767745592));
#24401=CARTESIAN_POINT('Ctrl Pts',(0.0565876642849942,0.120718470579899,
2.98956526594731));
#24402=CARTESIAN_POINT('Ctrl Pts',(0.0952135855502181,0.0933246270555131,
2.98693285443869));
#24403=CARTESIAN_POINT('Ctrl Pts',(0.113615704700958,0.0559683206447137,
2.98430044293008));
#24404=CARTESIAN_POINT('Ctrl Pts',(0.132017823851697,0.0186120142339143,
2.98166803142147));
#24405=CARTESIAN_POINT('Ctrl Pts',(0.130196140887953,-0.0287067550632971,
2.97903561991286));
#24406=CARTESIAN_POINT('Ctrl Pts',(0.108976451346127,-0.0645376969103253,
2.97640320840425));
#24407=CARTESIAN_POINT('Ctrl Pts',(0.0877567618043009,-0.100368638757354,
2.97377079689564));
#24408=CARTESIAN_POINT('Ctrl Pts',(0.0471390656843917,-0.124711753154198,
2.97113838538702));
#24409=CARTESIAN_POINT('Ctrl Pts',(0.00553595882347027,-0.126531950235485,
2.96850597387841));
#24410=CARTESIAN_POINT('Ctrl Pts',(-0.03606714803745,-0.128352147316772,
2.9658735623698));
#24411=CARTESIAN_POINT('Ctrl Pts',(-0.078655665639383,-0.107649427082503,
2.96324115086119));
#24412=CARTESIAN_POINT('Ctrl Pts',(-0.102923595936805,-0.0738086354698221,
2.96060873935258));
#24413=CARTESIAN_POINT('Ctrl Pts',(-0.118136947531953,-0.0525941414955858,
2.95895850378107));
#24414=CARTESIAN_POINT('Ctrl Pts',(-0.126150444648563,-0.0262164832362216,
2.95730826820956));
#24415=CARTESIAN_POINT('Ctrl Pts',(-0.126299886768127,7.7729991388234E-5,
2.95565803263806));
#24416=CARTESIAN_POINT('Ctrl Pts',(-0.126560384998288,9.09688539718206E-5,
2.96934196736194));
#24417=CARTESIAN_POINT('Ctrl Pts',(-0.126269000075926,-0.0357113665330736,
2.97160080239429));
#24418=CARTESIAN_POINT('Ctrl Pts',(-0.110322654377183,-0.0717408868526332,
2.97385963742664));
#24419=CARTESIAN_POINT('Ctrl Pts',(-0.0834402350166293,-0.0952822612815302,
2.97611847245899));
#24420=CARTESIAN_POINT('Ctrl Pts',(-0.0521118781022804,-0.122717015961572,
2.9787508839676));
#24421=CARTESIAN_POINT('Ctrl Pts',(-0.00593100756928766,-0.133191354806051,
2.98138329547621));
#24422=CARTESIAN_POINT('Ctrl Pts',(0.0341679124015605,-0.12195710679034,
2.98401570698482));
#24423=CARTESIAN_POINT('Ctrl Pts',(0.0742668323724097,-0.110722858774629,
2.98664811849343));
#24424=CARTESIAN_POINT('Ctrl Pts',(0.108283801781115,-0.0777800238987277,
2.98928053000205));
#24425=CARTESIAN_POINT('Ctrl Pts',(0.120798430769142,-0.038062071124208,
2.99191294151066));
#24426=CARTESIAN_POINT('Ctrl Pts',(0.133313059757168,0.00165588165031116,
2.99454535301927));
#24427=CARTESIAN_POINT('Ctrl Pts',(0.124325348324518,0.0481489523234473,
2.99717776452788));
#24428=CARTESIAN_POINT('Ctrl Pts',(0.0979095575425482,0.0803411518237943,
2.9998101760365));
#24429=CARTESIAN_POINT('Ctrl Pts',(0.0714937667605778,0.112533351324142,
3.00244258754511));
#24430=CARTESIAN_POINT('Ctrl Pts',(0.0276498966292865,0.130424679651699,
3.00507499905372));
#24431=CARTESIAN_POINT('Ctrl Pts',(-0.0137469851400152,0.125904735947905,
3.00770741056233));
#24432=CARTESIAN_POINT('Ctrl Pts',(-0.0551438669093158,0.121384792244111,
3.01033982207094));
#24433=CARTESIAN_POINT('Ctrl Pts',(-0.0940937603166274,0.0944535765089676,
3.01297223357955));
#24434=CARTESIAN_POINT('Ctrl Pts',(-0.112940108892359,0.0573194028051013,
3.01560464508816));
#24435=CARTESIAN_POINT('Ctrl Pts',(-0.121859038434214,0.039745861833548,
3.01685041917942));
#24436=CARTESIAN_POINT('Ctrl Pts',(-0.126275572181929,0.0198872634041666,
3.01809619327068));
#24437=CARTESIAN_POINT('Ctrl Pts',(-0.126250113253048,1.79623087654263E-5,
3.01934196736194));
#24438=CARTESIAN_POINT('Origin',(0.,0.,3.1));
#24439=CARTESIAN_POINT('',(-0.126496969333234,-0.000107906771987382,3.06934196736194));
#24440=CARTESIAN_POINT('',(-0.126645757366777,2.69067085927681E-5,3.05565803263806));
#24441=CARTESIAN_POINT('',(-0.12645,1.54856587752183E-17,3.1));
#24442=CARTESIAN_POINT('Ctrl Pts',(-0.126645757366777,2.69067085927681E-5,
3.05565803263806));
#24443=CARTESIAN_POINT('Ctrl Pts',(-0.126650109530876,0.00151667558283516,
3.05556387297957));
#24444=CARTESIAN_POINT('Ctrl Pts',(-0.126626072178,0.00300630074643505,
3.05546971332109));
#24445=CARTESIAN_POINT('Ctrl Pts',(-0.126573208557277,0.0044949022237674,
3.0553755536626));
#24446=CARTESIAN_POINT('Ctrl Pts',(-0.125095305962741,0.0461115746257868,
3.05274314215399));
#24447=CARTESIAN_POINT('Ctrl Pts',(-0.10108714199637,0.0869281462553232,
3.05011073064538));
#24448=CARTESIAN_POINT('Ctrl Pts',(-0.0654319685934297,0.108441868097491,
3.04747831913677));
#24449=CARTESIAN_POINT('Ctrl Pts',(-0.0297767951904896,0.129955589939659,
3.04484590762816));
#24450=CARTESIAN_POINT('Ctrl Pts',(0.0175253876490204,0.132166461994459,
3.04221349611954));
#24451=CARTESIAN_POINT('Ctrl Pts',(0.0550318084723819,0.114072263617167,
3.03958108461093));
#24452=CARTESIAN_POINT('Ctrl Pts',(0.092538229295744,0.095978065239874,
3.03694867310232));
#24453=CARTESIAN_POINT('Ctrl Pts',(0.120248888102957,0.0575787964304887,
3.03431626159371));
#24454=CARTESIAN_POINT('Ctrl Pts',(0.125602137884551,0.0162814074734155,
3.0316838500851));
#24455=CARTESIAN_POINT('Ctrl Pts',(0.130955387666146,-0.0250159814836577,
3.02905143857648));
#24456=CARTESIAN_POINT('Ctrl Pts',(0.113951228422121,-0.0692114905884188,
3.02641902706787));
#24457=CARTESIAN_POINT('Ctrl Pts',(0.0822978942873024,-0.0962706490388489,
3.02378661555926));
#24458=CARTESIAN_POINT('Ctrl Pts',(0.0506445601524839,-0.123329807489279,
3.02115420405065));
#24459=CARTESIAN_POINT('Ctrl Pts',(0.00434205112687179,-0.133252615285378,
3.01852179254204));
#24460=CARTESIAN_POINT('Ctrl Pts',(-0.0356200281006283,-0.121540918494949,
3.01588938103343));
#24461=CARTESIAN_POINT('Ctrl Pts',(-0.0755821073281284,-0.10982922170452,
3.01325696952481));
#24462=CARTESIAN_POINT('Ctrl Pts',(-0.109203756757516,-0.0764830203275614,
3.0106245580162));
#24463=CARTESIAN_POINT('Ctrl Pts',(-0.121243790859916,-0.0366186352613279,
3.00799214650759));
#24464=CARTESIAN_POINT('Ctrl Pts',(-0.124802354366684,-0.0248362810993748,
3.00721410855108));
#24465=CARTESIAN_POINT('Ctrl Pts',(-0.126475628781476,-0.012484522820876,
3.00643607059457));
#24466=CARTESIAN_POINT('Ctrl Pts',(-0.126375290424941,-0.000106230050797054,
3.00565803263806));
#24467=CARTESIAN_POINT('Ctrl Pts',(-0.126250113253048,1.79623087654263E-5,
3.01934196736194));
#24468=CARTESIAN_POINT('Ctrl Pts',(-0.126221775608494,-0.0220980188702133,
3.0207286047793));
#24469=CARTESIAN_POINT('Ctrl Pts',(-0.120690113995694,-0.0442272599176159,
3.02211524219665));
#24470=CARTESIAN_POINT('Ctrl Pts',(-0.109738425578795,-0.063233377942656,
3.023501879614));
#24471=CARTESIAN_POINT('Ctrl Pts',(-0.0889475899453455,-0.0993148533139586,
3.02613429112261));
#24472=CARTESIAN_POINT('Ctrl Pts',(-0.0486231149342947,-0.124140672383972,
3.02876670263122));
#24473=CARTESIAN_POINT('Ctrl Pts',(-0.00704467496461261,-0.126456928197685,
3.03139911413984));
#24474=CARTESIAN_POINT('Ctrl Pts',(0.0345337650050683,-0.128773184011397,
3.03403152564845));
#24475=CARTESIAN_POINT('Ctrl Pts',(0.0773661699333803,-0.108579876568808,
3.03666393715706));
#24476=CARTESIAN_POINT('Ctrl Pts',(0.102035984081992,-0.0750309275363891,
3.03929634866567));
#24477=CARTESIAN_POINT('Ctrl Pts',(0.126705798230605,-0.0414819785039689,
3.04192876017428));
#24478=CARTESIAN_POINT('Ctrl Pts',(0.133213021599516,0.00542261211828284,
3.0445611716829));
#24479=CARTESIAN_POINT('Ctrl Pts',(0.118607834643087,0.0444203072460051,
3.04719358319151));
#24480=CARTESIAN_POINT('Ctrl Pts',(0.104002647686659,0.0834180023737263,
3.04982599470012));
#24481=CARTESIAN_POINT('Ctrl Pts',(0.0682850504048921,0.114508802006919,
3.05245840620873));
#24482=CARTESIAN_POINT('Ctrl Pts',(0.0276463521492325,0.123598791852477,
3.05509081771734));
#24483=CARTESIAN_POINT('Ctrl Pts',(-0.0129923461064282,0.132688781698037,
3.05772322922596));
#24484=CARTESIAN_POINT('Ctrl Pts',(-0.0585521453359818,0.119777961755961,
3.06035564073457));
#24485=CARTESIAN_POINT('Ctrl Pts',(-0.0883801220659878,0.0907189955750862,
3.06298805224318));
#24486=CARTESIAN_POINT('Ctrl Pts',(-0.112378957568068,0.0673388865067503,
3.06510602394943));
#24487=CARTESIAN_POINT('Ctrl Pts',(-0.126193947985427,0.0335054291562246,
3.06722399565569));
#24488=CARTESIAN_POINT('Ctrl Pts',(-0.126496969333234,-0.000107906771987382,
3.06934196736194));
#24489=CARTESIAN_POINT('Origin',(0.,0.,3.1));
#24490=CARTESIAN_POINT('',(-0.126566979141993,8.83287276302464E-5,3.11934196736194));
#24491=CARTESIAN_POINT('',(-0.126304742691185,8.06358209441624E-5,3.10565803263806));
#24492=CARTESIAN_POINT('',(-0.12645,1.54856587752183E-17,3.1));
#24493=CARTESIAN_POINT('Ctrl Pts',(-0.126304742691185,8.06358209441624E-5,
3.10565803263806));
#24494=CARTESIAN_POINT('Ctrl Pts',(-0.12639574781383,0.0154767095828029,
3.10469167536458));
#24495=CARTESIAN_POINT('Ctrl Pts',(-0.123787659959305,0.0308430184790688,
3.1037253180911));
#24496=CARTESIAN_POINT('Ctrl Pts',(-0.118340823679398,0.0451268292855474,
3.10275896081762));
#24497=CARTESIAN_POINT('Ctrl Pts',(-0.103503335617549,0.0840367324711176,
3.10012654930901));
#24498=CARTESIAN_POINT('Ctrl Pts',(-0.0676009656676162,0.114913977953889,
3.09749413780039));
#24499=CARTESIAN_POINT('Ctrl Pts',(-0.0269087833345171,0.123761458661173,
3.09486172629178));
#24500=CARTESIAN_POINT('Ctrl Pts',(0.0137833989985814,0.132608939368457,
3.09222931478317));
#24501=CARTESIAN_POINT('Ctrl Pts',(0.0592653937148459,0.119426655300253,
3.08959690327456));
#24502=CARTESIAN_POINT('Ctrl Pts',(0.0889195472648929,0.0901903286649502,
3.08696449176595));
#24503=CARTESIAN_POINT('Ctrl Pts',(0.11857370081494,0.0609540020296468,
3.08433208025733));
#24504=CARTESIAN_POINT('Ctrl Pts',(0.13240001319877,0.015663632827244,3.08169966874872));
#24505=CARTESIAN_POINT('Ctrl Pts',(0.124130814751194,-0.0251499920415489,
3.07906725724011));
#24506=CARTESIAN_POINT('Ctrl Pts',(0.115861616303618,-0.0659636169103418,
3.0764348457315));
#24507=CARTESIAN_POINT('Ctrl Pts',(0.085496907024637,-0.102300497445525,
3.07380243422289));
#24508=CARTESIAN_POINT('Ctrl Pts',(0.0468014538280004,-0.117688594137541,
3.07117002271428));
#24509=CARTESIAN_POINT('Ctrl Pts',(0.0081060006313637,-0.133076690829557,
3.06853761120566));
#24510=CARTESIAN_POINT('Ctrl Pts',(-0.0389201964829282,-0.127516003678407,
3.06590519969705));
#24511=CARTESIAN_POINT('Ctrl Pts',(-0.0729594744287227,-0.103527273515581,
3.06327278818844));
#24512=CARTESIAN_POINT('Ctrl Pts',(-0.105781189400045,-0.0803966047281269,
3.06073453633831));
#24513=CARTESIAN_POINT('Ctrl Pts',(-0.12652843654431,-0.0401326336098284,
3.05819628448819));
#24514=CARTESIAN_POINT('Ctrl Pts',(-0.126645757366777,2.69067085927681E-5,
3.05565803263806));
#24515=CARTESIAN_POINT('Ctrl Pts',(-0.126496969333234,-0.000107906771987382,
3.06934196736194));
#24516=CARTESIAN_POINT('Ctrl Pts',(-0.126570570997419,-0.00827233967750279,
3.0698564071643));
#24517=CARTESIAN_POINT('Ctrl Pts',(-0.125847009061939,-0.0164237861126916,
3.07037084696666));
#24518=CARTESIAN_POINT('Ctrl Pts',(-0.124278591835651,-0.0244092963007763,
3.07088528676901));
#24519=CARTESIAN_POINT('Ctrl Pts',(-0.116252930644851,-0.0652715095760922,
3.07351769827763));
#24520=CARTESIAN_POINT('Ctrl Pts',(-0.0861054540327919,-0.101788823707051,
3.07615010978624));
#24521=CARTESIAN_POINT('Ctrl Pts',(-0.0475024541674668,-0.117407405995615,
3.07878252129485));
#24522=CARTESIAN_POINT('Ctrl Pts',(-0.00889945430214065,-0.133025988284179,
3.08141493280346));
#24523=CARTESIAN_POINT('Ctrl Pts',(0.0381590688164514,-0.127745838730347,
3.08404734431207));
#24524=CARTESIAN_POINT('Ctrl Pts',(0.072340798251519,-0.103960526368831,
3.08667975582068));
#24525=CARTESIAN_POINT('Ctrl Pts',(0.106522527686585,-0.0801752140073166,
3.0893121673293));
#24526=CARTESIAN_POINT('Ctrl Pts',(0.127827463438127,-0.0378847388381192,
3.09194457883791));
#24527=CARTESIAN_POINT('Ctrl Pts',(0.1265977664655,0.00374000808798695,
3.09457699034652));
#24528=CARTESIAN_POINT('Ctrl Pts',(0.125368069492872,0.0453647550140949,
3.09720940185513));
#24529=CARTESIAN_POINT('Ctrl Pts',(0.101603739796073,0.0863237736971122,
3.09984181336374));
#24530=CARTESIAN_POINT('Ctrl Pts',(0.066077495668981,0.108049741788989,
3.10247422487236));
#24531=CARTESIAN_POINT('Ctrl Pts',(0.0305512515418895,0.129775709880865,
3.10510663638097));
#24532=CARTESIAN_POINT('Ctrl Pts',(-0.0167369070154944,0.132268627381602,
3.10773904788958));
#24533=CARTESIAN_POINT('Ctrl Pts',(-0.0543505659626984,0.114398418319861,
3.11037145939819));
#24534=CARTESIAN_POINT('Ctrl Pts',(-0.0919642249099026,0.096528209258119,
3.1130038709068));
#24535=CARTESIAN_POINT('Ctrl Pts',(-0.119903384246927,0.0582948736338987,
3.11563628241541));
#24536=CARTESIAN_POINT('Ctrl Pts',(-0.125502814331461,0.0170301417913753,
3.11826869392403));
#24537=CARTESIAN_POINT('Ctrl Pts',(-0.126263804720884,0.011422059561536,
3.11862645173666));
#24538=CARTESIAN_POINT('Ctrl Pts',(-0.126612176704445,0.00575798695415024,
3.1189842095493));
#24539=CARTESIAN_POINT('Ctrl Pts',(-0.126566979141993,8.83287276302464E-5,
3.11934196736194));
#24540=CARTESIAN_POINT('Origin',(0.,0.,3.1));
#24541=CARTESIAN_POINT('',(-0.126251310180948,2.19509288584552E-5,3.16934196736194));
#24542=CARTESIAN_POINT('',(-0.126368593930883,-0.000104790611567188,3.15565803263806));
#24543=CARTESIAN_POINT('',(-0.12645,1.54856587752183E-17,3.1));
#24544=CARTESIAN_POINT('Ctrl Pts',(-0.126368593930883,-0.000104790611567188,
3.15565803263806));
#24545=CARTESIAN_POINT('Ctrl Pts',(-0.126135626550864,0.029149858613393,
3.15381947774958));
#24546=CARTESIAN_POINT('Ctrl Pts',(-0.116012034435359,0.0585500300902377,
3.15198092286111));
#24547=CARTESIAN_POINT('Ctrl Pts',(-0.0974287026581059,0.0809236008148654,
3.15014236797263));
#24548=CARTESIAN_POINT('Ctrl Pts',(-0.0708214054023045,0.112957697503196,
3.14750995646402));
#24549=CARTESIAN_POINT('Ctrl Pts',(-0.0268716218413343,0.130587246038798,
3.1448775449554));
#24550=CARTESIAN_POINT('Ctrl Pts',(0.014497568206441,0.125820514172312,
3.14224513344679));
#24551=CARTESIAN_POINT('Ctrl Pts',(0.0558667582542159,0.121053782305825,
3.13961272193818));
#24552=CARTESIAN_POINT('Ctrl Pts',(0.0946553547887964,0.0938907700372525,
3.13698031042957));
#24553=CARTESIAN_POINT('Ctrl Pts',(0.113279919572572,0.0566448681887155,
3.13434789892096));
#24554=CARTESIAN_POINT('Ctrl Pts',(0.131904484356347,0.0193989663401779,
3.13171548741235));
#24555=CARTESIAN_POINT('Ctrl Pts',(0.130365017389317,-0.0279298250883239,
3.12908307590374));
#24556=CARTESIAN_POINT('Ctrl Pts',(0.109359381568105,-0.0638866725814309,
3.12645066439512));
#24557=CARTESIAN_POINT('Ctrl Pts',(0.0883537457468925,-0.0998435200745383,
3.12381825288651));
#24558=CARTESIAN_POINT('Ctrl Pts',(0.0478819410714995,-0.12442842363225,
3.1211858413779));
#24559=CARTESIAN_POINT('Ctrl Pts',(0.00629042865298903,-0.126496686825572,
3.11855342986929));
#24560=CARTESIAN_POINT('Ctrl Pts',(-0.0353010837655206,-0.128564950018895,
3.11592101836068));
#24561=CARTESIAN_POINT('Ctrl Pts',(-0.0780123039271484,-0.108116572847827,
3.11328860685206));
#24562=CARTESIAN_POINT('Ctrl Pts',(-0.102481610921079,-0.0744211038181091,
3.11065619534345));
#24563=CARTESIAN_POINT('Ctrl Pts',(-0.117968244532349,-0.0530952287799418,
3.10899014110832));
#24564=CARTESIAN_POINT('Ctrl Pts',(-0.12614784474654,-0.0264630603867145,
3.10732408687319));
#24565=CARTESIAN_POINT('Ctrl Pts',(-0.126304742691185,8.06358209441624E-5,
3.10565803263806));
#24566=CARTESIAN_POINT('Ctrl Pts',(-0.126566979141993,8.83287276302464E-5,
3.11934196736194));
#24567=CARTESIAN_POINT('Ctrl Pts',(-0.126279609310085,-0.0359598261533815,
3.12161662105791));
#24568=CARTESIAN_POINT('Ctrl Pts',(-0.110082106605306,-0.0722337808796859,
3.12389127475389));
#24569=CARTESIAN_POINT('Ctrl Pts',(-0.0828705393299942,-0.0957781595443726,
3.12616592844986));
#24570=CARTESIAN_POINT('Ctrl Pts',(-0.0513791334119502,-0.12302560097677,
3.12879833995848));
#24571=CARTESIAN_POINT('Ctrl Pts',(-0.00513662074381884,-0.133224355780737,
3.13143075146709));
#24572=CARTESIAN_POINT('Ctrl Pts',(0.034894591212013,-0.121751179208655,
3.1340631629757));
#24573=CARTESIAN_POINT('Ctrl Pts',(0.0749258031678458,-0.110278002636571,
3.13669557448431));
#24574=CARTESIAN_POINT('Ctrl Pts',(0.108745714411378,-0.0771328946884361,
3.13932798599292));
#24575=CARTESIAN_POINT('Ctrl Pts',(0.12102326443306,-0.0373410176684702,
3.14196039750153));
#24576=CARTESIAN_POINT('Ctrl Pts',(0.133300814454742,0.00245085935149471,
3.14459280901015));
#24577=CARTESIAN_POINT('Ctrl Pts',(0.124036003254574,0.0488895054432904,
3.14722522051876));
#24578=CARTESIAN_POINT('Ctrl Pts',(0.097428705282154,0.0809236029943958,
3.14985763202737));
#24579=CARTESIAN_POINT('Ctrl Pts',(0.0708214073097326,0.112957700545502,
3.15249004353598));
#24580=CARTESIAN_POINT('Ctrl Pts',(0.0268716225650577,0.130587249555918,
3.15512245504459));
#24581=CARTESIAN_POINT('Ctrl Pts',(-0.0144975685969178,0.125820517561044,
3.15775486655321));
#24582=CARTESIAN_POINT('Ctrl Pts',(-0.0558667597588919,0.121053785566171,
3.16038727806182));
#24583=CARTESIAN_POINT('Ctrl Pts',(-0.0946553573381664,0.0938907725660106,
3.16301968957043));
#24584=CARTESIAN_POINT('Ctrl Pts',(-0.113279922623555,0.0566448697143249,
3.16565210107904));
#24585=CARTESIAN_POINT('Ctrl Pts',(-0.121981975887314,0.039242271290916,
3.16688205650667));
#24586=CARTESIAN_POINT('Ctrl Pts',(-0.126282044039751,0.0196384895744722,
3.16811201193431));
#24587=CARTESIAN_POINT('Ctrl Pts',(-0.126251310180948,2.19509288584552E-5,
3.16934196736194));
#24588=CARTESIAN_POINT('Origin',(0.,0.,3.1));
#24589=CARTESIAN_POINT('',(-0.126489518850073,-0.000109039769437509,3.21934196736194));
#24590=CARTESIAN_POINT('',(-0.126647930997008,2.24668189870201E-5,3.20565803263806));
#24591=CARTESIAN_POINT('',(-0.12645,1.54856587752183E-17,3.1));
#24592=CARTESIAN_POINT('Ctrl Pts',(-0.126647930997008,2.24668189870201E-5,
3.20565803263806));
#24593=CARTESIAN_POINT('Ctrl Pts',(-0.126650996831423,0.00126189995630808,
3.2055796916432));
#24594=CARTESIAN_POINT('Ctrl Pts',(-0.126634359036856,0.00250124877863209,
3.20550135064834));
#24595=CARTESIAN_POINT('Ctrl Pts',(-0.126597763055832,0.00374000798724603,
3.20542300965348));
#24596=CARTESIAN_POINT('Ctrl Pts',(-0.125368066116328,0.0453647537922705,
3.20279059814487));
#24597=CARTESIAN_POINT('Ctrl Pts',(-0.10160373705958,0.0863237713721372,
3.20015818663626));
#24598=CARTESIAN_POINT('Ctrl Pts',(-0.0660774938893213,0.10804973887887,
3.19752577512764));
#24599=CARTESIAN_POINT('Ctrl Pts',(-0.0305512507190632,0.129775706385603,
3.19489336361903));
#24600=CARTESIAN_POINT('Ctrl Pts',(0.0167369065647044,0.132268623819202,
3.19226095211042));
#24601=CARTESIAN_POINT('Ctrl Pts',(0.0543505644988585,0.114398415238764,
3.18962854060181));
#24602=CARTESIAN_POINT('Ctrl Pts',(0.091964222433013,0.0965282066583261,
3.1869961290932));
#24603=CARTESIAN_POINT('Ctrl Pts',(0.119903381017553,0.0582948720638503,
3.18436371758459));
#24604=CARTESIAN_POINT('Ctrl Pts',(0.125502810951281,0.0170301413327138,
3.18173130607597));
#24605=CARTESIAN_POINT('Ctrl Pts',(0.13110224088501,-0.0242345893984227,
3.17909889456736));
#24606=CARTESIAN_POINT('Ctrl Pts',(0.114361942167926,-0.0685307162662204,
3.17646648305875));
#24607=CARTESIAN_POINT('Ctrl Pts',(0.0828705370980449,-0.0957781569647633,
3.17383407155014));
#24608=CARTESIAN_POINT('Ctrl Pts',(0.0513791320281642,-0.123025597663306,
3.17120166004152));
#24609=CARTESIAN_POINT('Ctrl Pts',(0.00513662060548718,-0.133224352192594,
3.16856924853291));
#24610=CARTESIAN_POINT('Ctrl Pts',(-0.0348945902721819,-0.121751175929524,
3.1659368370243));
#24611=CARTESIAN_POINT('Ctrl Pts',(-0.0749258011498519,-0.110277999666453,
3.16330442551569));
#24612=CARTESIAN_POINT('Ctrl Pts',(-0.108745711482513,-0.0771328926110206,
3.16067201400708));
#24613=CARTESIAN_POINT('Ctrl Pts',(-0.121023261173527,-0.0373410166627737,
3.15803960249846));
#24614=CARTESIAN_POINT('Ctrl Pts',(-0.124725803146683,-0.0253409763781187,
3.15724574587833));
#24615=CARTESIAN_POINT('Ctrl Pts',(-0.126469185269255,-0.0127364488245176,
3.15645188925819));
#24616=CARTESIAN_POINT('Ctrl Pts',(-0.126368593930883,-0.000104790611567188,
3.15565803263806));
#24617=CARTESIAN_POINT('Ctrl Pts',(-0.126251310180948,2.19509288584552E-5,
3.16934196736194));
#24618=CARTESIAN_POINT('Ctrl Pts',(-0.126216265913324,-0.0223457977660937,
3.17074442344292));
#24619=CARTESIAN_POINT('Ctrl Pts',(-0.120550447304899,-0.0447301326243598,
3.1721468795239));
#24620=CARTESIAN_POINT('Ctrl Pts',(-0.109359384513483,-0.0638866743021069,
3.17354933560488));
#24621=CARTESIAN_POINT('Ctrl Pts',(-0.0883537481265213,-0.0998435227636405,
3.17618174711349));
#24622=CARTESIAN_POINT('Ctrl Pts',(-0.0478819423610949,-0.124428426983496,
3.1788141586221));
#24623=CARTESIAN_POINT('Ctrl Pts',(-0.00629042882239688,-0.126496690232519,
3.18144657013071));
#24624=CARTESIAN_POINT('Ctrl Pts',(0.0353010847163008,-0.128564953481541,
3.18407898163933));
#24625=CARTESIAN_POINT('Ctrl Pts',(0.0780123060282702,-0.108116575759732,
3.18671139314794));
#24626=CARTESIAN_POINT('Ctrl Pts',(0.102481613681232,-0.0744211058224891,
3.18934380465655));
#24627=CARTESIAN_POINT('Ctrl Pts',(0.126950921334194,-0.040725635885246,
3.19197621616516));
#24628=CARTESIAN_POINT('Ctrl Pts',(0.133178315328148,0.00621692626743081,
3.19460862767377));
#24629=CARTESIAN_POINT('Ctrl Pts',(0.118340826866677,0.0451268305009631,
3.19724103918239));
#24630=CARTESIAN_POINT('Ctrl Pts',(0.103503338405205,0.0840367347344954,
3.199873450691));
#24631=CARTESIAN_POINT('Ctrl Pts',(0.0676009674883078,0.114913981048883,
3.20250586219961));
#24632=CARTESIAN_POINT('Ctrl Pts',(0.026908784059242,0.123761461994453,
3.20513827370822));
#24633=CARTESIAN_POINT('Ctrl Pts',(-0.0137833993698235,0.132608942940023,
3.20777068521683));
#24634=CARTESIAN_POINT('Ctrl Pts',(-0.0592653953110574,0.119426658516775,
3.21040309672544));
#24635=CARTESIAN_POINT('Ctrl Pts',(-0.0889195496597795,0.0901903310940448,
3.21303550823405));
#24636=CARTESIAN_POINT('Ctrl Pts',(-0.11260033459284,0.0668432083338218,
3.21513766127668));
#24637=CARTESIAN_POINT('Ctrl Pts',(-0.126187596109782,0.0332583119648893,
3.21723981431931));
#24638=CARTESIAN_POINT('Ctrl Pts',(-0.126489518850073,-0.000109039769437509,
3.21934196736194));
#24639=CARTESIAN_POINT('Origin',(0.,0.,3.1));
#24640=CARTESIAN_POINT('',(-0.126573425356775,8.55484528903966E-5,3.26934196736194));
#24641=CARTESIAN_POINT('',(-0.126309785017077,8.34376343069358E-5,3.25565803263806));
#24642=CARTESIAN_POINT('',(-0.12645,1.54856587752183E-17,3.1));
#24643=CARTESIAN_POINT('Ctrl Pts',(-0.126309785017077,8.34376343069358E-5,
3.25565803263806));
#24644=CARTESIAN_POINT('Ctrl Pts',(-0.126402648710969,0.0152259667938181,
3.2547074940282));
#24645=CARTESIAN_POINT('Ctrl Pts',(-0.123881624579711,0.0303386118332616,
3.25375695541835));
#24646=CARTESIAN_POINT('Ctrl Pts',(-0.118607831448617,0.0444203060496175,
3.25280641680849));
#24647=CARTESIAN_POINT('Ctrl Pts',(-0.104002644885555,0.0834180001270126,
3.25017400529988));
#24648=CARTESIAN_POINT('Ctrl Pts',(-0.0682850485657758,0.114508798922838,
3.24754159379127));
#24649=CARTESIAN_POINT('Ctrl Pts',(-0.0276463514046418,0.123598788523579,
3.24490918228266));
#24650=CARTESIAN_POINT('Ctrl Pts',(0.0129923457564923,0.13268877812432,
3.24227677077404));
#24651=CARTESIAN_POINT('Ctrl Pts',(0.0585521437589804,0.119777958529977,
3.23964435926544));
#24652=CARTESIAN_POINT('Ctrl Pts',(0.0883801196856296,0.090718993131753,
3.23701194775682));
#24653=CARTESIAN_POINT('Ctrl Pts',(0.118208095612278,0.0616600277335293,
3.23437953624821));
#24654=CARTESIAN_POINT('Ctrl Pts',(0.132304249463088,0.0164529165314243,
3.2317471247396));
#24655=CARTESIAN_POINT('Ctrl Pts',(0.124278588488448,-0.024409295643347,
3.22911471323098));
#24656=CARTESIAN_POINT('Ctrl Pts',(0.116252927513807,-0.0652715078181186,
3.22648230172237));
#24657=CARTESIAN_POINT('Ctrl Pts',(0.0861054517137156,-0.101788820965557,
3.22384989021376));
#24658=CARTESIAN_POINT('Ctrl Pts',(0.0475024528880895,-0.117407402833467,
3.22121747870515));
#24659=CARTESIAN_POINT('Ctrl Pts',(0.00889945406246312,-0.133025984701378,
3.21858506719654));
#24660=CARTESIAN_POINT('Ctrl Pts',(-0.0381590677886978,-0.127745835289761,
3.21595265568793));
#24661=CARTESIAN_POINT('Ctrl Pts',(-0.0723407963031478,-0.103960523568861,
3.21332024417931));
#24662=CARTESIAN_POINT('Ctrl Pts',(-0.105505271014729,-0.0808830665952798,
3.21076617366556));
#24663=CARTESIAN_POINT('Ctrl Pts',(-0.126547978765194,-0.0403854911787608,
3.20821210315181));
#24664=CARTESIAN_POINT('Ctrl Pts',(-0.126647930997008,2.24668189870201E-5,
3.20565803263806));
#24665=CARTESIAN_POINT('Ctrl Pts',(-0.126489518850073,-0.000109039769437509,
3.21934196736194));
#24666=CARTESIAN_POINT('Ctrl Pts',(-0.126565677476903,-0.00852580124482262,
3.21987222582793));
#24667=CARTESIAN_POINT('Ctrl Pts',(-0.125796519899578,-0.0169287208447501,
3.22040248429391));
#24668=CARTESIAN_POINT('Ctrl Pts',(-0.124130818094417,-0.0251499927189283,
3.22093274275989));
#24669=CARTESIAN_POINT('Ctrl Pts',(-0.115861619424122,-0.065963618686957,
3.2235651542685));
#24670=CARTESIAN_POINT('Ctrl Pts',(-0.0854969093273219,-0.102300500200801,
3.22619756577711));
#24671=CARTESIAN_POINT('Ctrl Pts',(-0.0468014550884958,-0.117688597307262,
3.22882997728573));
#24672=CARTESIAN_POINT('Ctrl Pts',(-0.00810600084966979,-0.133076694413723,
3.23146238879434));
#24673=CARTESIAN_POINT('Ctrl Pts',(0.038920197531182,-0.127516007112802,
3.23409480030295));
#24674=CARTESIAN_POINT('Ctrl Pts',(0.0729594763937567,-0.103527276303882,
3.23672721181156));
#24675=CARTESIAN_POINT('Ctrl Pts',(0.106998755256331,-0.0795385454949616,
3.23935962332018));
#24676=CARTESIAN_POINT('Ctrl Pts',(0.128051114600629,-0.0371217711780427,
3.24199203482878));
#24677=CARTESIAN_POINT('Ctrl Pts',(0.126573211966284,0.00449490234484176,
3.2446244463374));
#24678=CARTESIAN_POINT('Ctrl Pts',(0.125095309331938,0.0461115758677259,
3.24725685784601));
#24679=CARTESIAN_POINT('Ctrl Pts',(0.10108714471895,0.0869281485965757,
3.24988926935462));
#24680=CARTESIAN_POINT('Ctrl Pts',(0.0654319703557041,0.108441871018171,
3.25252168086323));
#24681=CARTESIAN_POINT('Ctrl Pts',(0.0297767959924581,0.129955593439766,
3.25515409237185));
#24682=CARTESIAN_POINT('Ctrl Pts',(-0.0175253881210462,0.132166465554107,
3.25778650388046));
#24683=CARTESIAN_POINT('Ctrl Pts',(-0.0550318099545696,0.114072266689479,
3.26041891538907));
#24684=CARTESIAN_POINT('Ctrl Pts',(-0.0925382317880931,0.09597806782485,
3.26305132689768));
#24685=CARTESIAN_POINT('Ctrl Pts',(-0.120248891341636,0.0575787979812516,
3.26568373840629));
#24686=CARTESIAN_POINT('Ctrl Pts',(-0.125602141267406,0.0162814079119122,
3.26831614991491));
#24687=CARTESIAN_POINT('Ctrl Pts',(-0.126297505847784,0.0109170511726472,
3.26865808906392));
#24688=CARTESIAN_POINT('Ctrl Pts',(-0.126615635779588,0.00550379470022512,
3.26900002821293));
#24689=CARTESIAN_POINT('Ctrl Pts',(-0.126573425356775,8.55484528903966E-5,
3.26934196736194));
#24690=CARTESIAN_POINT('Origin',(0.,0.,3.1));
#24691=CARTESIAN_POINT('',(-0.126252746279467,2.59119664437757E-5,3.31934196736194));
#24692=CARTESIAN_POINT('',(-0.126362016509238,-0.00010321110317447,3.30565803263806));
#24693=CARTESIAN_POINT('',(-0.12645,1.54856587752183E-17,3.1));
#24694=CARTESIAN_POINT('Ctrl Pts',(-0.126362016509238,-0.00010321110317447,
3.30565803263806));
#24695=CARTESIAN_POINT('Ctrl Pts',(-0.126135404540093,0.0289035586789932,
3.30383529641321));
#24696=CARTESIAN_POINT('Ctrl Pts',(-0.116200394811108,0.0580506048820654,
3.30201256018836));
#24697=CARTESIAN_POINT('Ctrl Pts',(-0.0979095549055491,0.080341149659951,
3.30018982396351));
#24698=CARTESIAN_POINT('Ctrl Pts',(-0.0714937648350404,0.112533348293265,
3.2975574124549));
#24699=CARTESIAN_POINT('Ctrl Pts',(-0.0276498958846022,0.130424676138957,
3.29492500094628));
#24700=CARTESIAN_POINT('Ctrl Pts',(0.0137469847697539,0.125904732556904,
3.29229258943767));
#24701=CARTESIAN_POINT('Ctrl Pts',(0.05514386542411,0.12138478897485,3.28966017792906));
#24702=CARTESIAN_POINT('Ctrl Pts',(0.0940937577823839,0.0944535739650504,
3.28702776642045));
#24703=CARTESIAN_POINT('Ctrl Pts',(0.112940105850529,0.057319401261323,
3.28439535491184));
#24704=CARTESIAN_POINT('Ctrl Pts',(0.131786453918674,0.0201852285575958,
3.28176294340322));
#24705=CARTESIAN_POINT('Ctrl Pts',(0.13052925769669,-0.0271519018400594,
3.27913053189461));
#24706=CARTESIAN_POINT('Ctrl Pts',(0.109738422623206,-0.0632333762395775,
3.276498120386));
#24707=CARTESIAN_POINT('Ctrl Pts',(0.0889475875497212,-0.099314850639096,
3.27386570887739));
#24708=CARTESIAN_POINT('Ctrl Pts',(0.0486231136247353,-0.124140669040477,
3.27123329736878));
#24709=CARTESIAN_POINT('Ctrl Pts',(0.00704467477488957,-0.126456924791809,
3.26860088586016));
#24710=CARTESIAN_POINT('Ctrl Pts',(-0.0345337640749562,-0.128773180543141,
3.26596847435155));
#24711=CARTESIAN_POINT('Ctrl Pts',(-0.0773661678496626,-0.108579873644424,
3.26333606284294));
#24712=CARTESIAN_POINT('Ctrl Pts',(-0.102035981333843,-0.0750309255155824,
3.26070365133433));
#24713=CARTESIAN_POINT('Ctrl Pts',(-0.117797761200207,-0.0535961815725874,
3.25902177843557));
#24714=CARTESIAN_POINT('Ctrl Pts',(-0.126145472985543,-0.026709592283637,
3.25733990553681));
#24715=CARTESIAN_POINT('Ctrl Pts',(-0.126309785017077,8.34376343069358E-5,
3.25565803263806));
#24716=CARTESIAN_POINT('Ctrl Pts',(-0.126573425356775,8.55484528903966E-5,
3.26934196736194));
#24717=CARTESIAN_POINT('Ctrl Pts',(-0.126290679707385,-0.0362084626390545,
3.27163243972154));
#24718=CARTESIAN_POINT('Ctrl Pts',(-0.109839596819478,-0.0727263630692267,
3.27392291208114));
#24719=CARTESIAN_POINT('Ctrl Pts',(-0.0822978965038287,-0.0962706516317226,
3.27621338444074));
#24720=CARTESIAN_POINT('Ctrl Pts',(-0.0506445615164858,-0.123329810810936,
3.27884579594935));
#24721=CARTESIAN_POINT('Ctrl Pts',(-0.00434205124380389,-0.133252618874282,
3.28147820745796));
#24722=CARTESIAN_POINT('Ctrl Pts',(0.0356200290599969,-0.121540921768417,
3.28411061896657));
#24723=CARTESIAN_POINT('Ctrl Pts',(0.0755821093637979,-0.109829224662552,
3.28674303047519));
#24724=CARTESIAN_POINT('Ctrl Pts',(0.109203759698717,-0.0764830223874748,
3.2893754419838));
#24725=CARTESIAN_POINT('Ctrl Pts',(0.121243794125388,-0.0366186362475693,
3.29200785349241));
#24726=CARTESIAN_POINT('Ctrl Pts',(0.133283828552059,0.00324574989233616,
3.29464026500102));
#24727=CARTESIAN_POINT('Ctrl Pts',(0.123742247070482,0.0496283198970706,
3.29727267650964));
#24728=CARTESIAN_POINT('Ctrl Pts',(0.0969443881476166,0.0815031762647041,
3.29990508801825));
#24729=CARTESIAN_POINT('Ctrl Pts',(0.0701465292247518,0.113378032632337,
3.30253749952686));
#24730=CARTESIAN_POINT('Ctrl Pts',(0.0260923928606002,0.130745175362871,
3.30516991103547));
#24731=CARTESIAN_POINT('Ctrl Pts',(-0.0152476364742436,0.125731824597042,
3.30780232254408));
#24732=CARTESIAN_POINT('Ctrl Pts',(-0.0565876658090873,0.120718473831214,
3.31043473405269));
#24733=CARTESIAN_POINT('Ctrl Pts',(-0.095213588114623,0.0933246295690233,
3.31306714556131));
#24734=CARTESIAN_POINT('Ctrl Pts',(-0.113615707760984,0.0559683221521016,
3.31569955706992));
#24735=CARTESIAN_POINT('Ctrl Pts',(-0.122103244730499,0.0387386200124153,
3.31691369383393));
#24736=CARTESIAN_POINT('Ctrl Pts',(-0.12628858288157,0.0193896083672227,
3.31812783059793));
#24737=CARTESIAN_POINT('Ctrl Pts',(-0.126252746279467,2.59119664437757E-5,
3.31934196736194));
#24738=CARTESIAN_POINT('Origin',(0.,0.,3.1));
#24739=CARTESIAN_POINT('',(-0.126482040448775,-0.000110013702131137,3.36934196736194));
#24740=CARTESIAN_POINT('',(-0.126649735277799,1.79833793418055E-5,3.35565803263806));
#24741=CARTESIAN_POINT('',(-0.12645,1.54856587752183E-17,3.1));
#24742=CARTESIAN_POINT('Ctrl Pts',(-0.126649735277799,1.79833793418055E-5,
3.35565803263806));
#24743=CARTESIAN_POINT('Ctrl Pts',(-0.126651722007443,0.00100711151136191,
3.35559551030682));
#24744=CARTESIAN_POINT('Ctrl Pts',(-0.126641125668946,0.0019961959922384,
3.35553298797559));
#24745=CARTESIAN_POINT('Ctrl Pts',(-0.126617815335903,0.00298498074413288,
3.35547046564436));
#24746=CARTESIAN_POINT('Ctrl Pts',(-0.12563636778334,0.0446163196439928,
3.35283805413574));
#24747=CARTESIAN_POINT('Ctrl Pts',(-0.102116718771259,0.085716326541524,
3.35020564262713));
#24748=CARTESIAN_POINT('Ctrl Pts',(-0.0667206692597134,0.107653767068442,
3.34757323111852));
#24749=CARTESIAN_POINT('Ctrl Pts',(-0.0313246197481669,0.12959120759536,
3.34494081960991));
#24750=CARTESIAN_POINT('Ctrl Pts',(0.0159478302628458,0.132366081751665,
3.3423084081013));
#24751=CARTESIAN_POINT('Ctrl Pts',(0.0536673876466801,0.114720498489436,
3.33967599659268));
#24752=CARTESIAN_POINT('Ctrl Pts',(0.0913869450305144,0.0970749152272078,
3.33704358508407));
#24753=CARTESIAN_POINT('Ctrl Pts',(0.11955360978717,0.059008874546446,3.33441117357546));
#24754=CARTESIAN_POINT('Ctrl Pts',(0.12539902073952,0.0177782695461103,
3.33177876206685));
#24755=CARTESIAN_POINT('Ctrl Pts',(0.13124443169187,-0.0234523354542255,
3.32914635055824));
#24756=CARTESIAN_POINT('Ctrl Pts',(0.114768588839913,-0.0678475047741352,
3.32651393904963));
#24757=CARTESIAN_POINT('Ctrl Pts',(0.083440232769335,-0.0952822587152781,
3.32388152754101));
#24758=CARTESIAN_POINT('Ctrl Pts',(0.0521118766987572,-0.122717012656421,
3.3212491160324));
#24759=CARTESIAN_POINT('Ctrl Pts',(0.00593100740955835,-0.133191351218797,
3.31861670452379));
#24760=CARTESIAN_POINT('Ctrl Pts',(-0.0341679114813036,-0.121957103505662,
3.31598429301518));
#24761=CARTESIAN_POINT('Ctrl Pts',(-0.0742668303721658,-0.110722855792528,
3.31335188150657));
#24762=CARTESIAN_POINT('Ctrl Pts',(-0.108283798864691,-0.0777800218038817,
3.31071946999795));
#24763=CARTESIAN_POINT('Ctrl Pts',(-0.120798427515664,-0.0380620700990904,
3.30808705848934));
#24764=CARTESIAN_POINT('Ctrl Pts',(-0.124647668210362,-0.0258456503973156,
3.30727738320558));
#24765=CARTESIAN_POINT('Ctrl Pts',(-0.126462679516819,-0.0129882705177865,
3.30646770792182));
#24766=CARTESIAN_POINT('Ctrl Pts',(-0.126362016509238,-0.00010321110317447,
3.30565803263806));
#24767=CARTESIAN_POINT('Ctrl Pts',(-0.126252746279467,2.59119664437757E-5,
3.31934196736194));
#24768=CARTESIAN_POINT('Ctrl Pts',(-0.126210884316958,-0.0225934851076951,
3.32076024210655));
#24769=CARTESIAN_POINT('Ctrl Pts',(-0.120409070525885,-0.0452329200835406,
3.32217851685115));
#24770=CARTESIAN_POINT('Ctrl Pts',(-0.108976454281191,-0.064537698648537,
3.32359679159575));
#24771=CARTESIAN_POINT('Ctrl Pts',(-0.0877567641678496,-0.100368641460601,
3.32622920310437));
#24772=CARTESIAN_POINT('Ctrl Pts',(-0.047139066953979,-0.124711756513075,
3.32886161461298));
#24773=CARTESIAN_POINT('Ctrl Pts',(-0.00553595897255799,-0.126531953643381,
3.33149402612159));
#24774=CARTESIAN_POINT('Ctrl Pts',(0.0360671490088627,-0.128352150773687,
3.3341264376302));
#24775=CARTESIAN_POINT('Ctrl Pts',(0.0786556677578339,-0.107649429981826,
3.33675884913881));
#24776=CARTESIAN_POINT('Ctrl Pts',(0.102923598708863,-0.0738086374577052,
3.33939126064743));
#24777=CARTESIAN_POINT('Ctrl Pts',(0.127191529659892,-0.0399678449335842,
3.34202367215604));
#24778=CARTESIAN_POINT('Ctrl Pts',(0.133138872812978,0.00701101932279596,
3.34465608366465));
#24779=CARTESIAN_POINT('Ctrl Pts',(0.118069610514671,0.0458317489024548,
3.34728849517326));
#24780=CARTESIAN_POINT('Ctrl Pts',(0.103000348216365,0.0846524784821133,
3.34992090668187));
#24781=CARTESIAN_POINT('Ctrl Pts',(0.0669144804666656,0.11531507338505,
3.35255331819048));
#24782=CARTESIAN_POINT('Ctrl Pts',(0.0261702590074494,0.123919730785983,
3.3551857296991));
#24783=CARTESIAN_POINT('Ctrl Pts',(-0.0145739624517671,0.132524388186917,
3.35781814120771));
#24784=CARTESIAN_POINT('Ctrl Pts',(-0.059976537620501,0.119071108085846,
3.36045055271632));
#24785=CARTESIAN_POINT('Ctrl Pts',(-0.0894558149920353,0.0896584591581523,
3.36308296422493));
#24786=CARTESIAN_POINT('Ctrl Pts',(-0.112819802593213,0.0663472783512584,
3.36516929860394));
#24787=CARTESIAN_POINT('Ctrl Pts',(-0.126181642003826,0.033011291498231,
3.36725563298294));
#24788=CARTESIAN_POINT('Ctrl Pts',(-0.126482040448775,-0.000110013702131137,
3.36934196736194));
#24789=CARTESIAN_POINT('Origin',(0.,0.,3.1));
#24790=CARTESIAN_POINT('',(-0.126579711874066,8.26312290282544E-5,3.41934196736194));
#24791=CARTESIAN_POINT('',(-0.126315008613134,8.61315354740502E-5,3.40565803263806));
#24792=CARTESIAN_POINT('',(-0.12645,1.54856587752183E-17,3.1));
#24793=CARTESIAN_POINT('Ctrl Pts',(-0.126315008613134,8.61315354740502E-5,
3.40565803263806));
#24794=CARTESIAN_POINT('Ctrl Pts',(-0.12640952887744,0.0149751122618111,
3.40472331269183));
#24795=CARTESIAN_POINT('Ctrl Pts',(-0.123973978584825,0.029834173019371,
3.4037885927456));
#24796=CARTESIAN_POINT('Ctrl Pts',(-0.118870621145655,0.0437122030848606,
3.40285387279937));
#24797=CARTESIAN_POINT('Ctrl Pts',(-0.104498255487237,0.0827963011707195,
3.40022146129076));
#24798=CARTESIAN_POINT('Ctrl Pts',(-0.0689667030308244,0.114099547595362,
3.39758904978215));
#24799=CARTESIAN_POINT('Ctrl Pts',(-0.0283829362832705,0.123431722821457,
3.39495663827353));
#24800=CARTESIAN_POINT('Ctrl Pts',(0.0122008304642834,0.132763898047552,
3.39232422676492));
#24801=CARTESIAN_POINT('Ctrl Pts',(0.0578368115029788,0.120125002075099,
3.38969181525631));
#24802=CARTESIAN_POINT('Ctrl Pts',(0.0878375490289461,0.0912444313426293,
3.3870594037477));
#24803=CARTESIAN_POINT('Ctrl Pts',(0.117838286554913,0.0623638606101592,
3.38442699223909));
#24804=CARTESIAN_POINT('Ctrl Pts',(0.132203780568153,0.0172416151176717,
3.38179458073047));
#24805=CARTESIAN_POINT('Ctrl Pts',(0.124421942484303,-0.0236677311728431,
3.37916216922186));
#24806=CARTESIAN_POINT('Ctrl Pts',(0.116640104400452,-0.0645770774633583,
3.37652975771325));
#24807=CARTESIAN_POINT('Ctrl Pts',(0.0867109342195124,-0.1012735245519,
3.37389734620464));
#24808=CARTESIAN_POINT('Ctrl Pts',(0.0482017626101867,-0.117122036149449,
3.37126493469603));
#24809=CARTESIAN_POINT('Ctrl Pts',(0.00969259100086189,-0.132970547746997,
3.36863252318742));
#24810=CARTESIAN_POINT('Ctrl Pts',(-0.0373965820368482,-0.127971123853552,
3.3660001116788));
#24811=CARTESIAN_POINT('Ctrl Pts',(-0.0717195455091802,-0.104390076455735,
3.36336770017019));
#24812=CARTESIAN_POINT('Ctrl Pts',(-0.105227305247545,-0.0813691018472357,
3.36079781099281));
#24813=CARTESIAN_POINT('Ctrl Pts',(-0.126568073655319,-0.0406386849075436,
3.35822792181544));
#24814=CARTESIAN_POINT('Ctrl Pts',(-0.126649735277799,1.79833793418055E-5,
3.35565803263806));
#24815=CARTESIAN_POINT('Ctrl Pts',(-0.126482040448775,-0.000110013702131137,
3.36934196736194));
#24816=CARTESIAN_POINT('Ctrl Pts',(-0.126560666733329,-0.00877918363707953,
3.36988804449155));
#24817=CARTESIAN_POINT('Ctrl Pts',(-0.125744482172779,-0.0174336462000347,
3.37043412162116));
#24818=CARTESIAN_POINT('Ctrl Pts',(-0.123978629867097,-0.0258897947229394,
3.37098019875077));
#24819=CARTESIAN_POINT('Ctrl Pts',(-0.115466187796289,-0.0666533819220227,
3.37361261025938));
#24820=CARTESIAN_POINT('Ctrl Pts',(-0.0848853240803387,-0.102808538565874,
3.37624502176799));
#24821=CARTESIAN_POINT('Ctrl Pts',(-0.046098791601206,-0.117965603239704,
3.3788774332766));
#24822=CARTESIAN_POINT('Ctrl Pts',(-0.00731225912207339,-0.133122667913533,
3.38150984478522));
#24823=CARTESIAN_POINT('Ctrl Pts',(0.0396799421202415,-0.127281640617341,
3.38414225629383));
#24824=CARTESIAN_POINT('Ctrl Pts',(0.0735755598654084,-0.103090344478252,
3.38677466780244));
#24825=CARTESIAN_POINT('Ctrl Pts',(0.107471177610575,-0.0788990483391635,
3.38940707931105));
#24826=CARTESIAN_POINT('Ctrl Pts',(0.128270211858594,-0.0363574833571786,
3.39203949081966));
#24827=CARTESIAN_POINT('Ctrl Pts',(0.126544156121574,0.00524963674486975,
3.39467190232827));
#24828=CARTESIAN_POINT('Ctrl Pts',(0.124818100384554,0.0468567568469189,
3.39730431383689));
#24829=CARTESIAN_POINT('Ctrl Pts',(0.100566954662495,0.0875294320690312,
3.3999367253455));
#24830=CARTESIAN_POINT('Ctrl Pts',(0.0647841180740634,0.108830143717421,
3.40256913685411));
#24831=CARTESIAN_POINT('Ctrl Pts',(0.0290012814856321,0.13013085536581,
3.40520154836272));
#24832=CARTESIAN_POINT('Ctrl Pts',(-0.0183132459691715,0.132059603440478,
3.40783395987133));
#24833=CARTESIAN_POINT('Ctrl Pts',(-0.0557110968410662,0.113742058272906,
3.41046637137995));
#24834=CARTESIAN_POINT('Ctrl Pts',(-0.0931089477129611,0.0954245131053351,
3.41309878288856));
#24835=CARTESIAN_POINT('Ctrl Pts',(-0.120590122001947,0.056860674695525,
3.41573119439717));
#24836=CARTESIAN_POINT('Ctrl Pts',(-0.125697001391323,0.0155320950411155,
3.41836360590578));
#24837=CARTESIAN_POINT('Ctrl Pts',(-0.126329675264624,0.0104120382364903,
3.41868972639117));
#24838=CARTESIAN_POINT('Ctrl Pts',(-0.126618950983805,0.00524954849512788,
3.41901584687656));
#24839=CARTESIAN_POINT('Ctrl Pts',(-0.126579711874066,8.26312290282544E-5,
3.41934196736194));
#24840=CARTESIAN_POINT('Origin',(0.,0.,3.1));
#24841=CARTESIAN_POINT('',(-0.126254420230949,2.98387352259399E-5,3.46934196736194));
#24842=CARTESIAN_POINT('',(-0.126355565467006,-0.000101493988421879,3.45565803263806));
#24843=CARTESIAN_POINT('',(-0.12645,1.54856587752183E-17,3.1));
#24844=CARTESIAN_POINT('Ctrl Pts',(-0.126355565467006,-0.000101493988421879,
3.45565803263806));
#24845=CARTESIAN_POINT('Ctrl Pts',(-0.126135472102513,0.0286572548844595,
3.45385111507683));
#24846=CARTESIAN_POINT('Ctrl Pts',(-0.116386929963108,0.0575510084273647,
3.45204419751561));
#24847=CARTESIAN_POINT('Ctrl Pts',(-0.0983869251245805,0.079755841232973,
3.45023727995438));
#24848=CARTESIAN_POINT('Ctrl Pts',(-0.0721635816202546,0.112104996877157,
3.44760486844577));
#24849=CARTESIAN_POINT('Ctrl Pts',(-0.0284271866124946,0.130257467927816,
3.44497245693716));
#24850=CARTESIAN_POINT('Ctrl Pts',(0.0129959124187107,0.125984473413918,
3.44234004542855));
#24851=CARTESIAN_POINT('Ctrl Pts',(0.0544190114499162,0.121711478900021,
3.43970763391994));
#24852=CARTESIAN_POINT('Ctrl Pts',(0.0935288145045671,0.0950130188215667,
3.43707522241132));
#24853=CARTESIAN_POINT('Ctrl Pts',(0.112596275634196,0.0579918958508686,
3.43444281090271));
#24854=CARTESIAN_POINT('Ctrl Pts',(0.131663736763825,0.0209707728801704,
3.4318103993941));
#24855=CARTESIAN_POINT('Ctrl Pts',(0.130688855968432,-0.0263730129827715,
3.42917798788549));
#24856=CARTESIAN_POINT('Ctrl Pts',(0.110113561023984,-0.0625778311060434,
3.42654557637688));
#24857=CARTESIAN_POINT('Ctrl Pts',(0.0895382660795356,-0.0987826492293151,
3.42391316486827));
#24858=CARTESIAN_POINT('Ctrl Pts',(0.0493625569860325,-0.123848499612917,
3.42128075335965));
#24859=CARTESIAN_POINT('Ctrl Pts',(0.00779867036970612,-0.12641266555449,
3.41864834185104));
#24860=CARTESIAN_POINT('Ctrl Pts',(-0.0337652162466206,-0.128976831496062,
3.41601593034243));
#24861=CARTESIAN_POINT('Ctrl Pts',(-0.0767172803857706,-0.109039312995606,
3.41338351883382));
#24862=CARTESIAN_POINT('Ctrl Pts',(-0.101586723025134,-0.0756380788718395,
3.41075110732521));
#24863=CARTESIAN_POINT('Ctrl Pts',(-0.117625493100354,-0.0540969964234629,
3.40905341576282));
#24864=CARTESIAN_POINT('Ctrl Pts',(-0.126143335529839,-0.0269560826095475,
3.40735572420044));
#24865=CARTESIAN_POINT('Ctrl Pts',(-0.126315008613134,8.61315354740502E-5,
3.40565803263806));
#24866=CARTESIAN_POINT('Ctrl Pts',(-0.126579711874066,8.26312290282544E-5,
3.41934196736194));
#24867=CARTESIAN_POINT('Ctrl Pts',(-0.126302216866535,-0.0364572840554096,
3.42164825838517));
#24868=CARTESIAN_POINT('Ctrl Pts',(-0.109595120153288,-0.0732186276029635,
3.42395454940839));
#24869=CARTESIAN_POINT('Ctrl Pts',(-0.0817223269051259,-0.0967597200814019,
3.42626084043162));
#24870=CARTESIAN_POINT('Ctrl Pts',(-0.0499081885397876,-0.123629634650501,
3.42889325194023));
#24871=CARTESIAN_POINT('Ctrl Pts',(-0.00354732731934525,-0.133276142889689,
3.43152566344884));
#24872=CARTESIAN_POINT('Ctrl Pts',(0.0363442001504806,-0.121326341846207,
3.43415807495745));
#24873=CARTESIAN_POINT('Ctrl Pts',(0.0762357276203061,-0.109376540802726,
3.43679048646606));
#24874=CARTESIAN_POINT('Ctrl Pts',(0.109657921339515,-0.0758304304765741,
3.43942289797468));
#24875=CARTESIAN_POINT('Ctrl Pts',(0.121460011995994,-0.0358949527457304,
3.44205530948329));
#24876=CARTESIAN_POINT('Ctrl Pts',(0.133262102652474,0.00404052498511346,
3.4446877209919));
#24877=CARTESIAN_POINT('Ctrl Pts',(0.123444090246223,0.0503653701206494,
3.44732013250051));
#24878=CARTESIAN_POINT('Ctrl Pts',(0.0964566233770265,0.0820798513966518,
3.44995254400912));
#24879=CARTESIAN_POINT('Ctrl Pts',(0.0694691565078302,0.113794332672654,
3.45258495551774));
#24880=CARTESIAN_POINT('Ctrl Pts',(0.0253122351756883,0.130898450089123,
3.45521736702635));
#24881=CARTESIAN_POINT('Ctrl Pts',(-0.0159971621245858,0.12563865949158,
3.45784977853496));
#24882=CARTESIAN_POINT('Ctrl Pts',(-0.0573065594248602,0.120378868894038,
3.46048219004357));
#24883=CARTESIAN_POINT('Ctrl Pts',(-0.0957684326932668,0.0927551702824843,
3.46311460155218));
#24884=CARTESIAN_POINT('Ctrl Pts',(-0.113947452310361,0.0552897855612304,
3.46574701306079));
#24885=CARTESIAN_POINT('Ctrl Pts',(-0.122222848532838,0.0382349107810562,
3.46694533116118));
#24886=CARTESIAN_POINT('Ctrl Pts',(-0.126295183358791,0.0191406182899676,
3.46814364926156));
#24887=CARTESIAN_POINT('Ctrl Pts',(-0.126254420230949,2.98387352259399E-5,
3.46934196736194));
#24888=CARTESIAN_POINT('Origin',(0.,0.,3.1));
#24889=CARTESIAN_POINT('',(-0.126474550616365,-0.00011099430647141,3.51934196736194));
#24890=CARTESIAN_POINT('',(-0.12665116202208,1.34725138570783E-5,3.50565803263806));
#24891=CARTESIAN_POINT('',(-0.12645,1.54856587752183E-17,3.1));
#24892=CARTESIAN_POINT('Ctrl Pts',(-0.12665116202208,1.34725138570783E-5,
3.50565803263806));
#24893=CARTESIAN_POINT('Ctrl Pts',(-0.126652289762307,0.000752320916696393,
3.50561132897045));
#24894=CARTESIAN_POINT('Ctrl Pts',(-0.126646377467723,0.00149115078533116,
3.50556462530284));
#24895=CARTESIAN_POINT('Ctrl Pts',(-0.126633369929918,0.00222985570861129,
3.50551792163523));
#24896=CARTESIAN_POINT('Ctrl Pts',(-0.125900211401467,0.0438663147077999,
3.50288551012662));
#24897=CARTESIAN_POINT('Ctrl Pts',(-0.102626068622182,0.0851058329421116,
3.50025309861801));
#24898=CARTESIAN_POINT('Ctrl Pts',(-0.067361469104998,0.107253962401741,
3.4976206871094));
#24899=CARTESIAN_POINT('Ctrl Pts',(-0.0320968695878142,0.129402091861371,
3.49498827560079));
#24900=CARTESIAN_POINT('Ctrl Pts',(0.0151581866672683,0.132458832546319,
3.49235586409217));
#24901=CARTESIAN_POINT('Ctrl Pts',(0.0529823007948782,0.115038504173862,
3.48972345258356));
#24902=CARTESIAN_POINT('Ctrl Pts',(0.0908064149224882,0.0976181758014056,
3.48709104107495));
#24903=CARTESIAN_POINT('Ctrl Pts',(0.119199586922625,0.0597207783715444,
3.48445862956634));
#24904=CARTESIAN_POINT('Ctrl Pts',(0.125290771676778,0.0185257643337426,
3.48182621805773));
#24905=CARTESIAN_POINT('Ctrl Pts',(0.131381956430931,-0.0226692497040593,
3.47919380654911));
#24906=CARTESIAN_POINT('Ctrl Pts',(0.115171153939098,-0.0671618803498017,
3.4765613950405));
#24907=CARTESIAN_POINT('Ctrl Pts',(0.0840069606582608,-0.0947829713159226,
3.47392898353189));
#24908=CARTESIAN_POINT('Ctrl Pts',(0.0528427673774234,-0.122404062282043,
3.47129657202328));
#24909=CARTESIAN_POINT('Ctrl Pts',(0.00672518330758078,-0.133153613568543,
3.46866416051467));
#24910=CARTESIAN_POINT('Ctrl Pts',(-0.0334400173720784,-0.122158694217057,
3.46603174900606));
#24911=CARTESIAN_POINT('Ctrl Pts',(-0.0736052180517379,-0.111163774865571,
3.46339933749744));
#24912=CARTESIAN_POINT('Ctrl Pts',(-0.107818035341214,-0.0784243848761005,
3.46076692598883));
#24913=CARTESIAN_POINT('Ctrl Pts',(-0.120569297985506,-0.0387817697625104,
3.45813451448022));
#24914=CARTESIAN_POINT('Ctrl Pts',(-0.12456794717085,-0.0263503019894106,
3.45730902053283));
#24915=CARTESIAN_POINT('Ctrl Pts',(-0.126456115566329,-0.013239986655944,
3.45648352658544));
#24916=CARTESIAN_POINT('Ctrl Pts',(-0.126355565467006,-0.000101493988421879,
3.45565803263806));
#24917=CARTESIAN_POINT('Ctrl Pts',(-0.126254420230949,2.98387352259399E-5,
3.46934196736194));
#24918=CARTESIAN_POINT('Ctrl Pts',(-0.126205636746063,-0.0228410859189539,
3.47077606077017));
#24919=CARTESIAN_POINT('Ctrl Pts',(-0.120265979813939,-0.045735623724726,
3.4722101541784));
#24920=CARTESIAN_POINT('Ctrl Pts',(-0.108589648601543,-0.0651864304899691,
3.47364424758663));
#24921=CARTESIAN_POINT('Ctrl Pts',(-0.0871566593098471,-0.100890190988961,
3.47627665909524));
#24922=CARTESIAN_POINT('Ctrl Pts',(-0.0463945147606729,-0.124990641155991,
3.47890907060385));
#24923=CARTESIAN_POINT('Ctrl Pts',(-0.00478129205129982,-0.126562712056682,
3.48154148211247));
#24924=CARTESIAN_POINT('Ctrl Pts',(0.0368319306580732,-0.128134782957373,
3.48417389362108));
#24925=CARTESIAN_POINT('Ctrl Pts',(0.0792962315276452,-0.107178474591724,
3.48680630512969));
#24926=CARTESIAN_POINT('Ctrl Pts',(0.103361923070995,-0.0731935540746058,
3.4894387166383));
#24927=CARTESIAN_POINT('Ctrl Pts',(0.127427614614345,-0.0392086335574879,
3.49207112814691));
#24928=CARTESIAN_POINT('Ctrl Pts',(0.133094696831473,0.00780489911109889,
3.49470353965553));
#24929=CARTESIAN_POINT('Ctrl Pts',(0.117794195954941,0.0465350563376696,
3.49733595116414));
#24930=CARTESIAN_POINT('Ctrl Pts',(0.102493695078409,0.0852652135642405,
3.49996836267275));
#24931=CARTESIAN_POINT('Ctrl Pts',(0.0662256111082176,0.115711995348795,
3.50260077418136));
#24932=CARTESIAN_POINT('Ctrl Pts',(0.0254308018677658,0.124073556121702,
3.50523318568997));
#24933=CARTESIAN_POINT('Ctrl Pts',(-0.0153640073726858,0.13243511689461,
3.50786559719859));
#24934=CARTESIAN_POINT('Ctrl Pts',(-0.0606855418833975,0.118711456655871,
3.5104980087072));
#24935=CARTESIAN_POINT('Ctrl Pts',(-0.0899888963160071,0.0891234688732135,
3.51313042021581));
#24936=CARTESIAN_POINT('Ctrl Pts',(-0.113037365625426,0.0658511220193964,
3.51520093593118));
#24937=CARTESIAN_POINT('Ctrl Pts',(-0.12617608552629,0.032764207609907,
3.51727145164656));
#24938=CARTESIAN_POINT('Ctrl Pts',(-0.126474550616365,-0.00011099430647141,
3.51934196736194));
#24939=CARTESIAN_POINT('Origin',(0.,0.,3.1));
#24940=CARTESIAN_POINT('',(-0.126585968300139,7.56654190205152E-5,3.56934196736194));
#24941=CARTESIAN_POINT('',(-0.126320239448181,8.84447983197572E-5,3.55565803263806));
#24942=CARTESIAN_POINT('',(-0.12645,1.54856587752183E-17,3.1));
#24943=CARTESIAN_POINT('',(0.0958116152722374,0.0825211298936506,3.6));
#24944=CARTESIAN_POINT('Ctrl Pts',(-0.126585968300139,7.56654190205153E-5,
3.56934196736194));
#24945=CARTESIAN_POINT('Ctrl Pts',(-0.126314022279117,-0.0367013527487602,
3.57166407704879));
#24946=CARTESIAN_POINT('Ctrl Pts',(-0.109347743467702,-0.0736867832767084,
3.57398618673564));
#24947=CARTESIAN_POINT('Ctrl Pts',(-0.0811433985852254,-0.0972323262171825,
3.57630829642249));
#24948=CARTESIAN_POINT('Ctrl Pts',(-0.0491701276919849,-0.123924242866945,
3.57894070793111));
#24949=CARTESIAN_POINT('Ctrl Pts',(-0.00275464590947525,-0.133344354062013,
3.58157311943972));
#24950=CARTESIAN_POINT('Ctrl Pts',(0.0370665801591162,-0.121131220741312,
3.58420553094833));
#24951=CARTESIAN_POINT('Ctrl Pts',(0.0768878062277077,-0.108918087420612,
3.58683794245694));
#24952=CARTESIAN_POINT('Ctrl Pts',(0.110114776582381,-0.0750717095841421,
3.58947035396555));
#24953=CARTESIAN_POINT('Ctrl Pts',(0.121670197120012,-0.035135491975585,
3.59210276547417));
#24954=CARTESIAN_POINT('Ctrl Pts',(0.133225617657642,0.004800725632972,
3.59473517698278));
#24955=CARTESIAN_POINT('Ctrl Pts',(0.12310948837823,0.0508267830136165,
3.59736758849139));
#24956=CARTESIAN_POINT('Ctrl Pts',(0.0958116152722374,0.0825211298936506,
3.6));
#24957=CARTESIAN_POINT('',(-0.0959914412498779,0.0826500850312143,3.6));
#24958=CARTESIAN_POINT('Origin',(0.,0.,3.6));
#24959=CARTESIAN_POINT('Ctrl Pts',(-0.0959917963302685,0.0826503396631676,
3.6));
#24960=CARTESIAN_POINT('Ctrl Pts',(-0.0697118464080321,0.11301028941478,
3.59746250047314));
#24961=CARTESIAN_POINT('Ctrl Pts',(-0.0277082920252644,0.129939468632456,
3.59492500094628));
#24962=CARTESIAN_POINT('Ctrl Pts',(0.0122513409849536,0.126048715034846,
3.59238750141942));
#24963=CARTESIAN_POINT('Ctrl Pts',(0.0537056138636675,0.122012432687161,
3.58975508991081));
#24964=CARTESIAN_POINT('Ctrl Pts',(0.0929602052199782,0.095569602745952,
3.5871226784022));
#24965=CARTESIAN_POINT('Ctrl Pts',(0.112244799198078,0.058668125616663,
3.58449026689359));
#24966=CARTESIAN_POINT('Ctrl Pts',(0.131529393176178,0.0217666484873742,
3.58185785538498));
#24967=CARTESIAN_POINT('Ctrl Pts',(0.130843989776067,-0.0255934758299944,
3.57922544387636));
#24968=CARTESIAN_POINT('Ctrl Pts',(0.11048667870984,-0.0619230812123589,
3.57659303236775));
#24969=CARTESIAN_POINT('Ctrl Pts',(0.0901293676436137,-0.0982526865947235,
3.57396062085914));
#24970=CARTESIAN_POINT('Ctrl Pts',(0.0501001489112715,-0.123551773042084,
3.57132820935053));
#24971=CARTESIAN_POINT('Ctrl Pts',(0.00855140333287623,-0.126362339932449,
3.56869579784192));
#24972=CARTESIAN_POINT('Ctrl Pts',(-0.032997342245519,-0.129172906822815,
3.5660633863333));
#24973=CARTESIAN_POINT('Ctrl Pts',(-0.0760656146699672,-0.109494954156186,
3.56343097482469));
#24974=CARTESIAN_POINT('Ctrl Pts',(-0.101133339862815,-0.0762433587436205,
3.56079856331608));
#24975=CARTESIAN_POINT('Ctrl Pts',(-0.117450622825668,-0.0545989659182217,
3.55908505309007));
#24976=CARTESIAN_POINT('Ctrl Pts',(-0.126140944400475,-0.0272033229899018,
3.55737154286407));
#24977=CARTESIAN_POINT('Ctrl Pts',(-0.126320239448181,8.84447983197572E-5,
3.55565803263806));
#24978=CARTESIAN_POINT('Origin',(0.,0.,3.71042117235887));
#24979=CARTESIAN_POINT('',(-0.154532329218545,4.4775541170855E-5,2.73957882764113));
#24980=CARTESIAN_POINT('',(-0.154050519949587,1.7733618556367E-5,2.73542117235887));
#24981=CARTESIAN_POINT('',(-0.1543,1.43283619370552E-14,3.71042117235887));
#24982=CARTESIAN_POINT('',(0.03985138418574,-0.149064942821847,2.7));
#24983=CARTESIAN_POINT('Ctrl Pts',(-0.154050519949587,1.77336185563769E-5,
2.73542117235887));
#24984=CARTESIAN_POINT('Ctrl Pts',(-0.154066274679179,0.0248826176783822,
2.73414376094036));
#24985=CARTESIAN_POINT('Ctrl Pts',(-0.136678442565,0.100960491967761,2.73023393801324));
#24986=CARTESIAN_POINT('Ctrl Pts',(-0.0176337922607613,0.181151847216363,
2.72369170357751));
#24987=CARTESIAN_POINT('Ctrl Pts',(0.14217180017934,0.113903091069576,2.71579446905167));
#24988=CARTESIAN_POINT('Ctrl Pts',(0.172848115381474,-0.0569943527276058,
2.70789723452584));
#24989=CARTESIAN_POINT('Ctrl Pts',(0.0891618565332066,-0.135882161272415,
2.70263241150861));
#24990=CARTESIAN_POINT('Ctrl Pts',(0.0398513841857358,-0.149064942821848,
2.7));
#24991=CARTESIAN_POINT('',(-0.0398513841857137,-0.149064942821854,2.7));
#24992=CARTESIAN_POINT('Origin',(0.,0.,2.7));
#24993=CARTESIAN_POINT('Ctrl Pts',(-0.154532329218545,4.47755411708581E-5,
2.73957882764113));
#24994=CARTESIAN_POINT('Ctrl Pts',(-0.154541474731814,0.00247370285197769,
2.73945303065539));
#24995=CARTESIAN_POINT('Ctrl Pts',(-0.153393280968798,0.0557210645369631,
2.73669482216104));
#24996=CARTESIAN_POINT('Ctrl Pts',(-0.0921890914137533,0.156981837366664,
2.73130420215808));
#24997=CARTESIAN_POINT('Ctrl Pts',(0.081054919689294,0.163034936656946,
2.72340696763225));
#24998=CARTESIAN_POINT('Ctrl Pts',(0.180814453969382,0.0212164304176998,
2.71550973310641));
#24999=CARTESIAN_POINT('Ctrl Pts',(0.117409156055766,-0.137788854076994,
2.70770741056233));
#25000=CARTESIAN_POINT('Ctrl Pts',(0.00742265010309158,-0.161856516962739,
2.70253749952686));
#25001=CARTESIAN_POINT('Ctrl Pts',(-0.0399441884684105,-0.149319082708151,
2.7));
#25002=CARTESIAN_POINT('Origin',(0.,0.,3.71042117235887));
#25003=CARTESIAN_POINT('',(-0.154111134012939,9.12056675990702E-5,2.78957882764113));
#25004=CARTESIAN_POINT('',(-0.154375356381381,-0.000128347871137961,2.78542117235887));
#25005=CARTESIAN_POINT('',(-0.1543,1.43283619370552E-14,3.71042117235887));
#25006=CARTESIAN_POINT('Ctrl Pts',(-0.154375356381381,-0.000128347871137957,
2.78542117235887));
#25007=CARTESIAN_POINT('Ctrl Pts',(-0.154004490723256,0.0414883916240874,
2.78327156332537));
#25008=CARTESIAN_POINT('Ctrl Pts',(-0.115247407249284,0.134678118697344,
2.77848954278325));
#25009=CARTESIAN_POINT('Ctrl Pts',(0.0418557848916964,0.17717956471448,
2.77107511073252));
#25010=CARTESIAN_POINT('Ctrl Pts',(0.171243621830244,0.0618160489303277,
2.76317787620668));
#25011=CARTESIAN_POINT('Ctrl Pts',(0.145372553280857,-0.109598760687136,
2.75528064168085));
#25012=CARTESIAN_POINT('Ctrl Pts',(-0.0122890050489303,-0.181634550845065,
2.74738340715501));
#25013=CARTESIAN_POINT('Ctrl Pts',(-0.13512250192602,-0.104001863717814,
2.74076358404769));
#25014=CARTESIAN_POINT('Ctrl Pts',(-0.154033808293727,-0.0263574182340484,
2.73677617244897));
#25015=CARTESIAN_POINT('Ctrl Pts',(-0.154050519949587,1.77336185563769E-5,
2.73542117235887));
#25016=CARTESIAN_POINT('Ctrl Pts',(-0.154111134012939,9.12056675990824E-5,
2.78957882764113));
#25017=CARTESIAN_POINT('Ctrl Pts',(-0.154216904845773,0.0194969338944761,
2.7885808330404));
#25018=CARTESIAN_POINT('Ctrl Pts',(-0.141845660080373,0.0899592653630177,
2.78495042693105));
#25019=CARTESIAN_POINT('Ctrl Pts',(-0.0365555263461618,0.178349534836247,
2.7786876093131));
#25020=CARTESIAN_POINT('Ctrl Pts',(0.129354617910885,0.128110846926664,
2.77079037478726));
#25021=CARTESIAN_POINT('Ctrl Pts',(0.177988125847537,-0.0382780523762908,
2.76289314026143));
#25022=CARTESIAN_POINT('Ctrl Pts',(0.0652523050728403,-0.169960699505811,
2.75499590573559));
#25023=CARTESIAN_POINT('Ctrl Pts',(-0.10390483603623,-0.147913217635949,
2.74722446819549));
#25024=CARTESIAN_POINT('Ctrl Pts',(-0.154350096899974,-0.0483537169716228,
2.742085442164));
#25025=CARTESIAN_POINT('Ctrl Pts',(-0.154532329218545,4.47755411708581E-5,
2.73957882764113));
#25026=CARTESIAN_POINT('Origin',(0.,0.,3.71042117235887));
#25027=CARTESIAN_POINT('',(-0.154217143654561,-0.000131209131675823,2.83957882764113));
#25028=CARTESIAN_POINT('',(-0.154426485097132,0.00011404955978979,2.83542117235887));
#25029=CARTESIAN_POINT('',(-0.1543,1.43283619370552E-14,3.71042117235887));
#25030=CARTESIAN_POINT('Ctrl Pts',(-0.154426485097132,0.000114049559789811,
2.83542117235887));
#25031=CARTESIAN_POINT('Ctrl Pts',(-0.154488936846892,0.00764629898056818,
2.83503177721898));
#25032=CARTESIAN_POINT('Ctrl Pts',(-0.15057776842572,0.0660334076153961,
2.83200997057048));
#25033=CARTESIAN_POINT('Ctrl Pts',(-0.0761594594163292,0.165362226259928,
2.82635575241337));
#25034=CARTESIAN_POINT('Ctrl Pts',(0.0968288057644592,0.154172306963803,
2.81845851788754));
#25035=CARTESIAN_POINT('Ctrl Pts',(0.182029287997112,0.0032053357021354,
2.8105612833617));
#25036=CARTESIAN_POINT('Ctrl Pts',(0.102196604793212,-0.150667825661861,
2.80266404883587));
#25037=CARTESIAN_POINT('Ctrl Pts',(-0.0702903425019912,-0.167940860695529,
2.79476681431002));
#25038=CARTESIAN_POINT('Ctrl Pts',(-0.14944611336054,-0.069697339741445,
2.7890191888177));
#25039=CARTESIAN_POINT('Ctrl Pts',(-0.154458652857569,-0.00947547310228015,
2.78590397483398));
#25040=CARTESIAN_POINT('Ctrl Pts',(-0.154375356381381,-0.000128347871137957,
2.78542117235887));
#25041=CARTESIAN_POINT('Ctrl Pts',(-0.154217143654561,-0.000131209131675806,
2.83957882764113));
#25042=CARTESIAN_POINT('Ctrl Pts',(-0.153918019192818,0.0361710755121499,
2.8377086354254));
#25043=CARTESIAN_POINT('Ctrl Pts',(-0.123049963751881,0.124029060195803,
2.83320603170106));
#25044=CARTESIAN_POINT('Ctrl Pts',(0.0229951363840201,0.180599411232496,
2.82607101646811));
#25045=CARTESIAN_POINT('Ctrl Pts',(0.163793876249876,0.0794763606914083,
2.81817378194228));
#25046=CARTESIAN_POINT('Ctrl Pts',(0.1560922965942,-0.0937023067775016,
2.81027654741644));
#25047=CARTESIAN_POINT('Ctrl Pts',(0.00687287227597422,-0.181927677084725,
2.8023793128906));
#25048=CARTESIAN_POINT('Ctrl Pts',(-0.128932992743455,-0.114906920263654,
2.7954800729655));
#25049=CARTESIAN_POINT('Ctrl Pts',(-0.153937912998098,-0.0316895778160955,
2.79121324454901));
#25050=CARTESIAN_POINT('Ctrl Pts',(-0.154111134012939,9.12056675990824E-5,
2.78957882764113));
#25051=CARTESIAN_POINT('Origin',(0.,0.,3.71042117235887));
#25052=CARTESIAN_POINT('',(-0.154535784933253,3.81877733398595E-5,2.88957882764113));
#25053=CARTESIAN_POINT('',(-0.154054921884602,1.70237768407695E-5,2.88542117235887));
#25054=CARTESIAN_POINT('',(-0.1543,1.43283619370552E-14,3.71042117235887));
#25055=CARTESIAN_POINT('Ctrl Pts',(-0.154054921884602,1.70237768407841E-5,
2.88542117235887));
#25056=CARTESIAN_POINT('Ctrl Pts',(-0.154079346410273,0.0245707720672152,
2.88415957960399));
#25057=CARTESIAN_POINT('Ctrl Pts',(-0.1369997697474,0.100325734672348,2.88026557534049));
#25058=CARTESIAN_POINT('Ctrl Pts',(-0.0186809878927599,0.181096514045709,
2.87373915956839));
#25059=CARTESIAN_POINT('Ctrl Pts',(0.14142638889208,0.114645117640021,2.86584192504255));
#25060=CARTESIAN_POINT('Ctrl Pts',(0.173312464619039,-0.0557468952238434,
2.85794469051671));
#25061=CARTESIAN_POINT('Ctrl Pts',(0.0480683875166603,-0.175597144601074,
2.85004745599088));
#25062=CARTESIAN_POINT('Ctrl Pts',(-0.112431541495112,-0.138186203572753,
2.84253961660493));
#25063=CARTESIAN_POINT('Ctrl Pts',(-0.154066746922155,-0.0432736484708866,
2.8376641887276));
#25064=CARTESIAN_POINT('Ctrl Pts',(-0.154426485097132,0.000114049559789811,
2.83542117235887));
#25065=CARTESIAN_POINT('Ctrl Pts',(-0.154535784933253,3.8187773339879E-5,
2.88957882764113));
#25066=CARTESIAN_POINT('Ctrl Pts',(-0.154542902681706,0.00216158596911697,
2.88946884931902));
#25067=CARTESIAN_POINT('Ctrl Pts',(-0.153545003294962,0.0551032333888324,
2.8867264594883));
#25068=CARTESIAN_POINT('Ctrl Pts',(-0.0931239936920636,0.15643799622185,
2.88135165814895));
#25069=CARTESIAN_POINT('Ctrl Pts',(0.080081970475175,0.163498632518342,
2.87345442362313));
#25070=CARTESIAN_POINT('Ctrl Pts',(0.180683277203119,0.0223266252501708,
2.86555718909729));
#25071=CARTESIAN_POINT('Ctrl Pts',(0.11747183849698,-0.139087354145018,
2.85765995457145));
#25072=CARTESIAN_POINT('Ctrl Pts',(-0.0522430059551858,-0.174400668051551,
2.84976272004562));
#25073=CARTESIAN_POINT('Ctrl Pts',(-0.145618409602951,-0.0806790644135928,
2.84373567773551));
#25074=CARTESIAN_POINT('Ctrl Pts',(-0.154339055420526,-0.0149266411191706,
2.84034104693401));
#25075=CARTESIAN_POINT('Ctrl Pts',(-0.154217143654561,-0.000131209131675806,
2.83957882764113));
#25076=CARTESIAN_POINT('Origin',(0.,0.,3.71042117235887));
#25077=CARTESIAN_POINT('',(-0.154116825055928,9.48496454908493E-5,2.93957882764113));
#25078=CARTESIAN_POINT('',(-0.154366358871002,-0.000130096805920683,2.93542117235887));
#25079=CARTESIAN_POINT('',(-0.1543,1.43283619370552E-14,3.71042117235887));
#25080=CARTESIAN_POINT('Ctrl Pts',(-0.154366358871002,-0.000130096805920679,
2.93542117235887));
#25081=CARTESIAN_POINT('Ctrl Pts',(-0.153995797272422,0.0411865074797718,
2.93328738198899));
#25082=CARTESIAN_POINT('Ctrl Pts',(-0.115714146224304,0.134080683615333,
2.9285211801105));
#25083=CARTESIAN_POINT('Ctrl Pts',(0.0407990816336726,0.177427059877793,
2.9211225667234));
#25084=CARTESIAN_POINT('Ctrl Pts',(0.170870699467283,0.0628341523235889,
2.91322533219756));
#25085=CARTESIAN_POINT('Ctrl Pts',(0.146025941933673,-0.108726036068736,
2.90532809767173));
#25086=CARTESIAN_POINT('Ctrl Pts',(-0.0112102069433731,-0.181712019164164,
2.89743086314589));
#25087=CARTESIAN_POINT('Ctrl Pts',(-0.134787821110527,-0.104611252124613,
2.89079522137494));
#25088=CARTESIAN_POINT('Ctrl Pts',(-0.154028382735806,-0.026662535455284,
2.8867919911126));
#25089=CARTESIAN_POINT('Ctrl Pts',(-0.154054921884602,1.70237768407841E-5,
2.88542117235887));
#25090=CARTESIAN_POINT('Ctrl Pts',(-0.154116825055928,9.48496454908822E-5,
2.93957882764113));
#25091=CARTESIAN_POINT('Ctrl Pts',(-0.154225358468008,0.0191912107511692,
2.93859665170402));
#25092=CARTESIAN_POINT('Ctrl Pts',(-0.1421149984489,0.0893365787084054,
2.93498206425831));
#25093=CARTESIAN_POINT('Ctrl Pts',(-0.0376184643267171,0.178128537842515,
2.92873506530397));
#25094=CARTESIAN_POINT('Ctrl Pts',(0.128588348481182,0.128879639534425,
2.92083783077814));
#25095=CARTESIAN_POINT('Ctrl Pts',(0.178213202383553,-0.0372153106656781,
2.9129405962523));
#25096=CARTESIAN_POINT('Ctrl Pts',(0.0662647529343645,-0.169569771398652,
2.90504336172647));
#25097=CARTESIAN_POINT('Ctrl Pts',(-0.10336559476711,-0.148485092132862,
2.89725610552274));
#25098=CARTESIAN_POINT('Ctrl Pts',(-0.154372534171041,-0.0486635015632469,
2.89210126082763));
#25099=CARTESIAN_POINT('Ctrl Pts',(-0.154535784933253,3.8187773339879E-5,
2.88957882764113));
#25100=CARTESIAN_POINT('Origin',(0.,0.,3.71042117235887));
#25101=CARTESIAN_POINT('',(-0.154208836002914,-0.000129626704909153,2.98957882764113));
#25102=CARTESIAN_POINT('',(-0.154434696759477,0.000111004303427491,2.98542117235887));
#25103=CARTESIAN_POINT('',(-0.1543,1.43283619370552E-14,3.71042117235887));
#25104=CARTESIAN_POINT('Ctrl Pts',(-0.154434696759477,0.000111004303427509,
2.98542117235887));
#25105=CARTESIAN_POINT('Ctrl Pts',(-0.15449350107168,0.00733626390374423,
2.98504759588261));
#25106=CARTESIAN_POINT('Ctrl Pts',(-0.150762340620084,0.0654133961639385,
2.98204160789773));
#25107=CARTESIAN_POINT('Ctrl Pts',(-0.0771442428547834,0.164905101290741,
2.97640320840425));
#25108=CARTESIAN_POINT('Ctrl Pts',(0.0959076962473017,0.15474702077238,
2.96850597387841));
#25109=CARTESIAN_POINT('Ctrl Pts',(0.182006911912947,0.00429076371209153,
2.96060873935257));
#25110=CARTESIAN_POINT('Ctrl Pts',(0.103093336173269,-0.150055625266004,
2.95271150482674));
#25111=CARTESIAN_POINT('Ctrl Pts',(-0.069287674394006,-0.168357194128057,
2.9448142703009));
#25112=CARTESIAN_POINT('Ctrl Pts',(-0.14924717784082,-0.0703180680940833,
2.93905082614495));
#25113=CARTESIAN_POINT('Ctrl Pts',(-0.154452951185252,-0.00978490290509501,
2.9359197934976));
#25114=CARTESIAN_POINT('Ctrl Pts',(-0.154366358871002,-0.000130096805920679,
2.93542117235887));
#25115=CARTESIAN_POINT('Ctrl Pts',(-0.154208836002914,-0.00012962670490916,
2.98957882764113));
#25116=CARTESIAN_POINT('Ctrl Pts',(-0.15391701905173,0.0358705210125992,
2.98772445408903));
#25117=CARTESIAN_POINT('Ctrl Pts',(-0.123464382903156,0.123420397725162,
2.98323766902831));
#25118=CARTESIAN_POINT('Ctrl Pts',(0.0219177299165732,0.180733333857582,
2.97611847245899));
#25119=CARTESIAN_POINT('Ctrl Pts',(0.163317009898163,0.0804517192475515,
2.96822123793315));
#25120=CARTESIAN_POINT('Ctrl Pts',(0.156648310460303,-0.0927697778475837,
2.96032400340732));
#25121=CARTESIAN_POINT('Ctrl Pts',(0.00795766962277319,-0.181883480135435,
2.95242676888148));
#25122=CARTESIAN_POINT('Ctrl Pts',(-0.128557747147415,-0.11552191978543,
2.94551171029275));
#25123=CARTESIAN_POINT('Ctrl Pts',(-0.1539344690334,-0.0319905366812824,
2.94122906321263));
#25124=CARTESIAN_POINT('Ctrl Pts',(-0.154116825055928,9.48496454908822E-5,
2.93957882764113));
#25125=CARTESIAN_POINT('Origin',(0.,0.,3.71042117235887));
#25126=CARTESIAN_POINT('',(-0.154538871978598,3.2832780837988E-5,3.03957882764113));
#25127=CARTESIAN_POINT('',(-0.154056089165245,2.19184202627989E-5,3.03542117235887));
#25128=CARTESIAN_POINT('',(-0.1543,1.43283619370552E-14,3.71042117235887));
#25129=CARTESIAN_POINT('Ctrl Pts',(-0.154056089165245,2.19184202628134E-5,
3.03542117235887));
#25130=CARTESIAN_POINT('Ctrl Pts',(-0.154087155299894,0.0242673368387721,
3.03417539826761));
#25131=CARTESIAN_POINT('Ctrl Pts',(-0.137310014833352,0.0997044362362006,
3.03029721266774));
#25132=CARTESIAN_POINT('Ctrl Pts',(-0.0197606177252597,0.180981890321858,
3.02378661555926));
#25133=CARTESIAN_POINT('Ctrl Pts',(0.140740192743497,0.115486470133437,
3.01588938103343));
#25134=CARTESIAN_POINT('Ctrl Pts',(0.173641826766224,-0.0547123627222005,
3.00799214650759));
#25135=CARTESIAN_POINT('Ctrl Pts',(0.0491147003187017,-0.175307366787479,
3.00009491198175));
#25136=CARTESIAN_POINT('Ctrl Pts',(-0.11194410582055,-0.138777425062269,
2.99257125393218));
#25137=CARTESIAN_POINT('Ctrl Pts',(-0.15407913571938,-0.0435766220328422,
2.98768000739122));
#25138=CARTESIAN_POINT('Ctrl Pts',(-0.154434696759477,0.000111004303427509,
2.98542117235887));
#25139=CARTESIAN_POINT('Ctrl Pts',(-0.154538871978598,3.28327808380407E-5,
3.03957882764113));
#25140=CARTESIAN_POINT('Ctrl Pts',(-0.154544182685759,0.00185071603346938,
3.03948466798264));
#25141=CARTESIAN_POINT('Ctrl Pts',(-0.153694834634547,0.0544858891421056,
3.03675809681555));
#25142=CARTESIAN_POINT('Ctrl Pts',(-0.0940552495850459,0.15587987322763,
3.03139911413983));
#25143=CARTESIAN_POINT('Ctrl Pts',(0.0791055288760802,0.163973290975094,
3.02350187961401));
#25144=CARTESIAN_POINT('Ctrl Pts',(0.180546920428939,0.0234037256776295,
3.01560464508816));
#25145=CARTESIAN_POINT('Ctrl Pts',(0.118299191571216,-0.138384342053441,
3.00770741056233));
#25146=CARTESIAN_POINT('Ctrl Pts',(-0.0512020455023775,-0.174709116500372,
2.99981017603649));
#25147=CARTESIAN_POINT('Ctrl Pts',(-0.145381230907426,-0.0813015016053826,
2.99376731506276));
#25148=CARTESIAN_POINT('Ctrl Pts',(-0.154331273396456,-0.0152341784994835,
2.99035686559764));
#25149=CARTESIAN_POINT('Ctrl Pts',(-0.154208836002914,-0.00012962670490916,
2.98957882764113));
#25150=CARTESIAN_POINT('Origin',(0.,0.,3.71042117235887));
#25151=CARTESIAN_POINT('',(-0.154122750472518,9.83954699399631E-5,3.08957882764113));
#25152=CARTESIAN_POINT('',(-0.154357314101369,-0.000131672715837502,3.08542117235887));
#25153=CARTESIAN_POINT('',(-0.1543,1.43283619370552E-14,3.71042117235887));
#25154=CARTESIAN_POINT('Ctrl Pts',(-0.154357314101369,-0.000131672715837496,
3.08542117235887));
#25155=CARTESIAN_POINT('Ctrl Pts',(-0.153987553769485,0.0408848376338906,
3.08330320065262));
#25156=CARTESIAN_POINT('Ctrl Pts',(-0.11617759776856,0.133482913719063,
3.07855281743775));
#25157=CARTESIAN_POINT('Ctrl Pts',(0.039740276922879,0.17766720864428,3.07117002271427));
#25158=CARTESIAN_POINT('Ctrl Pts',(0.170492952144154,0.0638520156810144,
3.06327278818844));
#25159=CARTESIAN_POINT('Ctrl Pts',(0.146671728755708,-0.107853282848364,
3.0553755536626));
#25160=CARTESIAN_POINT('Ctrl Pts',(-0.0101263751692898,-0.181775639631079,
3.04747831913677));
#25161=CARTESIAN_POINT('Ctrl Pts',(-0.134457266065241,-0.105231153897523,
3.04082685870219));
#25162=CARTESIAN_POINT('Ctrl Pts',(-0.154021510291741,-0.026965000487735,
3.03680780977622));
#25163=CARTESIAN_POINT('Ctrl Pts',(-0.154056089165245,2.19184202628134E-5,
3.03542117235887));
#25164=CARTESIAN_POINT('Ctrl Pts',(-0.154122750472518,9.83954699399839E-5,
3.08957882764113));
#25165=CARTESIAN_POINT('Ctrl Pts',(-0.154233799032612,0.0188853799021587,
3.08861247036765));
#25166=CARTESIAN_POINT('Ctrl Pts',(-0.142381965748736,0.0887139061579003,
3.08501370158555));
#25167=CARTESIAN_POINT('Ctrl Pts',(-0.0386800578824722,0.177901034213339,
3.07878252129485));
#25168=CARTESIAN_POINT('Ctrl Pts',(0.127817493356429,0.129644179368171,
3.07088528676902));
#25169=CARTESIAN_POINT('Ctrl Pts',(0.178431965499368,-0.0361518815554529,
3.06298805224317));
#25170=CARTESIAN_POINT('Ctrl Pts',(0.0672747972491473,-0.169171588947593,
3.05509081771735));
#25171=CARTESIAN_POINT('Ctrl Pts',(-0.102823100152332,-0.149058093692613,
3.04728774284999));
#25172=CARTESIAN_POINT('Ctrl Pts',(-0.154395711813265,-0.0489716517674636,
3.04211707949126));
#25173=CARTESIAN_POINT('Ctrl Pts',(-0.154538871978598,3.28327808380407E-5,
3.03957882764113));
#25174=CARTESIAN_POINT('Origin',(0.,0.,3.71042117235887));
#25175=CARTESIAN_POINT('',(-0.154200664638475,-0.000127870236170058,3.13957882764113));
#25176=CARTESIAN_POINT('',(-0.154442743231392,0.000107782702043065,3.13542117235887));
#25177=CARTESIAN_POINT('',(-0.1543,1.43283619370552E-14,3.71042117235887));
#25178=CARTESIAN_POINT('Ctrl Pts',(-0.154442743231391,0.000107782702043087,
3.13542117235887));
#25179=CARTESIAN_POINT('Ctrl Pts',(-0.154497895338046,0.00702615569019676,
3.13506341454624));
#25180=CARTESIAN_POINT('Ctrl Pts',(-0.150944880930953,0.0647935208243374,
3.13207324522499));
#25181=CARTESIAN_POINT('Ctrl Pts',(-0.0781262761399388,0.164442122383114,
3.12645066439512));
#25182=CARTESIAN_POINT('Ctrl Pts',(0.0949831631341886,0.155316210867962,
3.11855342986929));
#25183=CARTESIAN_POINT('Ctrl Pts',(0.181978087741923,0.00537607841744088,
3.11065619534345));
#25184=CARTESIAN_POINT('Ctrl Pts',(0.10398635378076,-0.149438164016893,
3.10275896081762));
#25185=CARTESIAN_POINT('Ctrl Pts',(-0.0682824508977375,-0.168767394767933,
3.09486172629178));
#25186=CARTESIAN_POINT('Ctrl Pts',(-0.14904624696594,-0.0709390773474446,
3.0890824634722));
#25187=CARTESIAN_POINT('Ctrl Pts',(-0.154447126175577,-0.0100942824218163,
3.08593561216123));
#25188=CARTESIAN_POINT('Ctrl Pts',(-0.154357314101369,-0.000131672715837496,
3.08542117235887));
#25189=CARTESIAN_POINT('Ctrl Pts',(-0.154200664638475,-0.000127870236170063,
3.13957882764113));
#25190=CARTESIAN_POINT('Ctrl Pts',(-0.153916387321455,0.03556997377657,
3.13774027275265));
#25191=CARTESIAN_POINT('Ctrl Pts',(-0.123875930184563,0.122811200111113,
3.13326930635556));
#25192=CARTESIAN_POINT('Ctrl Pts',(0.0208395441149821,0.180860825645154,
3.12616592844986));
#25193=CARTESIAN_POINT('Ctrl Pts',(0.162834335224968,0.0814242232005321,
3.11826869392403));
#25194=CARTESIAN_POINT('Ctrl Pts',(0.157198753896076,-0.0918339622660831,
3.1103714593982));
#25195=CARTESIAN_POINT('Ctrl Pts',(0.00904218304404205,-0.181832790711041,
3.10247422487235));
#25196=CARTESIAN_POINT('Ctrl Pts',(-0.128179738775568,-0.116136573115574,
3.09554334762));
#25197=CARTESIAN_POINT('Ctrl Pts',(-0.153931296515552,-0.0322914212547928,
3.09124488187626));
#25198=CARTESIAN_POINT('Ctrl Pts',(-0.154122750472518,9.83954699399839E-5,
3.08957882764113));
#25199=CARTESIAN_POINT('Origin',(0.,0.,3.71042117235887));
#25200=CARTESIAN_POINT('',(-0.154541524340359,2.74150270591633E-5,3.18957882764113));
#25201=CARTESIAN_POINT('',(-0.154057549710717,2.67855146112065E-5,3.18542117235887));
#25202=CARTESIAN_POINT('',(-0.1543,1.43283619370552E-14,3.71042117235887));
#25203=CARTESIAN_POINT('Ctrl Pts',(-0.154057549710717,2.67855146112127E-5,
3.18542117235887));
#25204=CARTESIAN_POINT('Ctrl Pts',(-0.154095052553054,0.0239637717781011,
3.18419121693124));
#25205=CARTESIAN_POINT('Ctrl Pts',(-0.137617732079011,0.0990829983563936,
3.18032884999499));
#25206=CARTESIAN_POINT('Ctrl Pts',(-0.0208395446762738,0.180860830516292,
3.17383407155014));
#25207=CARTESIAN_POINT('Ctrl Pts',(0.140048991174337,0.116323715159066,
3.1659368370243));
#25208=CARTESIAN_POINT('Ctrl Pts',(0.173965014144346,-0.0536758837012937,
3.15803960249847));
#25209=CARTESIAN_POINT('Ctrl Pts',(0.050159265511441,-0.175011355976434,
3.15014236797263));
#25210=CARTESIAN_POINT('Ctrl Pts',(-0.111453603442084,-0.139367747346172,
3.14260289125943));
#25211=CARTESIAN_POINT('Ctrl Pts',(-0.154092081585972,-0.0438798036810342,
3.13769582605485));
#25212=CARTESIAN_POINT('Ctrl Pts',(-0.154442743231391,0.000107782702043087,
3.13542117235887));
#25213=CARTESIAN_POINT('Ctrl Pts',(-0.154541524340359,2.74150270592019E-5,
3.18957882764113));
#25214=CARTESIAN_POINT('Ctrl Pts',(-0.154545265409953,0.0015398273092893,
3.18950048664627));
#25215=CARTESIAN_POINT('Ctrl Pts',(-0.153842769766794,0.0538687068697594,
3.1867897341428));
#25216=CARTESIAN_POINT('Ctrl Pts',(-0.0949831605760139,0.155316206684809,
3.18144657013072));
#25217=CARTESIAN_POINT('Ctrl Pts',(0.0781262740357409,0.164442117954189,
3.17354933560488));
#25218=CARTESIAN_POINT('Ctrl Pts',(0.180404142828019,0.0244799939226929,
3.16565210107904));
#25219=CARTESIAN_POINT('Ctrl Pts',(0.119122337560023,-0.137676408822293,
3.15775486655321));
#25220=CARTESIAN_POINT('Ctrl Pts',(-0.0501592641604809,-0.175011351262844,
3.14985763202737));
#25221=CARTESIAN_POINT('Ctrl Pts',(-0.145141798308845,-0.081923988470417,
3.14379895239001));
#25222=CARTESIAN_POINT('Ctrl Pts',(-0.15432341073188,-0.0155415899851509,
3.14037268426126));
#25223=CARTESIAN_POINT('Ctrl Pts',(-0.154200664638475,-0.000127870236170063,
3.13957882764113));
#25224=CARTESIAN_POINT('Origin',(0.,0.,3.71042117235887));
#25225=CARTESIAN_POINT('',(-0.154128903346263,0.000101814369117867,3.23957882764113));
#25226=CARTESIAN_POINT('',(-0.15434822268538,-0.000133055250486845,3.23542117235887));
#25227=CARTESIAN_POINT('',(-0.1543,1.43283619370552E-14,3.71042117235887));
#25228=CARTESIAN_POINT('Ctrl Pts',(-0.15434822268538,-0.00013305525048684,
3.23542117235887));
#25229=CARTESIAN_POINT('Ctrl Pts',(-0.153979802923996,0.0405832940781535,
3.23331901931624));
#25230=CARTESIAN_POINT('Ctrl Pts',(-0.116638046803031,0.132884381239301,
3.228584454765));
#25231=CARTESIAN_POINT('Ctrl Pts',(0.0386800589242284,0.177901039004767,
3.22121747870515));
#25232=CARTESIAN_POINT('Ctrl Pts',(0.170109141545278,0.0648676082500797,
3.21332024417931));
#25233=CARTESIAN_POINT('Ctrl Pts',(0.147312299474883,-0.106976694007524,
3.20542300965349));
#25234=CARTESIAN_POINT('Ctrl Pts',(-0.00904218328755787,-0.18183279560836,
3.19752577512764));
#25235=CARTESIAN_POINT('Ctrl Pts',(-0.134124100441736,-0.105850839905797,
3.19085849602944));
#25236=CARTESIAN_POINT('Ctrl Pts',(-0.154014787112897,-0.0272673514852388,
3.18682362843985));
#25237=CARTESIAN_POINT('Ctrl Pts',(-0.154057549710717,2.67855146112127E-5,
3.18542117235887));
#25238=CARTESIAN_POINT('Ctrl Pts',(-0.154128903346263,0.000101814369117853,
3.23957882764113));
#25239=CARTESIAN_POINT('Ctrl Pts',(-0.15424221981892,0.0185794122284465,
3.23862828903127));
#25240=CARTESIAN_POINT('Ctrl Pts',(-0.142646569905461,0.0880912185498955,
3.23504533891281));
#25241=CARTESIAN_POINT('Ctrl Pts',(-0.0397402758525677,0.177667203859151,
3.22882997728572));
#25242=CARTESIAN_POINT('Ctrl Pts',(0.127042092635782,0.130404108641901,
3.22093274275989));
#25243=CARTESIAN_POINT('Ctrl Pts',(0.178644383007786,-0.0350871667669908,
3.21303550823405));
#25244=CARTESIAN_POINT('Ctrl Pts',(0.0682824490586963,-0.1687673902225,
3.20513827370822));
#25245=CARTESIAN_POINT('Ctrl Pts',(-0.102277435139451,-0.149629907004419,
3.19731938017724));
#25246=CARTESIAN_POINT('Ctrl Pts',(-0.154419558113643,-0.0492801999911546,
3.19213289815488));
#25247=CARTESIAN_POINT('Ctrl Pts',(-0.154541524340359,2.74150270592019E-5,
3.18957882764113));
#25248=CARTESIAN_POINT('Origin',(0.,0.,3.71042117235887));
#25249=CARTESIAN_POINT('',(-0.154192638571573,-0.000125942848695916,3.28957882764113));
#25250=CARTESIAN_POINT('',(-0.154450609193756,0.000104390085258889,3.28542117235887));
#25251=CARTESIAN_POINT('',(-0.1543,1.43283619370552E-14,3.71042117235887));
#25252=CARTESIAN_POINT('Ctrl Pts',(-0.154450609193756,0.000104390085258887,
3.28542117235887));
#25253=CARTESIAN_POINT('Ctrl Pts',(-0.154502116257734,0.0067159788236037,
3.28507923320986));
#25254=CARTESIAN_POINT('Ctrl Pts',(-0.151125396911172,0.064173784678776,
3.28210488255223));
#25255=CARTESIAN_POINT('Ctrl Pts',(-0.0791055310066521,0.163973295391393,
3.27649812038601));
#25256=CARTESIAN_POINT('Ctrl Pts',(0.0940552521182287,0.155879877425964,
3.26860088586016));
#25257=CARTESIAN_POINT('Ctrl Pts',(0.181942791852133,0.00646120193221371,
3.26070365133433));
#25258=CARTESIAN_POINT('Ctrl Pts',(0.104875673303493,-0.148815388271832,
3.25280641680849));
#25259=CARTESIAN_POINT('Ctrl Pts',(-0.067274799061048,-0.169171593503912,
3.24490918228266));
#25260=CARTESIAN_POINT('Ctrl Pts',(-0.148843209204449,-0.0715602003700874,
3.23911410079945));
#25261=CARTESIAN_POINT('Ctrl Pts',(-0.154441154880871,-0.0104035676716175,
3.23595143082485));
#25262=CARTESIAN_POINT('Ctrl Pts',(-0.15434822268538,-0.00013305525048684,
3.23542117235887));
#25263=CARTESIAN_POINT('Ctrl Pts',(-0.154192638571573,-0.000125942848695916,
3.28957882764113));
#25264=CARTESIAN_POINT('Ctrl Pts',(-0.153916116413885,0.0352694274746551,
3.28775609141628));
#25265=CARTESIAN_POINT('Ctrl Pts',(-0.124284613860796,0.122201478629219,
3.28330094368282));
#25266=CARTESIAN_POINT('Ctrl Pts',(0.0197606171930289,0.18098188544746,
3.27621338444074));
#25267=CARTESIAN_POINT('Ctrl Pts',(0.162345869645737,0.0823938314495476,
3.26831614991491));
#25268=CARTESIAN_POINT('Ctrl Pts',(0.157743606844976,-0.0908948807772195,
3.26041891538907));
#25269=CARTESIAN_POINT('Ctrl Pts',(0.0101263748965706,-0.181775634735301,
3.25252168086324));
#25270=CARTESIAN_POINT('Ctrl Pts',(-0.127798960265965,-0.1167508316284,
3.24557498494725));
#25271=CARTESIAN_POINT('Ctrl Pts',(-0.153928402385683,-0.0325922506078629,
3.24126070053988));
#25272=CARTESIAN_POINT('Ctrl Pts',(-0.154128903346263,0.000101814369117853,
3.23957882764113));
#25273=CARTESIAN_POINT('Origin',(0.,0.,3.71042117235887));
#25274=CARTESIAN_POINT('',(-0.154543726005254,2.19441315424396E-5,3.33957882764113));
#25275=CARTESIAN_POINT('',(-0.154059302102979,3.16189515402649E-5,3.33542117235887));
#25276=CARTESIAN_POINT('',(-0.1543,1.43283619370552E-14,3.71042117235887));
#25277=CARTESIAN_POINT('Ctrl Pts',(-0.154059302102979,3.16189515402656E-5,
3.33542117235887));
#25278=CARTESIAN_POINT('Ctrl Pts',(-0.15410303154311,0.0236600756904899,
3.33420703559487));
#25279=CARTESIAN_POINT('Ctrl Pts',(-0.137922930779561,0.0984614290803482,
3.33036048732225));
#25280=CARTESIAN_POINT('Ctrl Pts',(-0.0219177305069036,0.180733338725286,
3.32388152754101));
#25281=CARTESIAN_POINT('Ctrl Pts',(0.139352809018331,0.117156823343995,
3.31598429301518));
#25282=CARTESIAN_POINT('Ctrl Pts',(0.174282014774141,-0.0526374957955154,
3.30808705848934));
#25283=CARTESIAN_POINT('Ctrl Pts',(0.0512020468814229,-0.174709121205821,
3.3001898239635));
#25284=CARTESIAN_POINT('Ctrl Pts',(-0.110960029365619,-0.139957157472604,
3.29263452858669));
#25285=CARTESIAN_POINT('Ctrl Pts',(-0.154105590184654,-0.0441832011483282,
3.28771164471847));
#25286=CARTESIAN_POINT('Ctrl Pts',(-0.154450609193756,0.000104390085258887,
3.28542117235887));
#25287=CARTESIAN_POINT('Ctrl Pts',(-0.154543726005254,2.19441315424298E-5,
3.33957882764113));
#25288=CARTESIAN_POINT('Ctrl Pts',(-0.154546150302478,0.00122892294348618,
3.33951630530989));
#25289=CARTESIAN_POINT('Ctrl Pts',(-0.153988815888461,0.0532516871969489,
3.33682137147005));
#25290=CARTESIAN_POINT('Ctrl Pts',(-0.0959076936642258,0.154747016604558,
3.33149402612159));
#25291=CARTESIAN_POINT('Ctrl Pts',(0.0771442407770374,0.164905096849345,
3.32359679159575));
#25292=CARTESIAN_POINT('Ctrl Pts',(0.180254949482897,0.0255553915814562,
3.31569955706992));
#25293=CARTESIAN_POINT('Ctrl Pts',(0.119941247180243,-0.13696357938087,
3.30780232254408));
#25294=CARTESIAN_POINT('Ctrl Pts',(-0.0491146989958762,-0.175307362065916,
3.29990508801825));
#25295=CARTESIAN_POINT('Ctrl Pts',(-0.144900102757682,-0.0825465196247692,
3.29383058971726));
#25296=CARTESIAN_POINT('Ctrl Pts',(-0.154315472118983,-0.0158488741865795,
3.29038850292489));
#25297=CARTESIAN_POINT('Ctrl Pts',(-0.154192638571573,-0.000125942848695916,
3.28957882764113));
#25298=CARTESIAN_POINT('Origin',(0.,0.,3.71042117235887));
#25299=CARTESIAN_POINT('',(-0.15413527741405,0.000105101588974824,3.38957882764113));
#25300=CARTESIAN_POINT('',(-0.15433909720242,-0.000134243687139869,3.38542117235887));
#25301=CARTESIAN_POINT('',(-0.1543,1.43283619370552E-14,3.71042117235887));
#25302=CARTESIAN_POINT('Ctrl Pts',(-0.15433909720242,-0.000134243687139867,
3.38542117235887));
#25303=CARTESIAN_POINT('Ctrl Pts',(-0.153972537455045,0.0402818685502336,
3.38333483797987));
#25304=CARTESIAN_POINT('Ctrl Pts',(-0.117095500692927,0.132285100657941,
3.37861609209226));
#25305=CARTESIAN_POINT('Ctrl Pts',(0.0376184653398806,0.178128542640067,
3.37126493469602));
#25306=CARTESIAN_POINT('Ctrl Pts',(0.169719281325138,0.0658808939206553,
3.36336770017019));
#25307=CARTESIAN_POINT('Ctrl Pts',(0.14794763130091,-0.10609630073556,3.35547046564435));
#25308=CARTESIAN_POINT('Ctrl Pts',(-0.00795766983708003,-0.181883485034118,
3.34757323111852));
#25309=CARTESIAN_POINT('Ctrl Pts',(-0.133788315045723,-0.106470301039161,
3.34089013335669));
#25310=CARTESIAN_POINT('Ctrl Pts',(-0.154008220246,-0.0275695907640756,
3.33683944710348));
#25311=CARTESIAN_POINT('Ctrl Pts',(-0.154059302102979,3.16189515402656E-5,
3.33542117235887));
#25312=CARTESIAN_POINT('Ctrl Pts',(-0.15413527741405,0.000105101588974825,
3.38957882764113));
#25313=CARTESIAN_POINT('Ctrl Pts',(-0.154250615308729,0.0182733082008614,
3.3886441076949));
#25314=CARTESIAN_POINT('Ctrl Pts',(-0.142908820182152,0.0874685218643051,
3.38507697624006));
#25315=CARTESIAN_POINT('Ctrl Pts',(-0.0407990805348497,0.177427055099143,
3.3788774332766));
#25316=CARTESIAN_POINT('Ctrl Pts',(0.126262173896246,0.131159400329288,
3.37098019875077));
#25317=CARTESIAN_POINT('Ctrl Pts',(0.178850447353964,-0.0340212041663437,
3.36308296422493));
#25318=CARTESIAN_POINT('Ctrl Pts',(0.0692876725278909,-0.168357189593675,
3.3551857296991));
#25319=CARTESIAN_POINT('Ctrl Pts',(-0.101728594599068,-0.150200514568663,
3.3473510175045));
#25320=CARTESIAN_POINT('Ctrl Pts',(-0.15444407880598,-0.0495891584122831,
3.3421487168185));
#25321=CARTESIAN_POINT('Ctrl Pts',(-0.154543726005254,2.19441315424298E-5,
3.33957882764113));
#25322=CARTESIAN_POINT('Origin',(0.,0.,3.71042117235887));
#25323=CARTESIAN_POINT('',(-0.154184766718537,-0.000123847547745311,3.43957882764113));
#25324=CARTESIAN_POINT('',(-0.154458280286029,0.000100830356962909,3.43542117235887));
#25325=CARTESIAN_POINT('',(-0.1543,1.43283619370552E-14,3.71042117235887));
#25326=CARTESIAN_POINT('Ctrl Pts',(-0.154458280286029,0.000100830356962935,
3.43542117235887));
#25327=CARTESIAN_POINT('Ctrl Pts',(-0.154506161619621,0.00640573612334919,
3.43509505187348));
#25328=CARTESIAN_POINT('Ctrl Pts',(-0.151303896650316,0.0635541898545394,
3.43213651987949));
#25329=CARTESIAN_POINT('Ctrl Pts',(-0.0800819726320239,0.163498636922,3.42654557637688));
#25330=CARTESIAN_POINT('Ctrl Pts',(0.0931239962001525,0.156438000435139,
3.41864834185104));
#25331=CARTESIAN_POINT('Ctrl Pts',(0.181901025498224,0.00754609564814438,
3.41075110732521));
#25332=CARTESIAN_POINT('Ctrl Pts',(0.10576126311461,-0.148187320169658,
3.40285387279937));
#25333=CARTESIAN_POINT('Ctrl Pts',(-0.0662647547190597,-0.169569775965683,
3.39495663827354));
#25334=CARTESIAN_POINT('Ctrl Pts',(-0.148638055997427,-0.0721814340714305,
3.3891457381267));
#25335=CARTESIAN_POINT('Ctrl Pts',(-0.154435040545295,-0.0107127563084332,
3.38596724948848));
#25336=CARTESIAN_POINT('Ctrl Pts',(-0.15433909720242,-0.000134243687139867,
3.38542117235887));
#25337=CARTESIAN_POINT('Ctrl Pts',(-0.154184766718538,-0.000123847547745311,
3.43957882764113));
#25338=CARTESIAN_POINT('Ctrl Pts',(-0.153916198856604,0.0349688764624186,
3.4377719100799));
#25339=CARTESIAN_POINT('Ctrl Pts',(-0.124690442079412,0.121591245361209,
3.43333258101007));
#25340=CARTESIAN_POINT('Ctrl Pts',(0.0186809873893989,0.181096509168673,
3.42626084043161));
#25341=CARTESIAN_POINT('Ctrl Pts',(0.161851630600137,0.0833605094034181,
3.41836360590578));
#25342=CARTESIAN_POINT('Ctrl Pts',(0.158282849894819,-0.0899525667211824,
3.41046637137994));
#25343=CARTESIAN_POINT('Ctrl Pts',(0.0112102066414966,-0.181712014270169,
3.40256913685411));
#25344=CARTESIAN_POINT('Ctrl Pts',(-0.127415402859048,-0.117364684067358,
3.3956066222745));
#25345=CARTESIAN_POINT('Ctrl Pts',(-0.153925794165715,-0.032893029234098,
3.39127651920351));
#25346=CARTESIAN_POINT('Ctrl Pts',(-0.15413527741405,0.000105101588974825,
3.38957882764113));
#25347=CARTESIAN_POINT('Origin',(0.,0.,3.71042117235887));
#25348=CARTESIAN_POINT('',(-0.154545466983052,1.64397697926255E-5,3.48957882764113));
#25349=CARTESIAN_POINT('',(-0.154061344734167,3.6410572125671E-5,3.48542117235887));
#25350=CARTESIAN_POINT('',(-0.1543,1.43283619370552E-14,3.71042117235887));
#25351=CARTESIAN_POINT('Ctrl Pts',(-0.154061344734167,3.64105721256669E-5,
3.48542117235887));
#25352=CARTESIAN_POINT('Ctrl Pts',(-0.154111085743468,0.0233562467547802,
3.48422285425849));
#25353=CARTESIAN_POINT('Ctrl Pts',(-0.13822562008929,0.0978397409961887,
3.48039212464949));
#25354=CARTESIAN_POINT('Ctrl Pts',(-0.0229951370022999,0.180599416102118,
3.47392898353189));
#25355=CARTESIAN_POINT('Ctrl Pts',(0.138651671100891,0.117985766817156,
3.46603174900605));
#25356=CARTESIAN_POINT('Ctrl Pts',(0.174592817347261,-0.0515972368462645,
3.45813451448022));
#25357=CARTESIAN_POINT('Ctrl Pts',(0.0522430073621133,-0.174400672749591,
3.45023727995438));
#25358=CARTESIAN_POINT('Ctrl Pts',(-0.110463377019167,-0.140545639944236,
3.44266616591394));
#25359=CARTESIAN_POINT('Ctrl Pts',(-0.15411966834722,-0.0444868242763973,
3.4377274633821));
#25360=CARTESIAN_POINT('Ctrl Pts',(-0.154458280286029,0.000100830356962935,
3.43542117235887));
#25361=CARTESIAN_POINT('Ctrl Pts',(-0.154545466983052,1.64397697926493E-5,
3.48957882764113));
#25362=CARTESIAN_POINT('Ctrl Pts',(-0.154546843102601,0.000918015954509084,
3.48953212397352));
#25363=CARTESIAN_POINT('Ctrl Pts',(-0.154132992535152,0.0526348504359433,
3.4868530087973));
#25364=CARTESIAN_POINT('Ctrl Pts',(-0.0968288031440013,0.15417230277993,
3.48154148211247));
#25365=CARTESIAN_POINT('Ctrl Pts',(0.0761594573579975,0.165362221823523,
3.47364424758663));
#25366=CARTESIAN_POINT('Ctrl Pts',(0.180099349163956,0.0266298748857393,
3.46574701306079));
#25367=CARTESIAN_POINT('Ctrl Pts',(0.120755889508211,-0.136245876208876,
3.45784977853496));
#25368=CARTESIAN_POINT('Ctrl Pts',(-0.0480683862207756,-0.175597139874519,
3.44995254400912));
#25369=CARTESIAN_POINT('Ctrl Pts',(-0.144656135320296,-0.0831690899066176,
3.44386222704451));
#25370=CARTESIAN_POINT('Ctrl Pts',(-0.154307462490191,-0.0161560295849065,
3.44040432158851));
#25371=CARTESIAN_POINT('Ctrl Pts',(-0.154184766718538,-0.000123847547745311,
3.43957882764113));
#25372=CARTESIAN_POINT('Origin',(0.,0.,3.71042117235887));
#25373=CARTESIAN_POINT('',(-0.154141660315178,0.000107924336747972,3.53957882764113));
#25374=CARTESIAN_POINT('',(-0.154329957770701,-0.000135440264844456,3.53542117235887));
#25375=CARTESIAN_POINT('',(-0.1543,1.43283619370552E-14,3.71042117235887));
#25376=CARTESIAN_POINT('Ctrl Pts',(-0.154329957770701,-0.000135440264844458,
3.53542117235887));
#25377=CARTESIAN_POINT('Ctrl Pts',(-0.153965757190248,0.0399803656323286,
3.5333506566435));
#25378=CARTESIAN_POINT('Ctrl Pts',(-0.117549955642843,0.13168538088825,
3.52864772941951));
#25379=CARTESIAN_POINT('Ctrl Pts',(0.0365555273815534,0.178349539831362,
3.52131239068689));
#25380=CARTESIAN_POINT('Ctrl Pts',(0.169323388748115,0.0668919258489962,
3.51341515616108));
#25381=CARTESIAN_POINT('Ctrl Pts',(0.148577699872602,-0.105212180693424,
3.50551792163523));
#25382=CARTESIAN_POINT('Ctrl Pts',(-0.00687287246844015,-0.181927682017732,
3.4976206871094));
#25383=CARTESIAN_POINT('Ctrl Pts',(-0.133449900938225,-0.107089534990244,
3.49092177068394));
#25384=CARTESIAN_POINT('Ctrl Pts',(-0.154001816923033,-0.0278717244546827,
3.4868552657671));
#25385=CARTESIAN_POINT('Ctrl Pts',(-0.154061344734167,3.64105721256669E-5,
3.48542117235887));
#25386=CARTESIAN_POINT('Ctrl Pts',(-0.154141660315178,0.000107924336747963,
3.53957882764113));
#25387=CARTESIAN_POINT('Ctrl Pts',(-0.154258987201045,0.017967079764623,
3.53865992635852));
#25388=CARTESIAN_POINT('Ctrl Pts',(-0.14316956514131,0.0868471600938436,
3.53510861356731));
#25389=CARTESIAN_POINT('Ctrl Pts',(-0.0418557834629445,0.177179558878914,
3.52892488926748));
#25390=CARTESIAN_POINT('Ctrl Pts',(0.125477426630257,0.13191056683484,3.52102765474164));
#25391=CARTESIAN_POINT('Ctrl Pts',(0.179050327003836,-0.0329543119327003,
3.51313042021581));
#25392=CARTESIAN_POINT('Ctrl Pts',(0.0702903405429243,-0.167940855985405,
3.50523318568997));
#25393=CARTESIAN_POINT('Ctrl Pts',(-0.101176526834898,-0.15076997316947,
3.49738265483174));
#25394=CARTESIAN_POINT('Ctrl Pts',(-0.154469279323916,-0.0498985397050101,
3.49216453548213));
#25395=CARTESIAN_POINT('Ctrl Pts',(-0.154545466983052,1.64397697926493E-5,
3.48957882764113));
#25396=CARTESIAN_POINT('Origin',(0.,0.,3.71042117235887));
#25397=CARTESIAN_POINT('',(-0.154140927489633,-0.000180264065019253,3.58957882764113));
#25398=CARTESIAN_POINT('',(-0.15446591465964,9.2330361050462E-5,3.58542117235887));
#25399=CARTESIAN_POINT('',(-0.1543,1.43283619370552E-14,3.71042117235887));
#25400=CARTESIAN_POINT('',(-0.0398513841857247,-0.149064942821851,3.6));
#25401=CARTESIAN_POINT('Ctrl Pts',(-0.0398513841857247,-0.149064942821851,
3.6));
#25402=CARTESIAN_POINT('Ctrl Pts',(-0.0891618565331957,-0.135882161272422,
3.59736758849139));
#25403=CARTESIAN_POINT('Ctrl Pts',(-0.14437796139003,-0.0838321271698221,
3.59389386437176));
#25404=CARTESIAN_POINT('Ctrl Pts',(-0.154259564981832,-0.0165262407662603,
3.59042014025214));
#25405=CARTESIAN_POINT('Ctrl Pts',(-0.154140927489633,-0.000180264065019272,
3.58957882764113));
#25406=CARTESIAN_POINT('',(0.0399440158046003,-0.149318575284508,3.6));
#25407=CARTESIAN_POINT('Origin',(0.,0.,3.6));
#25408=CARTESIAN_POINT('Ctrl Pts',(0.0399441988940755,-0.14931907659749,
3.6));
#25409=CARTESIAN_POINT('Ctrl Pts',(-0.00742263582378978,-0.161856507480607,
3.59746250047314));
#25410=CARTESIAN_POINT('Ctrl Pts',(-0.110807703402812,-0.13923343552822,
3.59260289125943));
#25411=CARTESIAN_POINT('Ctrl Pts',(-0.154134073844742,-0.0447846479172299,
3.58774328204572));
#25412=CARTESIAN_POINT('Ctrl Pts',(-0.15446591465964,9.23303610504333E-5,
3.58542117235887));
#25413=CARTESIAN_POINT('Origin',(-1.70916393953233E-17,-6.81365885416763E-18,
2.7));
#25414=CARTESIAN_POINT('Ctrl Pts',(-0.0958116152722464,0.0825211298936403,
2.7));
#25415=CARTESIAN_POINT('Ctrl Pts',(-0.100666302508711,0.0779874972024075,
2.7));
#25416=CARTESIAN_POINT('Ctrl Pts',(-0.10511524090547,0.0730607151536329,
2.7));
#25417=CARTESIAN_POINT('Ctrl Pts',(-0.109154515912936,0.0678088625732328,
2.7));
#25418=CARTESIAN_POINT('Ctrl Pts',(-0.111628556611506,0.0645921226872924,
2.7));
#25419=CARTESIAN_POINT('Ctrl Pts',(-0.113949938179476,0.0612512837881844,
2.7));
#25420=CARTESIAN_POINT('Ctrl Pts',(-0.116112529388643,0.0578058814506189,
2.7));
#25421=CARTESIAN_POINT('Ctrl Pts',(-0.120278296492253,0.0511690544554421,
2.7));
#25422=CARTESIAN_POINT('Ctrl Pts',(-0.123843133570631,0.0441670378484578,
2.7));
#25423=CARTESIAN_POINT('Ctrl Pts',(-0.126794163478656,0.0368991818833284,
2.7));
#25424=CARTESIAN_POINT('Ctrl Pts',(-0.128540684647383,0.0325978143303114,
2.7));
#25425=CARTESIAN_POINT('Ctrl Pts',(-0.130072629552482,0.0281986906446855,
2.7));
#25426=CARTESIAN_POINT('Ctrl Pts',(-0.13137784724267,0.0237479033105473,
2.7));
#25427=CARTESIAN_POINT('Ctrl Pts',(-0.134168070532741,0.0142332525574809,
2.7));
#25428=CARTESIAN_POINT('Ctrl Pts',(-0.135935427906691,0.00446386180413974,
2.7));
#25429=CARTESIAN_POINT('Ctrl Pts',(-0.136643098733652,-0.00537896296213896,
2.7));
#25430=CARTESIAN_POINT('Ctrl Pts',(-0.136956933956429,-0.00974402223206864,
2.7));
#25431=CARTESIAN_POINT('Ctrl Pts',(-0.137061776691848,-0.0141238933117977,
2.7));
#25432=CARTESIAN_POINT('Ctrl Pts',(-0.136951314304003,-0.0185038366743994,
2.7));
#25433=CARTESIAN_POINT('Ctrl Pts',(-0.136873618225507,-0.0215845633357163,
2.7));
#25434=CARTESIAN_POINT('Ctrl Pts',(-0.13668911286562,-0.0246638039330577,
2.7));
#25435=CARTESIAN_POINT('Ctrl Pts',(-0.136397287648127,-0.0277243541204411,
2.7));
#25436=CARTESIAN_POINT('Ctrl Pts',(-0.136038403631432,-0.031488191097877,
2.7));
#25437=CARTESIAN_POINT('Ctrl Pts',(-0.135517191903042,-0.0352286565107813,
2.7));
#25438=CARTESIAN_POINT('Ctrl Pts',(-0.134831588718299,-0.0389361603135121,
2.7));
#25439=CARTESIAN_POINT('Ctrl Pts',(-0.133471069242182,-0.0462933769129071,
2.7));
#25440=CARTESIAN_POINT('Ctrl Pts',(-0.131464409754198,-0.0535208830833808,
2.7));
#25441=CARTESIAN_POINT('Ctrl Pts',(-0.128873836850864,-0.0605679807942907,
2.7));
#25442=CARTESIAN_POINT('Ctrl Pts',(-0.127324936193114,-0.064781432678084,
2.7));
#25443=CARTESIAN_POINT('Ctrl Pts',(-0.125566934259419,-0.0689304108686299,
2.7));
#25444=CARTESIAN_POINT('Ctrl Pts',(-0.123610254975486,-0.0730036509543968,
2.7));
#25445=CARTESIAN_POINT('Ctrl Pts',(-0.122225010943685,-0.0758873281953399,
2.7));
#25446=CARTESIAN_POINT('Ctrl Pts',(-0.120744058613202,-0.0787247786003408,
2.7));
#25447=CARTESIAN_POINT('Ctrl Pts',(-0.11917349881759,-0.0815104554030709,
2.7));
#25448=CARTESIAN_POINT('Ctrl Pts',(-0.115042560220701,-0.0888374351557691,
2.7));
#25449=CARTESIAN_POINT('Ctrl Pts',(-0.11029123440495,-0.095810889712998,
2.7));
#25450=CARTESIAN_POINT('Ctrl Pts',(-0.104997440961948,-0.102362839712403,
2.7));
#25451=CARTESIAN_POINT('Ctrl Pts',(-0.101348653506344,-0.106878821158406,
2.7));
#25452=CARTESIAN_POINT('Ctrl Pts',(-0.0974416313653614,-0.11119454456931,
2.7));
#25453=CARTESIAN_POINT('Ctrl Pts',(-0.09329635857045,-0.115285413781573,
2.7));
#25454=CARTESIAN_POINT('Ctrl Pts',(-0.0904535089763086,-0.118090953116413,
2.7));
#25455=CARTESIAN_POINT('Ctrl Pts',(-0.0874964288334564,-0.12079189694507,
2.7));
#25456=CARTESIAN_POINT('Ctrl Pts',(-0.0844493327259437,-0.123365242468763,
2.7));
#25457=CARTESIAN_POINT('Ctrl Pts',(-0.0762097423121146,-0.130323773594913,
2.7));
#25458=CARTESIAN_POINT('Ctrl Pts',(-0.0672905965515622,-0.136377649112853,
2.7));
#25459=CARTESIAN_POINT('Ctrl Pts',(-0.0578267373609757,-0.141381851878944,
2.7));
#25460=CARTESIAN_POINT('Ctrl Pts',(-0.0536817029967175,-0.143573620798307,
2.7));
#25461=CARTESIAN_POINT('Ctrl Pts',(-0.0494316342727489,-0.145563646977507,
2.7));
#25462=CARTESIAN_POINT('Ctrl Pts',(-0.0450857388735961,-0.147337358046063,
2.7));
#25463=CARTESIAN_POINT('Ctrl Pts',(-0.043386269574786,-0.148030970576765,
2.7));
#25464=CARTESIAN_POINT('Ctrl Pts',(-0.0416721350945774,-0.148691483593437,
2.7));
#25465=CARTESIAN_POINT('Ctrl Pts',(-0.0399441884684126,-0.149319082708151,
2.7));
#25466=CARTESIAN_POINT('Ctrl Pts',(0.0398513841857358,-0.149064942821848,
2.7));
#25467=CARTESIAN_POINT('Ctrl Pts',(0.0462200530662091,-0.146737857425647,
2.7));
#25468=CARTESIAN_POINT('Ctrl Pts',(0.0524055534681357,-0.143963403134301,
2.7));
#25469=CARTESIAN_POINT('Ctrl Pts',(0.0583783483111506,-0.140779078044469,
2.7));
#25470=CARTESIAN_POINT('Ctrl Pts',(0.062793202477668,-0.138425350642158,
2.7));
#25471=CARTESIAN_POINT('Ctrl Pts',(0.067091772966825,-0.135847508755531,
2.7));
#25472=CARTESIAN_POINT('Ctrl Pts',(0.0712602009478766,-0.133058650089746,
2.7));
#25473=CARTESIAN_POINT('Ctrl Pts',(0.0751200675142575,-0.130476232360243,
2.7));
#25474=CARTESIAN_POINT('Ctrl Pts',(0.078861342939135,-0.127717307612303,
2.7));
#25475=CARTESIAN_POINT('Ctrl Pts',(0.0824683178131891,-0.124797523957272,
2.7));
#25476=CARTESIAN_POINT('Ctrl Pts',(0.0880430571667216,-0.12028486905563,
2.7));
#25477=CARTESIAN_POINT('Ctrl Pts',(0.093301870580488,-0.115385246850429,
2.7));
#25478=CARTESIAN_POINT('Ctrl Pts',(0.098201122907525,-0.11013722292202,
2.7));
#25479=CARTESIAN_POINT('Ctrl Pts',(0.100467267721939,-0.107709754113023,
2.7));
#25480=CARTESIAN_POINT('Ctrl Pts',(0.102654039344122,-0.10520989028497,
2.7));
#25481=CARTESIAN_POINT('Ctrl Pts',(0.104752062819345,-0.102648267464436,
2.7));
#25482=CARTESIAN_POINT('Ctrl Pts',(0.111288676944248,-0.0946672605266598,
2.7));
#25483=CARTESIAN_POINT('Ctrl Pts',(0.11698432795861,-0.0860702972477514,
2.7));
#25484=CARTESIAN_POINT('Ctrl Pts',(0.121705201609602,-0.0769745632194894,
2.7));
#25485=CARTESIAN_POINT('Ctrl Pts',(0.12379312017453,-0.0729517586830322,
2.7));
#25486=CARTESIAN_POINT('Ctrl Pts',(0.125689731189231,-0.0688311600363216,
2.7));
#25487=CARTESIAN_POINT('Ctrl Pts',(0.127380076370131,-0.0646223264534606,
2.7));
#25488=CARTESIAN_POINT('Ctrl Pts',(0.128615050131834,-0.0615473337827676,
2.7));
#25489=CARTESIAN_POINT('Ctrl Pts',(0.129739752069541,-0.0584245102417657,
2.7));
#25490=CARTESIAN_POINT('Ctrl Pts',(0.130743760465559,-0.0552728510655911,
2.7));
#25491=CARTESIAN_POINT('Ctrl Pts',(0.131931576408969,-0.0515442059342363,
2.7));
#25492=CARTESIAN_POINT('Ctrl Pts',(0.132952645794869,-0.0477702728539015,
2.7));
#25493=CARTESIAN_POINT('Ctrl Pts',(0.13379905511372,-0.0439575955102323,
2.7));
#25494=CARTESIAN_POINT('Ctrl Pts',(0.135238114697535,-0.0374753064460584,
2.7));
#25495=CARTESIAN_POINT('Ctrl Pts',(0.136172820012768,-0.0308808878255892,
2.7));
#25496=CARTESIAN_POINT('Ctrl Pts',(0.136617245503396,-0.0242291498972301,
2.7));
#25497=CARTESIAN_POINT('Ctrl Pts',(0.136949796542121,-0.0192518423303904,
2.7));
#25498=CARTESIAN_POINT('Ctrl Pts',(0.13700760567975,-0.0142424066500717,
2.7));
#25499=CARTESIAN_POINT('Ctrl Pts',(0.136793131026844,-0.00922497436481165,
2.7));
#25500=CARTESIAN_POINT('Ctrl Pts',(0.136645101058571,-0.00576195282855203,
2.7));
#25501=CARTESIAN_POINT('Ctrl Pts',(0.1363675285007,-0.00230375513318918,
2.7));
#25502=CARTESIAN_POINT('Ctrl Pts',(0.13596351343207,0.00113554936727295,
2.7));
#25503=CARTESIAN_POINT('Ctrl Pts',(0.13510375104742,0.00845454528710606,
2.7));
#25504=CARTESIAN_POINT('Ctrl Pts',(0.133671961121794,0.0156977511556185,
2.7));
#25505=CARTESIAN_POINT('Ctrl Pts',(0.131684102868306,0.0227886248739312,
2.7));
#25506=CARTESIAN_POINT('Ctrl Pts',(0.130343128964387,0.0275720024591066,
2.7));
#25507=CARTESIAN_POINT('Ctrl Pts',(0.128748781223598,0.0322859803615266,
2.7));
#25508=CARTESIAN_POINT('Ctrl Pts',(0.126902487239724,0.0369045444632721,
2.7));
#25509=CARTESIAN_POINT('Ctrl Pts',(0.125403567336896,0.0406541410687207,
2.7));
#25510=CARTESIAN_POINT('Ctrl Pts',(0.123736334503949,0.0443441630809861,
2.7));
#25511=CARTESIAN_POINT('Ctrl Pts',(0.121913684068145,0.047935992310073,
2.7));
#25512=CARTESIAN_POINT('Ctrl Pts',(0.117743460752234,0.0561540958496606,
2.7));
#25513=CARTESIAN_POINT('Ctrl Pts',(0.112753744605352,0.0638862445298334,
2.7));
#25514=CARTESIAN_POINT('Ctrl Pts',(0.106960788703284,0.0709645017846505,
2.7));
#25515=CARTESIAN_POINT('Ctrl Pts',(0.104535029275377,0.0739284720891533,
2.7));
#25516=CARTESIAN_POINT('Ctrl Pts',(0.101968022916162,0.0767773427076814,
2.7));
#25517=CARTESIAN_POINT('Ctrl Pts',(0.0992594073891335,0.0794964656217155,
2.7));
#25518=CARTESIAN_POINT('Ctrl Pts',(0.0981919726164135,0.0805680412369242,
2.7));
#25519=CARTESIAN_POINT('Ctrl Pts',(0.0971025353237707,0.0816194476022307,
2.7));
#25520=CARTESIAN_POINT('Ctrl Pts',(0.0959918005672169,0.0826503307119895,
2.7));
#25521=CARTESIAN_POINT('Origin',(0.,0.,3.71042117235887));
#25522=CARTESIAN_POINT('Ctrl Pts',(-0.15446591465964,9.23303610504368E-5,
3.58542117235887));
#25523=CARTESIAN_POINT('Ctrl Pts',(-0.154510258305412,0.00608920819750747,
3.58511087053711));
#25524=CARTESIAN_POINT('Ctrl Pts',(-0.151481073290489,0.0629168758661166,
3.58216815720674));
#25525=CARTESIAN_POINT('Ctrl Pts',(-0.0810549264538156,0.163034932450524,
3.57659303236775));
#25526=CARTESIAN_POINT('Ctrl Pts',(0.0921890963056651,0.156981846810788,
3.56869579784192));
#25527=CARTESIAN_POINT('Ctrl Pts',(0.181852962765875,0.00863524897295638,
3.56079856331608));
#25528=CARTESIAN_POINT('Ctrl Pts',(0.10664300202618,-0.147556335146073,
3.55290132879024));
#25529=CARTESIAN_POINT('Ctrl Pts',(-0.0652523071804818,-0.169960705131912,
3.54500409426442));
#25530=CARTESIAN_POINT('Ctrl Pts',(-0.1484307843993,-0.072802923531341,
3.53917737545395));
#25531=CARTESIAN_POINT('Ctrl Pts',(-0.154428794390259,-0.0110220529132785,
3.53598306815211));
#25532=CARTESIAN_POINT('Ctrl Pts',(-0.154329957770701,-0.000135440264844458,
3.53542117235887));
#25533=CARTESIAN_POINT('Ctrl Pts',(-0.154140927489633,-0.000180264065019272,
3.58957882764113));
#25534=CARTESIAN_POINT('Ctrl Pts',(-0.153888356116389,0.0346192390763322,
3.58778772874353));
#25535=CARTESIAN_POINT('Ctrl Pts',(-0.125147291545086,0.121067307783401,
3.58336421833732));
#25536=CARTESIAN_POINT('Ctrl Pts',(0.0176337902165689,0.181151815132919,
3.5763082964225));
#25537=CARTESIAN_POINT('Ctrl Pts',(0.161334465098627,0.0843516096779105,
3.56841106189666));
#25538=CARTESIAN_POINT('Ctrl Pts',(0.158825384561566,-0.0890212772063117,
3.56051382737082));
#25539=CARTESIAN_POINT('Ctrl Pts',(0.0122890037691484,-0.181634540286447,
3.55261659284499));
#25540=CARTESIAN_POINT('Ctrl Pts',(-0.127027468209772,-0.117980653400407,
3.54563825960175));
#25541=CARTESIAN_POINT('Ctrl Pts',(-0.153922876401689,-0.0331947231106458,
3.54129233786714));
#25542=CARTESIAN_POINT('Ctrl Pts',(-0.154141660315178,0.000107924336747963,
3.53957882764113));
#25543=CARTESIAN_POINT('Ctrl Pts',(0.0958116152722374,0.0825211298936506,
3.6));
#25544=CARTESIAN_POINT('Ctrl Pts',(0.12310948837823,0.0508267830136165,
3.59736758849139));
#25545=CARTESIAN_POINT('Ctrl Pts',(0.143341746937054,-0.0412253317476725,
3.59210276547417));
#25546=CARTESIAN_POINT('Ctrl Pts',(0.0436608358730345,-0.142764465257081,
3.58420553094833));
#25547=CARTESIAN_POINT('Ctrl Pts',(-0.0955856094744946,-0.114504131671876,
3.57630829642249));
#25548=CARTESIAN_POINT('Ctrl Pts',(-0.148178789486409,0.0173870346414916,
3.56841106189666));
#25549=CARTESIAN_POINT('Ctrl Pts',(-0.066425116332372,0.133608342244775,
3.56051382737082));
#25550=CARTESIAN_POINT('Ctrl Pts',(0.0755496515090821,0.128647793449282,
3.55261659284499));
#25551=CARTESIAN_POINT('Ctrl Pts',(0.149029858339241,0.0070766508919659,
3.54471935831915));
#25552=CARTESIAN_POINT('Ctrl Pts',(0.0873947349721999,-0.120923516391581,
3.53682212379332));
#25553=CARTESIAN_POINT('Ctrl Pts',(-0.0534747520607383,-0.13928406457505,
3.52892488926748));
#25554=CARTESIAN_POINT('Ctrl Pts',(-0.145862599457632,-0.0313691495625942,
3.52102765474165));
#25555=CARTESIAN_POINT('Ctrl Pts',(-0.106007076394109,0.104987796417131,
3.5131304202158));
#25556=CARTESIAN_POINT('Ctrl Pts',(0.029957527138026,0.146158777133349,
3.50523318568998));
#25557=CARTESIAN_POINT('Ctrl Pts',(0.138761779048601,0.0548184317796861,
3.49733595116414));
#25558=CARTESIAN_POINT('Ctrl Pts',(0.121760532397217,-0.0862221662260755,
3.4894387166383));
#25559=CARTESIAN_POINT('Ctrl Pts',(-0.0056323702114988,-0.149091091323021,
3.48154148211246));
#25560=CARTESIAN_POINT('Ctrl Pts',(-0.127918803859021,-0.0767897408219312,
3.47364424758663));
#25561=CARTESIAN_POINT('Ctrl Pts',(-0.134230305961673,0.0651314716709306,
3.46574701306079));
#25562=CARTESIAN_POINT('Ctrl Pts',(-0.0188446861564537,0.148002567505592,
3.45784977853496));
#25563=CARTESIAN_POINT('Ctrl Pts',(0.113626077839972,0.0966902152561852,
3.44995254400912));
#25564=CARTESIAN_POINT('Ctrl Pts',(0.143080115058725,-0.0422843201504222,
3.44205530948329));
#25565=CARTESIAN_POINT('Ctrl Pts',(0.0428135339010967,-0.142922651128878,
3.43415807495745));
#25566=CARTESIAN_POINT('Ctrl Pts',(-0.0962690497602299,-0.113983126411312,
3.42626084043161));
#25567=CARTESIAN_POINT('Ctrl Pts',(-0.148071296290933,0.0182968362857149,
3.41836360590578));
#25568=CARTESIAN_POINT('Ctrl Pts',(-0.0656277734239754,0.133988351515145,
3.41046637137994));
#25569=CARTESIAN_POINT('Ctrl Pts',(0.076315808940436,0.128202107291143,
3.40256913685411));
#25570=CARTESIAN_POINT('Ctrl Pts',(0.149069246106613,0.0061840816248079,
3.39467190232827));
#25571=CARTESIAN_POINT('Ctrl Pts',(0.086672143362556,-0.121440613321149,
3.38677466780244));
#25572=CARTESIAN_POINT('Ctrl Pts',(-0.0543044603643882,-0.138963695209725,
3.37887743327661));
#25573=CARTESIAN_POINT('Ctrl Pts',(-0.14604705151224,-0.0304982252781714,
3.37098019875076));
#25574=CARTESIAN_POINT('Ctrl Pts',(-0.105379112789235,0.105617827984774,
3.36308296422493));
#25575=CARTESIAN_POINT('Ctrl Pts',(0.0308286127169663,0.145977668287988,
3.35518572969909));
#25576=CARTESIAN_POINT('Ctrl Pts',(0.139086215966064,0.0539898835791761,
3.34728849517326));
#25577=CARTESIAN_POINT('Ctrl Pts',(0.121244186506805,-0.0869467091899644,
3.33939126064743));
#25578=CARTESIAN_POINT('Ctrl Pts',(-0.00652136974010873,-0.149054871565549,
3.33149402612159));
#25579=CARTESIAN_POINT('Ctrl Pts',(-0.12837446138172,-0.0760255264081264,
3.32359679159575));
#25580=CARTESIAN_POINT('Ctrl Pts',(-0.133839510420159,0.0659307853068325,
3.31569955706992));
#25581=CARTESIAN_POINT('Ctrl Pts',(-0.0179617435035512,0.148112318093405,
3.30780232254408));
#25582=CARTESIAN_POINT('Ctrl Pts',(0.114200665588904,0.0960108899018034,
3.29990508801825));
#25583=CARTESIAN_POINT('Ctrl Pts',(0.142825410033637,-0.0431368201123976,
3.29200785349241));
#25584=CARTESIAN_POINT('Ctrl Pts',(0.0419604590288785,-0.143175426937629,
3.28411061896658));
#25585=CARTESIAN_POINT('Ctrl Pts',(-0.0969470717891682,-0.113407002747589,
3.27621338444074));
#25586=CARTESIAN_POINT('Ctrl Pts',(-0.147959550895179,0.0191795281376522,
3.26831614991491));
#25587=CARTESIAN_POINT('Ctrl Pts',(-0.0648275722345507,0.134377337668448,
3.26041891538907));
#25588=CARTESIAN_POINT('Ctrl Pts',(0.0770789801059626,0.127744721325426,
3.25252168086324));
#25589=CARTESIAN_POINT('Ctrl Pts',(0.149103473944927,0.00529500313887513,
3.24462444633739));
#25590=CARTESIAN_POINT('Ctrl Pts',(0.085946395912033,-0.121955319811881,
3.23672721181157));
#25591=CARTESIAN_POINT('Ctrl Pts',(-0.0551321992305218,-0.138637381714645,
3.22882997728572));
#25592=CARTESIAN_POINT('Ctrl Pts',(-0.146226329520922,-0.0296267371731131,
3.22093274275989));
#25593=CARTESIAN_POINT('Ctrl Pts',(-0.104747391252292,0.106244374093527,
3.21303550823405));
#25594=CARTESIAN_POINT('Ctrl Pts',(0.0316985965714106,0.145791227363271,
3.20513827370822));
#25595=CARTESIAN_POINT('Ctrl Pts',(0.139405709322103,0.0531594884201076,
3.19724103918239));
#25596=CARTESIAN_POINT('Ctrl Pts',(0.12072352734024,-0.0876681980379225,
3.18934380465655));
#25597=CARTESIAN_POINT('Ctrl Pts',(-0.00741013659566878,-0.149013331203351,
3.18144657013072));
#25598=CARTESIAN_POINT('Ctrl Pts',(-0.128825553891948,-0.0752586185437851,
3.17354933560487));
#25599=CARTESIAN_POINT('Ctrl Pts',(-0.133443954917441,0.0667277595658497,
3.16565210107904));
#25600=CARTESIAN_POINT('Ctrl Pts',(-0.0170781621796165,0.148216798566333,
3.15775486655321));
#25601=CARTESIAN_POINT('Ctrl Pts',(0.114771192054407,0.0953281515350871,
3.14985763202737));
#25602=CARTESIAN_POINT('Ctrl Pts',(0.14256562565491,-0.0439877867403021,
3.14196039750153));
#25603=CARTESIAN_POINT('Ctrl Pts',(0.0411058919243144,-0.143423110584706,
3.1340631629757));
#25604=CARTESIAN_POINT('Ctrl Pts',(-0.0976216460800827,-0.112826846172802,
3.12616592844987));
#25605=CARTESIAN_POINT('Ctrl Pts',(-0.147842543583951,0.0200615380096788,
3.11826869392402));
#25606=CARTESIAN_POINT('Ctrl Pts',(-0.0640250655728793,0.134761544882338,
3.11037145939819));
#25607=CARTESIAN_POINT('Ctrl Pts',(0.0778394100992752,0.127282792380129,
3.10247422487235));
#25608=CARTESIAN_POINT('Ctrl Pts',(0.14913239918967,0.00440573633107837,
3.09457699034652));
#25609=CARTESIAN_POINT('Ctrl Pts',(0.0852175919350427,-0.122465689176514,
3.08667975582068));
#25610=CARTESIAN_POINT('Ctrl Pts',(-0.0559579774207319,-0.138306137838011,
3.07878252129485));
#25611=CARTESIAN_POINT('Ctrl Pts',(-0.14640040725691,-0.028754195445133,
3.07088528676901));
#25612=CARTESIAN_POINT('Ctrl Pts',(-0.104111944565534,0.106867141813886,
3.06298805224318));
#25613=CARTESIAN_POINT('Ctrl Pts',(0.0325674531231242,0.145599601640112,
3.05509081771734));
#25614=CARTESIAN_POINT('Ctrl Pts',(0.139720244968427,0.0523272027405333,
3.04719358319151));
#25615=CARTESIAN_POINT('Ctrl Pts',(0.120198574861694,-0.0883865691262194,
3.03929634866567));
#25616=CARTESIAN_POINT('Ctrl Pts',(-0.00829863992324496,-0.148966491453986,
3.03139911413983));
#25617=CARTESIAN_POINT('Ctrl Pts',(-0.129272064956395,-0.0744890342439453,
3.023501879614));
#25618=CARTESIAN_POINT('Ctrl Pts',(-0.133043653723939,0.0675223607738245,
3.01560464508816));
#25619=CARTESIAN_POINT('Ctrl Pts',(-0.0161939735020032,0.148316007979255,
3.00770741056233));
#25620=CARTESIAN_POINT('Ctrl Pts',(0.115337636891868,0.0946420229965858,
2.9998101760365));
#25621=CARTESIAN_POINT('Ctrl Pts',(0.142300771189819,-0.0448371890228274,
2.99191294151066));
#25622=CARTESIAN_POINT('Ctrl Pts',(0.040249862963706,-0.14366569365053,
2.98401570698482));
#25623=CARTESIAN_POINT('Ctrl Pts',(-0.0982927486352741,-0.112242677117094,
2.97611847245899));
#25624=CARTESIAN_POINT('Ctrl Pts',(-0.14772027852239,0.0209428344297273,
2.96822123793315));
#25625=CARTESIAN_POINT('Ctrl Pts',(-0.0632202819765869,0.135140959547726,
2.96032400340732));
#25626=CARTESIAN_POINT('Ctrl Pts',(0.0785970718760291,0.126816336854618,
2.95242676888148));
#25627=CARTESIAN_POINT('Ctrl Pts',(0.149156020812652,0.00351631284117927,
2.94452953435565));
#25628=CARTESIAN_POINT('Ctrl Pts',(0.0844857573500313,-0.122971703272108,
2.93663229982981));
#25629=CARTESIAN_POINT('Ctrl Pts',(-0.0567817655678681,-0.137969975356402,
2.92873506530398));
#25630=CARTESIAN_POINT('Ctrl Pts',(-0.146569278528953,-0.0278806311257436,
2.92083783077813));
#25631=CARTESIAN_POINT('Ctrl Pts',(-0.103472795328523,0.107486108997575,
2.91294059625231));
#25632=CARTESIAN_POINT('Ctrl Pts',(0.0334351514749053,0.145402797936144,
2.90504336172646));
#25633=CARTESIAN_POINT('Ctrl Pts',(0.140029811715087,0.0514930561329736,
2.89714612720063));
#25634=CARTESIAN_POINT('Ctrl Pts',(0.119669347747977,-0.0891017968949556,
2.88924889267479));
#25635=CARTESIAN_POINT('Ctrl Pts',(-0.00918684813991898,-0.148914354007184,
2.88135165814896));
#25636=CARTESIAN_POINT('Ctrl Pts',(-0.129713978666681,-0.073716800831252,
2.87345442362312));
#25637=CARTESIAN_POINT('Ctrl Pts',(-0.132638621131497,0.0683145605832212,
2.86555718909729));
#25638=CARTESIAN_POINT('Ctrl Pts',(-0.0153092088077737,0.148409942975243,
2.85765995457145));
#25639=CARTESIAN_POINT('Ctrl Pts',(0.11589997974986,0.0939525283576191,
2.84976272004561));
#25640=CARTESIAN_POINT('Ctrl Pts',(0.14203085645546,-0.0456849961183085,
2.84186548551979));
#25641=CARTESIAN_POINT('Ctrl Pts',(0.0393924018242494,-0.143903168728488,
2.83396825099394));
#25642=CARTESIAN_POINT('Ctrl Pts',(-0.0989603541143928,-0.111654514006987,
2.82607101646811));
#25643=CARTESIAN_POINT('Ctrl Pts',(-0.14759276289462,0.0218233815372009,
2.81817378194227));
#25644=CARTESIAN_POINT('Ctrl Pts',(-0.0624132446091692,0.135515576866934,
2.81027654741644));
#25645=CARTESIAN_POINT('Ctrl Pts',(0.0793519279903814,0.126345354605138,
2.8023793128906));
#25646=CARTESIAN_POINT('Ctrl Pts',(0.149174358180394,0.00262679649731067,
2.79448207836477));
#25647=CARTESIAN_POINT('Ctrl Pts',(0.0837508793007237,-0.12347340605925,
2.78658484383893));
#25648=CARTESIAN_POINT('Ctrl Pts',(-0.0576034595552612,-0.137628787005506,
2.7786876093131));
#25649=CARTESIAN_POINT('Ctrl Pts',(-0.146733081304572,-0.0270063046901533,
2.77079037478726));
#25650=CARTESIAN_POINT('Ctrl Pts',(-0.102829689230287,0.108101695072837,
2.76289314026143));
#25651=CARTESIAN_POINT('Ctrl Pts',(0.0343011276704797,0.145199973805224,
2.75499590573559));
#25652=CARTESIAN_POINT('Ctrl Pts',(0.140335424370929,0.0506587128142576,
2.74709867120975));
#25653=CARTESIAN_POINT('Ctrl Pts',(0.11913389087728,-0.0898170012241629,
2.73920143668392));
#25654=CARTESIAN_POINT('Ctrl Pts',(-0.0100709312277202,-0.14885086814231,
2.73130420215808));
#25655=CARTESIAN_POINT('Ctrl Pts',(-0.130158589013459,-0.0729535941759648,
2.72340696763225));
#25656=CARTESIAN_POINT('Ctrl Pts',(-0.132214800612389,0.0691267612890124,
2.71550973310641));
#25657=CARTESIAN_POINT('Ctrl Pts',(-0.0144510241825876,0.148455288920992,
2.70761249858058));
#25658=CARTESIAN_POINT('Ctrl Pts',(0.116510849855331,0.0933444320528056,
2.69971526405474));
#25659=CARTESIAN_POINT('Ctrl Pts',(0.141650318794474,-0.0467072968399595,
2.6918180295289));
#25660=CARTESIAN_POINT('Ctrl Pts',(0.073068805953493,-0.111356443894342,
2.68655320651168));
#25661=CARTESIAN_POINT('Ctrl Pts',(0.0326585063531192,-0.122159831625552,
2.68392079500307));
#25662=CARTESIAN_POINT('Ctrl Pts',(0.102845629995664,0.088579422941069,
3.60535973499898));
#25663=CARTESIAN_POINT('Ctrl Pts',(0.132147577876935,0.0545582339347427,
3.60272732349037));
#25664=CARTESIAN_POINT('Ctrl Pts',(0.153865188751202,-0.0442518916242316,
3.59746250047314));
#25665=CARTESIAN_POINT('Ctrl Pts',(0.046866198411756,-0.153245525906639,
3.58956526594731));
#25666=CARTESIAN_POINT('Ctrl Pts',(-0.102603031970513,-0.122910458459966,
3.58166803142147));
#25667=CARTESIAN_POINT('Ctrl Pts',(-0.159057343031147,0.0186635046949134,
3.57377079689563));
#25668=CARTESIAN_POINT('Ctrl Pts',(-0.0713017197061865,0.143417205646691,
3.5658735623698));
#25669=CARTESIAN_POINT('Ctrl Pts',(0.0810961331079431,0.138092477903117,
3.55797632784396));
#25670=CARTESIAN_POINT('Ctrl Pts',(0.159970893148119,0.00759618358562943,
3.55007909331813));
#25671=CARTESIAN_POINT('Ctrl Pts',(0.0938108239901933,-0.129801122643079,
3.54218185879229));
#25672=CARTESIAN_POINT('Ctrl Pts',(-0.0574006037673195,-0.149509611427338,
3.53428462426646));
#25673=CARTESIAN_POINT('Ctrl Pts',(-0.156571109790821,-0.0336721173108959,
3.52638738974062));
#25674=CARTESIAN_POINT('Ctrl Pts',(-0.113789591426601,0.112695480957047,
3.51849015521479));
#25675=CARTESIAN_POINT('Ctrl Pts',(0.0321568605525351,0.15688903136602,
3.51059292068895));
#25676=CARTESIAN_POINT('Ctrl Pts',(0.148948982281772,0.0588429298027895,
3.50269568616312));
#25677=CARTESIAN_POINT('Ctrl Pts',(0.130699588222345,-0.092552171048525,
3.49479845163728));
#25678=CARTESIAN_POINT('Ctrl Pts',(-0.00604587096381251,-0.160036621554591,
3.48690121711144));
#25679=CARTESIAN_POINT('Ctrl Pts',(-0.137309969504135,-0.0824272636422575,
3.47900398258561));
#25680=CARTESIAN_POINT('Ctrl Pts',(-0.144084830862247,0.0699131020545748,
3.47110674805977));
#25681=CARTESIAN_POINT('Ctrl Pts',(-0.0202281697717358,0.158868183704434,
3.46320951353394));
#25682=CARTESIAN_POINT('Ctrl Pts',(0.121967942260279,0.103788732443176,
3.4553122790081));
#25683=CARTESIAN_POINT('Ctrl Pts',(0.153584349154903,-0.045388625715703,
3.44741504448227));
#25684=CARTESIAN_POINT('Ctrl Pts',(0.0459566917214356,-0.153415325002449,
3.43951780995643));
#25685=CARTESIAN_POINT('Ctrl Pts',(-0.103336647060408,-0.122351203571073,
3.43162057543059));
#25686=CARTESIAN_POINT('Ctrl Pts',(-0.158941958217129,0.0196400994742142,
3.42372334090476));
#25687=CARTESIAN_POINT('Ctrl Pts',(-0.0704458398266582,0.14382511331743,
3.41582610637892));
#25688=CARTESIAN_POINT('Ctrl Pts',(0.0819185380270082,0.137614071672475,
3.40792887185309));
#25689=CARTESIAN_POINT('Ctrl Pts',(0.160013172570483,0.00663808629925336,
3.40003163732726));
#25690=CARTESIAN_POINT('Ctrl Pts',(0.0930351832799072,-0.130356182270652,
3.39213440280141));
#25691=CARTESIAN_POINT('Ctrl Pts',(-0.0582912251492787,-0.149165722128378,
3.38423716827558));
#25692=CARTESIAN_POINT('Ctrl Pts',(-0.15676910340262,-0.0327372540747895,
3.37633993374974));
#25693=CARTESIAN_POINT('Ctrl Pts',(-0.113115525840982,0.11337176632503,
3.36844269922391));
#25694=CARTESIAN_POINT('Ctrl Pts',(0.0330918969246043,0.156694626405347,
3.36054546469807));
#25695=CARTESIAN_POINT('Ctrl Pts',(0.149297237752422,0.0579535536930025,
3.35264823017224));
#25696=CARTESIAN_POINT('Ctrl Pts',(0.130145334771507,-0.0933299063718294,
3.3447509956464));
#25697=CARTESIAN_POINT('Ctrl Pts',(-0.00700013643909911,-0.159997742721738,
3.33685376112057));
#25698=CARTESIAN_POINT('Ctrl Pts',(-0.137799079147585,-0.0816069443874761,
3.32895652659473));
#25699=CARTESIAN_POINT('Ctrl Pts',(-0.143665345045706,0.0707710973426707,
3.3210592920689));
#25700=CARTESIAN_POINT('Ctrl Pts',(-0.019280405838002,0.158985991637365,
3.31316205754306));
#25701=CARTESIAN_POINT('Ctrl Pts',(0.122584713398713,0.103059534382534,
3.30526482301722));
#25702=CARTESIAN_POINT('Ctrl Pts',(0.153310944947138,-0.0463037120067701,
3.29736758849139));
#25703=CARTESIAN_POINT('Ctrl Pts',(0.04504098831306,-0.15368665836036,3.28947035396555));
#25704=CARTESIAN_POINT('Ctrl Pts',(-0.1040644461119,-0.121732783758583,
3.28157311943972));
#25705=CARTESIAN_POINT('Ctrl Pts',(-0.158822009027328,0.0205875941944168,
3.27367588491388));
#25706=CARTESIAN_POINT('Ctrl Pts',(-0.0695868918252512,0.14424265690943,
3.26577865038805));
#25707=CARTESIAN_POINT('Ctrl Pts',(0.0827377374433846,0.137123106692272,
3.25788141586221));
#25708=CARTESIAN_POINT('Ctrl Pts',(0.160049913247329,0.00568373606998795,
3.24998418133638));
#25709=CARTESIAN_POINT('Ctrl Pts',(0.0922561550425197,-0.130908675965198,
3.24208694681054));
#25710=CARTESIAN_POINT('Ctrl Pts',(-0.0591797325073638,-0.148815452311067,
3.2341897122847));
#25711=CARTESIAN_POINT('Ctrl Pts',(-0.156961543115644,-0.0318017856251262,
3.22629247775887));
#25712=CARTESIAN_POINT('Ctrl Pts',(-0.112437426434515,0.114044310348977,
3.21839524323303));
#25713=CARTESIAN_POINT('Ctrl Pts',(0.0340257506890165,0.156494497910436,
3.21049800870719));
#25714=CARTESIAN_POINT('Ctrl Pts',(0.149640186729828,0.0570621950300983,
3.20260077418136));
#25715=CARTESIAN_POINT('Ctrl Pts',(0.129586451385121,-0.094104363361123,
3.19470353965552));
#25716=CARTESIAN_POINT('Ctrl Pts',(-0.00795415215963184,-0.159953152671687,
3.18680630512969));
#25717=CARTESIAN_POINT('Ctrl Pts',(-0.138283288637936,-0.0807837339423469,
3.17890907060385));
#25718=CARTESIAN_POINT('Ctrl Pts',(-0.143240749815163,0.0716265815084065,
3.17101183607802));
#25719=CARTESIAN_POINT('Ctrl Pts',(-0.0183319563451689,0.159098142549652,
3.16311460155218));
#25720=CARTESIAN_POINT('Ctrl Pts',(0.123197125094384,0.10232667274308,3.15521736702635));
#25721=CARTESIAN_POINT('Ctrl Pts',(0.153032088484722,-0.047217152393966,
3.14732013250051));
#25722=CARTESIAN_POINT('Ctrl Pts',(0.0441236831200233,-0.153952525715282,
3.13942289797468));
#25723=CARTESIAN_POINT('Ctrl Pts',(-0.104788544309502,-0.121110034958652,
3.13152566344884));
#25724=CARTESIAN_POINT('Ctrl Pts',(-0.158696411618254,0.021534356867118,
3.123628428923));
#25725=CARTESIAN_POINT('Ctrl Pts',(-0.0687254690952325,0.14465507071593,
3.11573119439717));
#25726=CARTESIAN_POINT('Ctrl Pts',(0.0835539944442463,0.136627265209407,
3.10783395987133));
#25727=CARTESIAN_POINT('Ctrl Pts',(0.160080962040421,0.00472918369319909,
3.0999367253455));
#25728=CARTESIAN_POINT('Ctrl Pts',(0.091473845883615,-0.131456514123307,
3.09203949081966));
#25729=CARTESIAN_POINT('Ctrl Pts',(-0.0600661352464005,-0.148459890147985,
3.08414225629383));
#25730=CARTESIAN_POINT('Ctrl Pts',(-0.157148400777682,-0.0308651862007597,
3.07624502176799));
#25731=CARTESIAN_POINT('Ctrl Pts',(-0.111755328396166,0.114712798593949,
3.06834778724216));
#25732=CARTESIAN_POINT('Ctrl Pts',(0.0349583943897092,0.156288803974834,
3.06045055271632));
#25733=CARTESIAN_POINT('Ctrl Pts',(0.149977814027003,0.0561688070540271,
3.05255331819049));
#25734=CARTESIAN_POINT('Ctrl Pts',(0.129022959493032,-0.0948754737002677,
3.04465608366465));
#25735=CARTESIAN_POINT('Ctrl Pts',(-0.00890788500525998,-0.159902874179684,
3.03675884913881));
#25736=CARTESIAN_POINT('Ctrl Pts',(-0.138762580335427,-0.0799576505710677,
3.02886161461298));
#25737=CARTESIAN_POINT('Ctrl Pts',(-0.142811060488699,0.072479518405434,
3.02096438008714));
#25738=CARTESIAN_POINT('Ctrl Pts',(-0.0173828549097553,0.159204635426789,
3.01306714556131));
#25739=CARTESIAN_POINT('Ctrl Pts',(0.123805155509077,0.101590172042203,
3.00516991103547));
#25740=CARTESIAN_POINT('Ctrl Pts',(0.152747789715287,-0.0481289135892851,
2.99727267650964));
#25741=CARTESIAN_POINT('Ctrl Pts',(0.0432048087487045,-0.154212918029513,
2.9893754419838));
#25742=CARTESIAN_POINT('Ctrl Pts',(-0.105508915893722,-0.120482979101306,
2.98147820745797));
#25743=CARTESIAN_POINT('Ctrl Pts',(-0.158565170460834,0.0224803537097271,
2.97358097293213));
#25744=CARTESIAN_POINT('Ctrl Pts',(-0.067861602269319,0.145062340128731,
2.9656837384063));
#25745=CARTESIAN_POINT('Ctrl Pts',(0.0843672799997867,0.136126564827205,
2.95778650388046));
#25746=CARTESIAN_POINT('Ctrl Pts',(0.160106317846084,0.0037744631314833,
2.94988926935462));
#25747=CARTESIAN_POINT('Ctrl Pts',(0.0906882836244439,-0.131999677270073,
2.94199203482879));
#25748=CARTESIAN_POINT('Ctrl Pts',(-0.0609504018432475,-0.148099048280287,
2.93409480030295));
#25749=CARTESIAN_POINT('Ctrl Pts',(-0.157329669742954,-0.0299274891113821,
2.92619756577712));
#25750=CARTESIAN_POINT('Ctrl Pts',(-0.111069255984644,0.115377207285653,
2.91830033125128));
#25751=CARTESIAN_POINT('Ctrl Pts',(0.0358897948611611,0.156077551916693,
2.91040309672545));
#25752=CARTESIAN_POINT('Ctrl Pts',(0.150310107632486,0.0552734215298454,
2.90250586219961));
#25753=CARTESIAN_POINT('Ctrl Pts',(0.128454879143209,-0.0956432099528824,
2.89460862767377));
#25754=CARTESIAN_POINT('Ctrl Pts',(-0.00986130107440376,-0.159846909059511,
2.88671139314794));
#25755=CARTESIAN_POINT('Ctrl Pts',(-0.139236937163761,-0.079128723602177,
2.8788141586221));
#25756=CARTESIAN_POINT('Ctrl Pts',(-0.142376292407395,0.0733298776050816,
2.87091692409627));
#25757=CARTESIAN_POINT('Ctrl Pts',(-0.0164331351694357,0.159305466665398,
2.86301968957043));
#25758=CARTESIAN_POINT('Ctrl Pts',(0.124408782797267,0.10085005811842,2.85512245504459));
#25759=CARTESIAN_POINT('Ctrl Pts',(0.152458059176653,-0.0490389624868201,
2.84722522051876));
#25760=CARTESIAN_POINT('Ctrl Pts',(0.0422843970550532,-0.154467827352683,
2.83932798599292));
#25761=CARTESIAN_POINT('Ctrl Pts',(-0.106225533663848,-0.11985163596585,
2.83143075146709));
#25762=CARTESIAN_POINT('Ctrl Pts',(-0.158428293266612,0.0234255462289395,
2.82353351694125));
#25763=CARTESIAN_POINT('Ctrl Pts',(-0.0669953162115558,0.145464459997932,
2.81563628241542));
#25764=CARTESIAN_POINT('Ctrl Pts',(0.085177553915074,0.13562100539136,2.80773904788958));
#25765=CARTESIAN_POINT('Ctrl Pts',(0.160126001452633,0.00281964289891892,
2.79984181336375));
#25766=CARTESIAN_POINT('Ctrl Pts',(0.0898994544648863,-0.132538212593453,
2.79194457883791));
#25767=CARTESIAN_POINT('Ctrl Pts',(-0.0618324205375044,-0.147732811568847,
2.78404734431207));
#25768=CARTESIAN_POINT('Ctrl Pts',(-0.157505498107873,-0.028988973955003,
2.77615010978624));
#25769=CARTESIAN_POINT('Ctrl Pts',(-0.110378936218723,0.11603798664468,
2.7682528752604));
#25770=CARTESIAN_POINT('Ctrl Pts',(0.0368193467442185,0.155859837441643,
2.76035564073457));
#25771=CARTESIAN_POINT('Ctrl Pts',(0.150638156857367,0.0543778248529476,
2.75245840620873));
#25772=CARTESIAN_POINT('Ctrl Pts',(0.127880111678472,-0.0964109210451539,
2.7445611716829));
#25773=CARTESIAN_POINT('Ctrl Pts',(-0.0108102891681236,-0.159778762376561,
2.73666393715706));
#25774=CARTESIAN_POINT('Ctrl Pts',(-0.139714188602295,-0.0783094860905571,
2.72876670263123));
#25775=CARTESIAN_POINT('Ctrl Pts',(-0.141921357082812,0.0742017060679738,
2.72086946810539));
#25776=CARTESIAN_POINT('Ctrl Pts',(-0.0155119468753121,0.159354141686116,
2.71297223357956));
#25777=CARTESIAN_POINT('Ctrl Pts',(0.125064499963334,0.100197318391729,
2.70507499905372));
#25778=CARTESIAN_POINT('Ctrl Pts',(0.152049584323474,-0.050136315469175,
2.69717776452788));
#25779=CARTESIAN_POINT('Ctrl Pts',(0.0784331561467309,-0.119531683020366,
2.69191294151066));
#25780=CARTESIAN_POINT('Ctrl Pts',(0.0350561322973247,-0.131128202024318,
2.68928053000205));
#25781=CARTESIAN_POINT('Ctrl Pts',(0.10987964471909,0.0946377159884874,
3.61071946999795));
#25782=CARTESIAN_POINT('Ctrl Pts',(0.14118566737564,0.0582896848558689,
3.60808705848934));
#25783=CARTESIAN_POINT('Ctrl Pts',(0.16438863056535,-0.0472784515007908,
3.60282223547212));
#25784=CARTESIAN_POINT('Ctrl Pts',(0.0500715609504776,-0.163726586556196,
3.59492500094628));
#25785=CARTESIAN_POINT('Ctrl Pts',(-0.109620454466532,-0.131316785248055,
3.58702776642045));
#25786=CARTESIAN_POINT('Ctrl Pts',(-0.169935896575886,0.0199399747483351,
3.57913053189461));
#25787=CARTESIAN_POINT('Ctrl Pts',(-0.0761783230800011,0.153226069048607,
3.57123329736878));
#25788=CARTESIAN_POINT('Ctrl Pts',(0.0866426147068042,0.147537162356952,
3.56333606284294));
#25789=CARTESIAN_POINT('Ctrl Pts',(0.170911927956997,0.00811571627929297,
3.55543882831711));
#25790=CARTESIAN_POINT('Ctrl Pts',(0.100226913008187,-0.138678728894576,
3.54754159379127));
#25791=CARTESIAN_POINT('Ctrl Pts',(-0.0613264554739007,-0.159735158279625,
3.53964435926544));
#25792=CARTESIAN_POINT('Ctrl Pts',(-0.167279620124009,-0.0359750850591977,
3.53174712473959));
#25793=CARTESIAN_POINT('Ctrl Pts',(-0.121572106459094,0.120403165496963,
3.52384989021377));
#25794=CARTESIAN_POINT('Ctrl Pts',(0.0343561939670442,0.167619285598691,
3.51595265568792));
#25795=CARTESIAN_POINT('Ctrl Pts',(0.159136185514944,0.0628674278258929,
3.5080554211621));
#25796=CARTESIAN_POINT('Ctrl Pts',(0.139638644047474,-0.0988821758709744,
3.50015818663625));
#25797=CARTESIAN_POINT('Ctrl Pts',(-0.00645937171612636,-0.170982151786161,
3.49226095211042));
#25798=CARTESIAN_POINT('Ctrl Pts',(-0.146701135149248,-0.0880647864625838,
3.48436371758458));
#25799=CARTESIAN_POINT('Ctrl Pts',(-0.15393935576282,0.074694732438219,
3.47646648305875));
#25800=CARTESIAN_POINT('Ctrl Pts',(-0.0216116533870178,0.169733799903276,
3.46856924853291));
#25801=CARTESIAN_POINT('Ctrl Pts',(0.130309806680585,0.110887249630166,
3.46067201400708));
#25802=CARTESIAN_POINT('Ctrl Pts',(0.164088583251082,-0.0484929312809838,
3.45277477948124));
#25803=CARTESIAN_POINT('Ctrl Pts',(0.0490998495417746,-0.16390799887602,
3.4448775449554));
#25804=CARTESIAN_POINT('Ctrl Pts',(-0.110404244360585,-0.130719280730833,
3.43698031042957));
#25805=CARTESIAN_POINT('Ctrl Pts',(-0.169812620143325,0.0209833626627134,
3.42908307590373));
#25806=CARTESIAN_POINT('Ctrl Pts',(-0.075263906229341,0.153661875119715,
3.4211858413779));
#25807=CARTESIAN_POINT('Ctrl Pts',(0.0875212671135803,0.147026036053807,
3.41328860685206));
#25808=CARTESIAN_POINT('Ctrl Pts',(0.170957099034354,0.00709209097369881,
3.40539137232623));
#25809=CARTESIAN_POINT('Ctrl Pts',(0.0993982231972585,-0.139271751220155,
3.39749413780039));
#25810=CARTESIAN_POINT('Ctrl Pts',(-0.0622779899341693,-0.15936774904703,
3.38959690327456));
#25811=CARTESIAN_POINT('Ctrl Pts',(-0.167491155293001,-0.0349762828714076,
3.38169966874872));
#25812=CARTESIAN_POINT('Ctrl Pts',(-0.120851938892729,0.121125704665286,
3.37380243422289));
#25813=CARTESIAN_POINT('Ctrl Pts',(0.0353551811322426,0.167411584522707,
3.36590519969705));
#25814=CARTESIAN_POINT('Ctrl Pts',(0.15950825953878,0.0619172238068289,
3.35800796517121));
#25815=CARTESIAN_POINT('Ctrl Pts',(0.139046483036208,-0.0997131035536944,
3.35011073064538));
#25816=CARTESIAN_POINT('Ctrl Pts',(-0.00747890313808957,-0.170940613877928,
3.34221349611955));
#25817=CARTESIAN_POINT('Ctrl Pts',(-0.14722369691345,-0.0871883623668259,
3.33431626159371));
#25818=CARTESIAN_POINT('Ctrl Pts',(-0.153491179671254,0.0756114093785092,
3.32641902706787));
#25819=CARTESIAN_POINT('Ctrl Pts',(-0.0205990681724529,0.169859665181325,
3.31852179254204));
#25820=CARTESIAN_POINT('Ctrl Pts',(0.130968761208522,0.110108178863265,
3.3106245580162));
#25821=CARTESIAN_POINT('Ctrl Pts',(0.16379647986064,-0.0494706039011429,
3.30272732349037));
#25822=CARTESIAN_POINT('Ctrl Pts',(0.0481215175972415,-0.16419788978309,
3.29483008896453));
#25823=CARTESIAN_POINT('Ctrl Pts',(-0.111181820434632,-0.130058564769576,
3.2869328544387));
#25824=CARTESIAN_POINT('Ctrl Pts',(-0.169684467159477,0.0219956602511813,
3.27903561991286));
#25825=CARTESIAN_POINT('Ctrl Pts',(-0.0743462114159517,0.154107976150411,
3.27113838538702));
#25826=CARTESIAN_POINT('Ctrl Pts',(0.0883964947808067,0.146501492059118,
3.26324115086119));
#25827=CARTESIAN_POINT('Ctrl Pts',(0.170996352549731,0.00607246900110077,
3.25534391633535));
#25828=CARTESIAN_POINT('Ctrl Pts',(0.0985659141730064,-0.139862032118515,
3.24744668180952));
#25829=CARTESIAN_POINT('Ctrl Pts',(-0.0632272657842059,-0.15899352290749,
3.23954944728368));
#25830=CARTESIAN_POINT('Ctrl Pts',(-0.167696756710366,-0.0339768340771394,
3.23165221275785));
#25831=CARTESIAN_POINT('Ctrl Pts',(-0.120127461616738,0.121844246604426,
3.22375497823201));
#25832=CARTESIAN_POINT('Ctrl Pts',(0.0363529048066224,0.167197768457601,
3.21585774370617));
#25833=CARTESIAN_POINT('Ctrl Pts',(0.159874664137553,0.0609649016400891,
3.20796050918034));
#25834=CARTESIAN_POINT('Ctrl Pts',(0.138449375430002,-0.100540528684324,
3.2000632746545));
#25835=CARTESIAN_POINT('Ctrl Pts',(-0.00849816772359493,-0.170892974140023,
3.19216604012867));
#25836=CARTESIAN_POINT('Ctrl Pts',(-0.147741023383925,-0.0863088493409087,
3.18426880560283));
#25837=CARTESIAN_POINT('Ctrl Pts',(-0.153037544712885,0.0765254034509632,
3.176371571077));
#25838=CARTESIAN_POINT('Ctrl Pts',(-0.0195857505107214,0.169979486532972,
3.16847433655116));
#25839=CARTESIAN_POINT('Ctrl Pts',(0.131623058134361,0.109325193951073,
3.16057710202532));
#25840=CARTESIAN_POINT('Ctrl Pts',(0.163498551314534,-0.0504465180476298,
3.15267986749949));
#25841=CARTESIAN_POINT('Ctrl Pts',(0.0471414743157323,-0.164481940845858,
3.14478263297365));
#25842=CARTESIAN_POINT('Ctrl Pts',(-0.111955442538922,-0.129393223744503,
3.13688539844782));
#25843=CARTESIAN_POINT('Ctrl Pts',(-0.169550279652557,0.0230071757245571,
3.12898816392198));
#25844=CARTESIAN_POINT('Ctrl Pts',(-0.0734258726175858,0.154548596549523,
3.12109092939615));
#25845=CARTESIAN_POINT('Ctrl Pts',(0.0892685787892176,0.145971738038684,
3.11319369487031));
#25846=CARTESIAN_POINT('Ctrl Pts',(0.171029524891172,0.00505263105532012,
3.10529646034447));
#25847=CARTESIAN_POINT('Ctrl Pts',(0.0977300998321875,-0.140447339070101,
3.09739922581864));
#25848=CARTESIAN_POINT('Ctrl Pts',(-0.0641742930720691,-0.158613642457959,
3.0895019912928));
#25849=CARTESIAN_POINT('Ctrl Pts',(-0.167896394298454,-0.0329761769563863,
3.08160475676697));
#25850=CARTESIAN_POINT('Ctrl Pts',(-0.119398712226798,0.122558455374011,
3.07370752224113));
#25851=CARTESIAN_POINT('Ctrl Pts',(0.0373493356562941,0.166978006309557,
3.0658102877153));
#25852=CARTESIAN_POINT('Ctrl Pts',(0.160235383085578,0.0600104113675208,
3.05791305318946));
#25853=CARTESIAN_POINT('Ctrl Pts',(0.13784734412437,-0.101364378274316,
3.05001581866363));
#25854=CARTESIAN_POINT('Ctrl Pts',(-0.00951713008727486,-0.170839256905381,
3.04211858413779));
#25855=CARTESIAN_POINT('Ctrl Pts',(-0.148253095714458,-0.0854262668981903,
3.03422134961195));
#25856=CARTESIAN_POINT('Ctrl Pts',(-0.152578467253459,0.0774366760370435,
3.02632411508612));
#25857=CARTESIAN_POINT('Ctrl Pts',(-0.0185717363175075,0.170093262874324,
3.01842688056029));
#25858=CARTESIAN_POINT('Ctrl Pts',(0.132272674126287,0.10853832108782,3.01052964603445));
#25859=CARTESIAN_POINT('Ctrl Pts',(0.163194808240755,-0.051420638155743,
3.00263241150862));
#25860=CARTESIAN_POINT('Ctrl Pts',(0.0461597545337032,-0.164760142408496,
2.99473517698277));
#25861=CARTESIAN_POINT('Ctrl Pts',(-0.112725083152171,-0.128723281085519,
2.98683794245694));
#25862=CARTESIAN_POINT('Ctrl Pts',(-0.169410062399277,0.024017872989727,
2.9789407079311));
#25863=CARTESIAN_POINT('Ctrl Pts',(-0.0725029225620513,0.154983720709736,
2.97104347340527));
#25864=CARTESIAN_POINT('Ctrl Pts',(0.0901374881235442,0.145436792799793,
2.96314623887944));
#25865=CARTESIAN_POINT('Ctrl Pts',(0.171056614879515,0.00403261342178739,
2.95524900435359));
#25866=CARTESIAN_POINT('Ctrl Pts',(0.0968908098988563,-0.141027651268038,
2.94735176982777));
#25867=CARTESIAN_POINT('Ctrl Pts',(-0.0651190381186268,-0.158228121204172,
2.93945453530192));
#25868=CARTESIAN_POINT('Ctrl Pts',(-0.168090060956955,-0.0319743470970206,
2.93155730077609));
#25869=CARTESIAN_POINT('Ctrl Pts',(-0.118665716640764,0.123268305573731,
2.92366006625025));
#25870=CARTESIAN_POINT('Ctrl Pts',(0.0383444382474168,0.166752305897243,
2.91576283172442));
#25871=CARTESIAN_POINT('Ctrl Pts',(0.160590403549885,0.0590537869267172,
2.90786559719859));
#25872=CARTESIAN_POINT('Ctrl Pts',(0.137240410538441,-0.102184623010809,
2.89996836267275));
#25873=CARTESIAN_POINT('Ctrl Pts',(-0.0105357540088883,-0.170779464111837,
2.89207112814692));
#25874=CARTESIAN_POINT('Ctrl Pts',(-0.14875989566084,-0.0845406463731019,
2.88417389362107));
#25875=CARTESIAN_POINT('Ctrl Pts',(-0.152113963683294,0.0783451946269418,
2.87627665909525));
#25876=CARTESIAN_POINT('Ctrl Pts',(-0.0175570615310977,0.170200990355554,
2.86837942456941));
#25877=CARTESIAN_POINT('Ctrl Pts',(0.132917585844673,0.10774758787922,2.86048219004357));
#25878=CARTESIAN_POINT('Ctrl Pts',(0.162885261897846,-0.0523929288553319,
2.85258495551774));
#25879=CARTESIAN_POINT('Ctrl Pts',(0.0451763922858567,-0.165032485976878,
2.8446877209919));
#25880=CARTESIAN_POINT('Ctrl Pts',(-0.113490713213303,-0.128048757924713,
2.83679048646607));
#25881=CARTESIAN_POINT('Ctrl Pts',(-0.169263823638604,0.0250277109206782,
2.82889325194023));
#25882=CARTESIAN_POINT('Ctrl Pts',(-0.0715773878139425,0.15541334312893,
2.82099601741439));
#25883=CARTESIAN_POINT('Ctrl Pts',(0.0910031798397666,0.144896656177581,
2.81309878288856));
#25884=CARTESIAN_POINT('Ctrl Pts',(0.171077644724872,0.00301248930052715,
2.80520154836272));
#25885=CARTESIAN_POINT('Ctrl Pts',(0.0960480296290492,-0.141603019127657,
2.79730431383689));
#25886=CARTESIAN_POINT('Ctrl Pts',(-0.0660613815197478,-0.157836836132188,
2.78940707931105));
#25887=CARTESIAN_POINT('Ctrl Pts',(-0.168277914911174,-0.0309716432198527,
2.78150984478522));
#25888=CARTESIAN_POINT('Ctrl Pts',(-0.11792818320716,0.123974278216523,
2.77361261025938));
#25889=CARTESIAN_POINT('Ctrl Pts',(0.0393375658179575,0.166519701078062,
2.76571537573355));
#25890=CARTESIAN_POINT('Ctrl Pts',(0.160940889343806,0.0580969368916377,
2.75781814120771));
#25891=CARTESIAN_POINT('Ctrl Pts',(0.136626332479664,-0.103004840866145,
2.74992090668187));
#25892=CARTESIAN_POINT('Ctrl Pts',(-0.011549647108527,-0.170706656610813,
2.74202367215604));
#25893=CARTESIAN_POINT('Ctrl Pts',(-0.149269788191131,-0.0836653780051494,
2.7341264376302));
#25894=CARTESIAN_POINT('Ctrl Pts',(-0.151627913553235,0.0792766508469352,
2.72622920310437));
#25895=CARTESIAN_POINT('Ctrl Pts',(-0.0165728695680367,0.170252994451239,
2.71833196857853));
#25896=CARTESIAN_POINT('Ctrl Pts',(0.133618150071337,0.107050204730652,
2.7104347340527));
#25897=CARTESIAN_POINT('Ctrl Pts',(0.162448849852474,-0.0535653340983903,
2.70253749952686));
#25898=CARTESIAN_POINT('Ctrl Pts',(0.0837975063399687,-0.127706922146391,
2.69727267650963));
#25899=CARTESIAN_POINT('Ctrl Pts',(0.0374537582415302,-0.140096572423083,
2.69464026500102));
#25900=CARTESIAN_POINT('Ctrl Pts',(0.116913659442517,0.100696009035906,
3.61607920499693));
#25901=CARTESIAN_POINT('Ctrl Pts',(0.150223756874345,0.0620211357769951,
3.61344679348832));
#25902=CARTESIAN_POINT('Ctrl Pts',(0.174912072379498,-0.0503050113773498,
3.60818197047109));
#25903=CARTESIAN_POINT('Ctrl Pts',(0.0532769234891989,-0.174207647205754,
3.60028473594526));
#25904=CARTESIAN_POINT('Ctrl Pts',(-0.11663787696255,-0.139723112036145,
3.59238750141943));
#25905=CARTESIAN_POINT('Ctrl Pts',(-0.180814450120624,0.0212164448017569,
3.58449026689359));
#25906=CARTESIAN_POINT('Ctrl Pts',(-0.0810549264538156,0.163034932450524,
3.57659303236775));
#25907=CARTESIAN_POINT('Ctrl Pts',(0.0921890963056651,0.156981846810788,
3.56869579784192));
#25908=CARTESIAN_POINT('Ctrl Pts',(0.181852962765875,0.00863524897295638,
3.56079856331608));
#25909=CARTESIAN_POINT('Ctrl Pts',(0.10664300202618,-0.147556335146073,
3.55290132879024));
#25910=CARTESIAN_POINT('Ctrl Pts',(-0.0652523071804818,-0.169960705131912,
3.54500409426442));
#25911=CARTESIAN_POINT('Ctrl Pts',(-0.177988130457198,-0.0382780528074994,
3.53710685973857));
#25912=CARTESIAN_POINT('Ctrl Pts',(-0.129354621491586,0.128110850036879,
3.52920962521275));
#25913=CARTESIAN_POINT('Ctrl Pts',(0.0365555273815534,0.178349539831362,
3.52131239068689));
#25914=CARTESIAN_POINT('Ctrl Pts',(0.169323388748115,0.0668919258489962,
3.51341515616108));
#25915=CARTESIAN_POINT('Ctrl Pts',(0.148577699872602,-0.105212180693424,
3.50551792163523));
#25916=CARTESIAN_POINT('Ctrl Pts',(-0.00687287246844015,-0.181927682017732,
3.4976206871094));
#25917=CARTESIAN_POINT('Ctrl Pts',(-0.156092300794361,-0.0937023092829102,
3.48972345258356));
#25918=CARTESIAN_POINT('Ctrl Pts',(-0.163793880663394,0.0794763628218631,
3.48182621805772));
#25919=CARTESIAN_POINT('Ctrl Pts',(-0.0229951370022999,0.180599416102118,
3.47392898353189));
#25920=CARTESIAN_POINT('Ctrl Pts',(0.138651671100891,0.117985766817156,
3.46603174900605));
#25921=CARTESIAN_POINT('Ctrl Pts',(0.174592817347261,-0.0515972368462645,
3.45813451448022));
#25922=CARTESIAN_POINT('Ctrl Pts',(0.0522430073621133,-0.174400672749591,
3.45023727995438));
#25923=CARTESIAN_POINT('Ctrl Pts',(-0.117471841660763,-0.139087357890593,
3.44234004542855));
#25924=CARTESIAN_POINT('Ctrl Pts',(-0.180683282069521,0.0223266258512126,
3.43444281090271));
#25925=CARTESIAN_POINT('Ctrl Pts',(-0.0800819726320239,0.163498636922,3.42654557637688));
#25926=CARTESIAN_POINT('Ctrl Pts',(0.0931239962001525,0.156438000435139,
3.41864834185104));
#25927=CARTESIAN_POINT('Ctrl Pts',(0.181901025498224,0.00754609564814438,
3.41075110732521));
#25928=CARTESIAN_POINT('Ctrl Pts',(0.10576126311461,-0.148187320169658,
3.40285387279937));
#25929=CARTESIAN_POINT('Ctrl Pts',(-0.0662647547190597,-0.169569775965683,
3.39495663827354));
#25930=CARTESIAN_POINT('Ctrl Pts',(-0.178213207183381,-0.0372153116680257,
3.3870594037477));
#25931=CARTESIAN_POINT('Ctrl Pts',(-0.128588351944475,0.128879643005541,
3.37916216922186));
#25932=CARTESIAN_POINT('Ctrl Pts',(0.0376184653398806,0.178128542640067,
3.37126493469602));
#25933=CARTESIAN_POINT('Ctrl Pts',(0.169719281325138,0.0658808939206553,
3.36336770017019));
#25934=CARTESIAN_POINT('Ctrl Pts',(0.14794763130091,-0.10609630073556,3.35547046564435));
#25935=CARTESIAN_POINT('Ctrl Pts',(-0.00795766983708003,-0.181883485034118,
3.34757323111852));
#25936=CARTESIAN_POINT('Ctrl Pts',(-0.156648314679315,-0.0927697803461756,
3.33967599659268));
#25937=CARTESIAN_POINT('Ctrl Pts',(-0.163317014296801,0.0804517214143475,
3.33177876206685));
#25938=CARTESIAN_POINT('Ctrl Pts',(-0.0219177305069036,0.180733338725286,
3.32388152754101));
#25939=CARTESIAN_POINT('Ctrl Pts',(0.139352809018331,0.117156823343995,
3.31598429301518));
#25940=CARTESIAN_POINT('Ctrl Pts',(0.174282014774141,-0.0526374957955154,
3.30808705848934));
#25941=CARTESIAN_POINT('Ctrl Pts',(0.0512020468814229,-0.174709121205821,
3.3001898239635));
#25942=CARTESIAN_POINT('Ctrl Pts',(-0.118299194757364,-0.13838434578057,
3.29229258943767));
#25943=CARTESIAN_POINT('Ctrl Pts',(-0.180546925291626,0.0234037263079457,
3.28439535491183));
#25944=CARTESIAN_POINT('Ctrl Pts',(-0.0791055310066521,0.163973295391393,
3.27649812038601));
#25945=CARTESIAN_POINT('Ctrl Pts',(0.0940552521182287,0.155879877425964,
3.26860088586016));
#25946=CARTESIAN_POINT('Ctrl Pts',(0.181942791852133,0.00646120193221371,
3.26070365133433));
#25947=CARTESIAN_POINT('Ctrl Pts',(0.104875673303493,-0.148815388271832,
3.25280641680849));
#25948=CARTESIAN_POINT('Ctrl Pts',(-0.067274799061048,-0.169171593503912,
3.24490918228266));
#25949=CARTESIAN_POINT('Ctrl Pts',(-0.178431970305088,-0.0361518825291525,
3.23701194775682));
#25950=CARTESIAN_POINT('Ctrl Pts',(-0.127817496798961,0.129644182859876,
3.22911471323099));
#25951=CARTESIAN_POINT('Ctrl Pts',(0.0386800589242284,0.177901039004767,
3.22121747870515));
#25952=CARTESIAN_POINT('Ctrl Pts',(0.170109141545278,0.0648676082500797,
3.21332024417931));
#25953=CARTESIAN_POINT('Ctrl Pts',(0.147312299474883,-0.106976694007524,
3.20542300965349));
#25954=CARTESIAN_POINT('Ctrl Pts',(-0.00904218328755787,-0.18183279560836,
3.19752577512764));
#25955=CARTESIAN_POINT('Ctrl Pts',(-0.157198758129913,-0.0918339647394704,
3.18962854060181));
#25956=CARTESIAN_POINT('Ctrl Pts',(-0.162834339610607,0.0814242253935201,
3.18173130607597));
#25957=CARTESIAN_POINT('Ctrl Pts',(-0.0208395446762738,0.180860830516292,
3.17383407155014));
#25958=CARTESIAN_POINT('Ctrl Pts',(0.140048991174337,0.116323715159066,
3.1659368370243));
#25959=CARTESIAN_POINT('Ctrl Pts',(0.173965014144346,-0.0536758837012937,
3.15803960249847));
#25960=CARTESIAN_POINT('Ctrl Pts',(0.050159265511441,-0.175011355976434,
3.15014236797263));
#25961=CARTESIAN_POINT('Ctrl Pts',(-0.119122340768341,-0.137676412530354,
3.14224513344679));
#25962=CARTESIAN_POINT('Ctrl Pts',(-0.180404147686861,0.0244799945819963,
3.13434789892096));
#25963=CARTESIAN_POINT('Ctrl Pts',(-0.0781262761399388,0.164442122383114,
3.12645066439512));
#25964=CARTESIAN_POINT('Ctrl Pts',(0.0949831631341886,0.155316210867962,
3.11855342986929));
#25965=CARTESIAN_POINT('Ctrl Pts',(0.181978087741923,0.00537607841744088,
3.11065619534345));
#25966=CARTESIAN_POINT('Ctrl Pts',(0.10398635378076,-0.149438164016893,
3.10275896081762));
#25967=CARTESIAN_POINT('Ctrl Pts',(-0.0682824508977375,-0.168767394767933,
3.09486172629178));
#25968=CARTESIAN_POINT('Ctrl Pts',(-0.178644387819226,-0.0350871677120128,
3.08696449176594));
#25969=CARTESIAN_POINT('Ctrl Pts',(-0.127042096057429,0.130404112154074,
3.07906725724011));
#25970=CARTESIAN_POINT('Ctrl Pts',(0.039740276922879,0.17766720864428,3.07117002271427));
#25971=CARTESIAN_POINT('Ctrl Pts',(0.170492952144154,0.0638520156810144,
3.06327278818844));
#25972=CARTESIAN_POINT('Ctrl Pts',(0.146671728755708,-0.107853282848364,
3.0553755536626));
#25973=CARTESIAN_POINT('Ctrl Pts',(-0.0101263751692898,-0.181775639631079,
3.04747831913677));
#25974=CARTESIAN_POINT('Ctrl Pts',(-0.15774361109349,-0.0908948832253125,
3.03958108461093));
#25975=CARTESIAN_POINT('Ctrl Pts',(-0.162345874018219,0.0823938336686527,
3.0316838500851));
#25976=CARTESIAN_POINT('Ctrl Pts',(-0.0197606177252597,0.180981890321858,
3.02378661555926));
#25977=CARTESIAN_POINT('Ctrl Pts',(0.140740192743497,0.115486470133437,
3.01588938103343));
#25978=CARTESIAN_POINT('Ctrl Pts',(0.173641826766224,-0.0547123627222005,
3.00799214650759));
#25979=CARTESIAN_POINT('Ctrl Pts',(0.0491147003187017,-0.175307366787479,
3.00009491198175));
#25980=CARTESIAN_POINT('Ctrl Pts',(-0.119941250410619,-0.136963583069732,
2.99219767745592));
#25981=CARTESIAN_POINT('Ctrl Pts',(-0.180254954337721,0.0255553922697266,
2.98430044293008));
#25982=CARTESIAN_POINT('Ctrl Pts',(-0.0771442428547834,0.164905101290741,
2.97640320840425));
#25983=CARTESIAN_POINT('Ctrl Pts',(0.0959076962473017,0.15474702077238,
2.96850597387841));
#25984=CARTESIAN_POINT('Ctrl Pts',(0.182006911912947,0.00429076371209153,
2.96060873935257));
#25985=CARTESIAN_POINT('Ctrl Pts',(0.103093336173269,-0.150055625266004,
2.95271150482674));
#25986=CARTESIAN_POINT('Ctrl Pts',(-0.069287674394006,-0.168357194128057,
2.9448142703009));
#25987=CARTESIAN_POINT('Ctrl Pts',(-0.178850452170956,-0.0340212050826592,
2.93691703577507));
#25988=CARTESIAN_POINT('Ctrl Pts',(-0.126262177296885,0.131159403861809,
2.92901980124923));
#25989=CARTESIAN_POINT('Ctrl Pts',(0.0407990816336726,0.177427059877793,
2.9211225667234));
#25990=CARTESIAN_POINT('Ctrl Pts',(0.170870699467283,0.0628341523235889,
2.91322533219756));
#25991=CARTESIAN_POINT('Ctrl Pts',(0.146025941933673,-0.108726036068736,
2.90532809767173));
#25992=CARTESIAN_POINT('Ctrl Pts',(-0.0112102069433731,-0.181712019164164,
2.89743086314589));
#25993=CARTESIAN_POINT('Ctrl Pts',(-0.158282854157919,-0.0899525691440268,
2.88953362862006));
#25994=CARTESIAN_POINT('Ctrl Pts',(-0.161851634959193,0.0833605116488022,
2.88163639409422));
#25995=CARTESIAN_POINT('Ctrl Pts',(-0.0186809878927599,0.181096514045709,
2.87373915956839));
#25996=CARTESIAN_POINT('Ctrl Pts',(0.14142638889208,0.114645117640021,2.86584192504255));
#25997=CARTESIAN_POINT('Ctrl Pts',(0.173312464619039,-0.0557468952238434,
2.85794469051671));
#25998=CARTESIAN_POINT('Ctrl Pts',(0.0480683875166603,-0.175597144601074,
2.85004745599088));
#25999=CARTESIAN_POINT('Ctrl Pts',(-0.120755892762759,-0.136245879883575,
2.84215022146504));
#26000=CARTESIAN_POINT('Ctrl Pts',(-0.180099354010596,0.0266298756124168,
2.83425298693921));
#26001=CARTESIAN_POINT('Ctrl Pts',(-0.0761594594163292,0.165362226259928,
2.82635575241337));
#26002=CARTESIAN_POINT('Ctrl Pts',(0.0968288057644592,0.154172306963803,
2.81845851788754));
#26003=CARTESIAN_POINT('Ctrl Pts',(0.182029287997112,0.0032053357021354,
2.8105612833617));
#26004=CARTESIAN_POINT('Ctrl Pts',(0.102196604793212,-0.150667825661861,
2.80266404883587));
#26005=CARTESIAN_POINT('Ctrl Pts',(-0.0702903425019912,-0.167940860695529,
2.79476681431002));
#26006=CARTESIAN_POINT('Ctrl Pts',(-0.179050331714475,-0.0329543124847025,
2.7868695797842));
#26007=CARTESIAN_POINT('Ctrl Pts',(-0.125477430195597,0.131910569788365,
2.77897234525835));
#26008=CARTESIAN_POINT('Ctrl Pts',(0.0418557848916964,0.17717956471448,
2.77107511073252));
#26009=CARTESIAN_POINT('Ctrl Pts',(0.171243621830244,0.0618160489303277,
2.76317787620668));
#26010=CARTESIAN_POINT('Ctrl Pts',(0.145372553280857,-0.109598760687136,
2.75528064168085));
#26011=CARTESIAN_POINT('Ctrl Pts',(-0.0122890050489303,-0.181634550845065,
2.74738340715501));
#26012=CARTESIAN_POINT('Ctrl Pts',(-0.158825387779967,-0.0890212699197419,
2.73948617262918));
#26013=CARTESIAN_POINT('Ctrl Pts',(-0.161334470023658,0.0843515956258966,
2.73158893810334));
#26014=CARTESIAN_POINT('Ctrl Pts',(-0.0176337922607613,0.181151847216363,
2.72369170357751));
#26015=CARTESIAN_POINT('Ctrl Pts',(0.14217180017934,0.113903091069576,2.71579446905167));
#26016=CARTESIAN_POINT('Ctrl Pts',(0.172848115381474,-0.0569943527276058,
2.70789723452584));
#26017=CARTESIAN_POINT('Ctrl Pts',(0.0891618565332066,-0.135882161272415,
2.70263241150861));
#26018=CARTESIAN_POINT('Ctrl Pts',(0.0398513841857358,-0.149064942821848,
2.7));
#26019=CARTESIAN_POINT('Ctrl Pts',(0.0958116152722374,0.0825211298936506,
3.6));
#26020=CARTESIAN_POINT('Ctrl Pts',(0.102493614798766,0.0762810303731869,
3.6));
#26021=CARTESIAN_POINT('Ctrl Pts',(0.108396094096263,0.0693090539021388,
3.6));
#26022=CARTESIAN_POINT('Ctrl Pts',(0.113512571306729,0.0617846659987563,
3.6));
#26023=CARTESIAN_POINT('Ctrl Pts',(0.117461600031764,0.0559771498608983,
3.6));
#26024=CARTESIAN_POINT('Ctrl Pts',(0.120942091267611,0.0498392138898472,
3.6));
#26025=CARTESIAN_POINT('Ctrl Pts',(0.123938893544148,0.0434377969520944,
3.6));
#26026=CARTESIAN_POINT('Ctrl Pts',(0.125176287448039,0.0407946214723323,
3.6));
#26027=CARTESIAN_POINT('Ctrl Pts',(0.126329312445263,0.0381097373250835,
3.6));
#26028=CARTESIAN_POINT('Ctrl Pts',(0.12739426777321,0.0353959223183902,
3.6));
#26029=CARTESIAN_POINT('Ctrl Pts',(0.130992400282108,0.0262268372474364,
3.6));
#26030=CARTESIAN_POINT('Ctrl Pts',(0.13360037697833,0.0167048680256365,
3.6));
#26031=CARTESIAN_POINT('Ctrl Pts',(0.135185783736742,0.0070125550480467,
3.6));
#26032=CARTESIAN_POINT('Ctrl Pts',(0.135855615028331,0.00291757154566029,
3.6));
#26033=CARTESIAN_POINT('Ctrl Pts',(0.13634239472836,-0.00120821237992505,
3.6));
#26034=CARTESIAN_POINT('Ctrl Pts',(0.136641151680689,-0.0053522141362822,
3.6));
#26035=CARTESIAN_POINT('Ctrl Pts',(0.136866179264237,-0.00847352962091436,
3.6));
#26036=CARTESIAN_POINT('Ctrl Pts',(0.136984148876184,-0.0116047424016575,
3.6));
#26037=CARTESIAN_POINT('Ctrl Pts',(0.136993305813875,-0.0147266162095009,
3.6));
#26038=CARTESIAN_POINT('Ctrl Pts',(0.1370171880242,-0.0228687756739225,
3.6));
#26039=CARTESIAN_POINT('Ctrl Pts',(0.1363045911537,-0.0309705737407376,
3.6));
#26040=CARTESIAN_POINT('Ctrl Pts',(0.134831565375878,-0.0389361856515032,
3.6));
#26041=CARTESIAN_POINT('Ctrl Pts',(0.133932184221546,-0.043799726631656,
3.6));
#26042=CARTESIAN_POINT('Ctrl Pts',(0.132748938308619,-0.0486126850413777,
3.6));
#26043=CARTESIAN_POINT('Ctrl Pts',(0.131298540463925,-0.0533602760289537,
3.6));
#26044=CARTESIAN_POINT('Ctrl Pts',(0.130441077796828,-0.0561670107778959,
3.6));
#26045=CARTESIAN_POINT('Ctrl Pts',(0.129489770756279,-0.058951963571448,
3.6));
#26046=CARTESIAN_POINT('Ctrl Pts',(0.128448797183808,-0.061708664264176,
3.6));
#26047=CARTESIAN_POINT('Ctrl Pts',(0.124844109667278,-0.0712545786242284,
3.6));
#26048=CARTESIAN_POINT('Ctrl Pts',(0.120197621014249,-0.0803872939153616,
3.6));
#26049=CARTESIAN_POINT('Ctrl Pts',(0.114666430721154,-0.0889848980033025,
3.6));
#26050=CARTESIAN_POINT('Ctrl Pts',(0.111763941762871,-0.0934964858552134,
3.6));
#26051=CARTESIAN_POINT('Ctrl Pts',(0.108616890563154,-0.0978607268708147,
3.6));
#26052=CARTESIAN_POINT('Ctrl Pts',(0.105242483611131,-0.102058774522217,
3.6));
#26053=CARTESIAN_POINT('Ctrl Pts',(0.103051571759935,-0.104784454169668,
3.6));
#26054=CARTESIAN_POINT('Ctrl Pts',(0.100763130867069,-0.107441777418394,
3.6));
#26055=CARTESIAN_POINT('Ctrl Pts',(0.098386472215756,-0.110019467506635,
3.6));
#26056=CARTESIAN_POINT('Ctrl Pts',(0.0926299038901994,-0.116262959438837,
3.6));
#26057=CARTESIAN_POINT('Ctrl Pts',(0.0863771877690887,-0.12201951201926,
3.6));
#26058=CARTESIAN_POINT('Ctrl Pts',(0.0796980248685607,-0.127218319244159,
3.6));
#26059=CARTESIAN_POINT('Ctrl Pts',(0.0749983795646852,-0.130876345006388,
3.6));
#26060=CARTESIAN_POINT('Ctrl Pts',(0.0700820293375014,-0.134260491890013,
3.6));
#26061=CARTESIAN_POINT('Ctrl Pts',(0.064997448628775,-0.137327043702736,
3.6));
#26062=CARTESIAN_POINT('Ctrl Pts',(0.0586168958330981,-0.141175206779031,
3.6));
#26063=CARTESIAN_POINT('Ctrl Pts',(0.0519659322704503,-0.144529310638398,
3.6));
#26064=CARTESIAN_POINT('Ctrl Pts',(0.0450857487477646,-0.147337352418514,
3.6));
#26065=CARTESIAN_POINT('Ctrl Pts',(0.0433856322299594,-0.148031228998597,
3.6));
#26066=CARTESIAN_POINT('Ctrl Pts',(0.0416714833555574,-0.148691718060548,
3.6));
#26067=CARTESIAN_POINT('Ctrl Pts',(0.0399441988940855,-0.149319076597487,
3.6));
#26068=CARTESIAN_POINT('Ctrl Pts',(-0.126474550616365,-0.00011099430647141,
3.51934196736194));
#26069=CARTESIAN_POINT('Ctrl Pts',(-0.126555547962724,-0.00903265450993761,
3.51990386315518));
#26070=CARTESIAN_POINT('Ctrl Pts',(-0.125690900286005,-0.0179387227435883,
3.52046575894841));
#26071=CARTESIAN_POINT('Ctrl Pts',(-0.123822037714229,-0.0266288110680491,
3.52102765474165));
#26072=CARTESIAN_POINT('Ctrl Pts',(-0.115066650325334,-0.0673407879000796,
3.52366006625026));
#26073=CARTESIAN_POINT('Ctrl Pts',(-0.0842707011930362,-0.103312426237565,
3.52629247775887));
#26074=CARTESIAN_POINT('Ctrl Pts',(-0.0453944787880641,-0.118238154042396,
3.52892488926748));
#26075=CARTESIAN_POINT('Ctrl Pts',(-0.00651825638309213,-0.133163881847227,
3.53155730077609));
#26076=CARTESIAN_POINT('Ctrl Pts',(0.0404382392945539,-0.127043699119404,
3.5341897122847));
#26077=CARTESIAN_POINT('Ctrl Pts',(0.0741890076945504,-0.102650246541568,
3.53682212379332));
#26078=CARTESIAN_POINT('Ctrl Pts',(0.107939776094547,-0.0782567939637322,
3.53945453530193));
#26079=CARTESIAN_POINT('Ctrl Pts',(0.128484817216894,-0.0355900715358833,
3.54208694681054));
#26080=CARTESIAN_POINT('Ctrl Pts',(0.126510636639707,0.00600514677092718,
3.54471935831915));
#26081=CARTESIAN_POINT('Ctrl Pts',(0.124536456062521,0.0476003650777378,
3.54735176982776));
#26082=CARTESIAN_POINT('Ctrl Pts',(0.100043053785802,0.0881240792635097,
3.54998418133637));
#26083=CARTESIAN_POINT('Ctrl Pts',(0.0641338913405327,0.109212694488978,
3.55261659284499));
#26084=CARTESIAN_POINT('Ctrl Pts',(0.028224728895264,0.130301309714446,
3.5552490043536));
#26085=CARTESIAN_POINT('Ctrl Pts',(-0.019100193718554,0.13195482597961,
3.55788141586221));
#26086=CARTESIAN_POINT('Ctrl Pts',(-0.0563882672178024,0.113411366178312,
3.56051382737082));
#26087=CARTESIAN_POINT('Ctrl Pts',(-0.0936763407170509,0.0948679063770136,
3.56314623887943));
#26088=CARTESIAN_POINT('Ctrl Pts',(-0.12092756510173,0.0561274705092526,
3.56577865038805));
#26089=CARTESIAN_POINT('Ctrl Pts',(-0.125787647292084,0.0147753915231441,
3.56841106189666));
#26090=CARTESIAN_POINT('Ctrl Pts',(-0.126360541139662,0.00990091600857084,
3.56872136371842));
#26091=CARTESIAN_POINT('Ctrl Pts',(-0.126622308248343,0.0049901515008091,
3.56903166554018));
#26092=CARTESIAN_POINT('Ctrl Pts',(-0.126585968300139,7.56654190205153E-5,
3.56934196736194));
#26093=CARTESIAN_POINT('Ctrl Pts',(-0.0398513841857247,-0.149064942821851,
3.6));
#26094=CARTESIAN_POINT('Ctrl Pts',(-0.0891618565331957,-0.135882161272422,
3.59736758849139));
#26095=CARTESIAN_POINT('Ctrl Pts',(-0.17284812802765,-0.0569944292149041,
3.59210276547417));
#26096=CARTESIAN_POINT('Ctrl Pts',(-0.142171789002704,0.113903133580536,
3.58420553094833));
#26097=CARTESIAN_POINT('Ctrl Pts',(0.0176337902165689,0.181151815132919,
3.5763082964225));
#26098=CARTESIAN_POINT('Ctrl Pts',(0.161334465098627,0.0843516096779105,
3.56841106189666));
#26099=CARTESIAN_POINT('Ctrl Pts',(0.158825384561566,-0.0890212772063117,
3.56051382737082));
#26100=CARTESIAN_POINT('Ctrl Pts',(0.0122890037691484,-0.181634540286447,
3.55261659284499));
#26101=CARTESIAN_POINT('Ctrl Pts',(-0.145372548664834,-0.109598761010981,
3.54471935831915));
#26102=CARTESIAN_POINT('Ctrl Pts',(-0.171243617690229,0.0618160491398297,
3.53682212379332));
#26103=CARTESIAN_POINT('Ctrl Pts',(-0.0418557834629445,0.177179558878914,
3.52892488926748));
#26104=CARTESIAN_POINT('Ctrl Pts',(0.125477426630257,0.13191056683484,3.52102765474164));
#26105=CARTESIAN_POINT('Ctrl Pts',(0.179050327003836,-0.0329543119327003,
3.51313042021581));
#26106=CARTESIAN_POINT('Ctrl Pts',(0.0702903405429243,-0.167940855985405,
3.50523318568997));
#26107=CARTESIAN_POINT('Ctrl Pts',(-0.102196602002365,-0.150667821707605,
3.49733595116413));
#26108=CARTESIAN_POINT('Ctrl Pts',(-0.182029283116568,0.00320533567306586,
3.4894387166383));
#26109=CARTESIAN_POINT('Ctrl Pts',(-0.0968288031440013,0.15417230277993,
3.48154148211247));
#26110=CARTESIAN_POINT('Ctrl Pts',(0.0761594573579975,0.165362221823523,
3.47364424758663));
#26111=CARTESIAN_POINT('Ctrl Pts',(0.180099349163956,0.0266298748857393,
3.46574701306079));
#26112=CARTESIAN_POINT('Ctrl Pts',(0.120755889508211,-0.136245876208876,
3.45784977853496));
#26113=CARTESIAN_POINT('Ctrl Pts',(-0.0480683862207756,-0.175597139874519,
3.44995254400912));
#26114=CARTESIAN_POINT('Ctrl Pts',(-0.173312459951882,-0.0557468937208932,
3.44205530948329));
#26115=CARTESIAN_POINT('Ctrl Pts',(-0.141426385082663,0.114645114551432,
3.43415807495745));
#26116=CARTESIAN_POINT('Ctrl Pts',(0.0186809873893989,0.181096509168673,
3.42626084043161));
#26117=CARTESIAN_POINT('Ctrl Pts',(0.161851630600137,0.0833605094034181,
3.41836360590578));
#26118=CARTESIAN_POINT('Ctrl Pts',(0.158282849894819,-0.0899525667211824,
3.41046637137994));
#26119=CARTESIAN_POINT('Ctrl Pts',(0.0112102066414966,-0.181712014270169,
3.40256913685411));
#26120=CARTESIAN_POINT('Ctrl Pts',(-0.146025938000753,-0.108726033140384,
3.39467190232827));
#26121=CARTESIAN_POINT('Ctrl Pts',(-0.170870694865204,0.0628341506312357,
3.38677466780244));
#26122=CARTESIAN_POINT('Ctrl Pts',(-0.0407990805348497,0.177427055099143,
3.3788774332766));
#26123=CARTESIAN_POINT('Ctrl Pts',(0.126262173896246,0.131159400329288,
3.37098019875077));
#26124=CARTESIAN_POINT('Ctrl Pts',(0.178850447353964,-0.0340212041663437,
3.36308296422493));
#26125=CARTESIAN_POINT('Ctrl Pts',(0.0692876725278909,-0.168357189593675,
3.3551857296991));
#26126=CARTESIAN_POINT('Ctrl Pts',(-0.103093333396635,-0.150055621224551,
3.34728849517326));
#26127=CARTESIAN_POINT('Ctrl Pts',(-0.18200690701094,0.00429076359651101,
3.33939126064742));
#26128=CARTESIAN_POINT('Ctrl Pts',(-0.0959076936642258,0.154747016604558,
3.33149402612159));
#26129=CARTESIAN_POINT('Ctrl Pts',(0.0771442407770374,0.164905096849345,
3.32359679159575));
#26130=CARTESIAN_POINT('Ctrl Pts',(0.180254949482897,0.0255553915814562,
3.31569955706992));
#26131=CARTESIAN_POINT('Ctrl Pts',(0.119941247180243,-0.13696357938087,
3.30780232254408));
#26132=CARTESIAN_POINT('Ctrl Pts',(-0.0491146989958762,-0.175307362065916,
3.29990508801825));
#26133=CARTESIAN_POINT('Ctrl Pts',(-0.173641822089509,-0.0547123612486432,
3.29200785349241));
#26134=CARTESIAN_POINT('Ctrl Pts',(-0.14074018895294,0.115486467023018,
3.28411061896658));
#26135=CARTESIAN_POINT('Ctrl Pts',(0.0197606171930289,0.18098188544746,
3.27621338444074));
#26136=CARTESIAN_POINT('Ctrl Pts',(0.162345869645737,0.0823938314495476,
3.26831614991491));
#26137=CARTESIAN_POINT('Ctrl Pts',(0.157743606844976,-0.0908948807772195,
3.26041891538907));
#26138=CARTESIAN_POINT('Ctrl Pts',(0.0101263748965706,-0.181775634735301,
3.25252168086324));
#26139=CARTESIAN_POINT('Ctrl Pts',(-0.146671724805377,-0.107853279943556,
3.2446244463374));
#26140=CARTESIAN_POINT('Ctrl Pts',(-0.170492947552259,0.0638520139612676,
3.23672721181156));
#26141=CARTESIAN_POINT('Ctrl Pts',(-0.0397402758525677,0.177667203859151,
3.22882997728572));
#26142=CARTESIAN_POINT('Ctrl Pts',(0.127042092635782,0.130404108641901,
3.22093274275989));
#26143=CARTESIAN_POINT('Ctrl Pts',(0.178644383007786,-0.0350871667669908,
3.21303550823405));
#26144=CARTESIAN_POINT('Ctrl Pts',(0.0682824490586963,-0.1687673902225,
3.20513827370822));
#26145=CARTESIAN_POINT('Ctrl Pts',(-0.103986350980073,-0.149438159992073,
3.19724103918238));
#26146=CARTESIAN_POINT('Ctrl Pts',(-0.181978082840693,0.00537607827262928,
3.18934380465655));
#26147=CARTESIAN_POINT('Ctrl Pts',(-0.0949831605760139,0.155316206684809,
3.18144657013072));
#26148=CARTESIAN_POINT('Ctrl Pts',(0.0781262740357409,0.164442117954189,
3.17354933560488));
#26149=CARTESIAN_POINT('Ctrl Pts',(0.180404142828019,0.0244799939226929,
3.16565210107904));
#26150=CARTESIAN_POINT('Ctrl Pts',(0.119122337560023,-0.137676408822293,
3.15775486655321));
#26151=CARTESIAN_POINT('Ctrl Pts',(-0.0501592641604809,-0.175011351262844,
3.14985763202737));
#26152=CARTESIAN_POINT('Ctrl Pts',(-0.173965009458927,-0.0536758822556528,
3.14196039750153));
#26153=CARTESIAN_POINT('Ctrl Pts',(-0.140048987402398,0.116323712026096,
3.1340631629757));
#26154=CARTESIAN_POINT('Ctrl Pts',(0.0208395441149821,0.180860825645154,
3.12616592844986));
#26155=CARTESIAN_POINT('Ctrl Pts',(0.162834335224968,0.0814242232005321,
3.11826869392403));
#26156=CARTESIAN_POINT('Ctrl Pts',(0.157198753896076,-0.0918339622660831,
3.1103714593982));
#26157=CARTESIAN_POINT('Ctrl Pts',(0.00904218304404205,-0.181832790711041,
3.10247422487235));
#26158=CARTESIAN_POINT('Ctrl Pts',(-0.147312295507299,-0.106976691126326,
3.09457699034652));
#26159=CARTESIAN_POINT('Ctrl Pts',(-0.170109136963721,0.0648676065029794,
3.08667975582068));
#26160=CARTESIAN_POINT('Ctrl Pts',(-0.0386800578824722,0.177901034213339,
3.07878252129485));
#26161=CARTESIAN_POINT('Ctrl Pts',(0.127817493356429,0.129644179368171,
3.07088528676902));
#26162=CARTESIAN_POINT('Ctrl Pts',(0.178431965499368,-0.0361518815554529,
3.06298805224317));
#26163=CARTESIAN_POINT('Ctrl Pts',(0.0672747972491473,-0.169171588947593,
3.05509081771735));
#26164=CARTESIAN_POINT('Ctrl Pts',(-0.104875670478854,-0.148815384263785,
3.0471935831915));
#26165=CARTESIAN_POINT('Ctrl Pts',(-0.181942786951853,0.00646120175817659,
3.03929634866568));
#26166=CARTESIAN_POINT('Ctrl Pts',(-0.0940552495850459,0.15587987322763,
3.03139911413983));
#26167=CARTESIAN_POINT('Ctrl Pts',(0.0791055288760802,0.163973290975094,
3.02350187961401));
#26168=CARTESIAN_POINT('Ctrl Pts',(0.180546920428939,0.0234037256776295,
3.01560464508816));
#26169=CARTESIAN_POINT('Ctrl Pts',(0.118299191571216,-0.138384342053441,
3.00770741056233));
#26170=CARTESIAN_POINT('Ctrl Pts',(-0.0512020455023775,-0.174709116500372,
2.99981017603649));
#26171=CARTESIAN_POINT('Ctrl Pts',(-0.174282010080185,-0.0526374943778417,
2.99191294151066));
#26172=CARTESIAN_POINT('Ctrl Pts',(-0.139352805265142,0.117156820188587,
2.98401570698483));
#26173=CARTESIAN_POINT('Ctrl Pts',(0.0219177299165732,0.180733333857582,
2.97611847245899));
#26174=CARTESIAN_POINT('Ctrl Pts',(0.163317009898163,0.0804517192475515,
2.96822123793315));
#26175=CARTESIAN_POINT('Ctrl Pts',(0.156648310460303,-0.0927697778475837,
2.96032400340732));
#26176=CARTESIAN_POINT('Ctrl Pts',(0.00795766962277319,-0.181883480135435,
2.95242676888148));
#26177=CARTESIAN_POINT('Ctrl Pts',(-0.147947627316214,-0.106096297878073,
2.94452953435564));
#26178=CARTESIAN_POINT('Ctrl Pts',(-0.169719276754081,0.0658808921462626,
2.93663229982981));
#26179=CARTESIAN_POINT('Ctrl Pts',(-0.0376184643267171,0.178128537842515,
2.92873506530397));
#26180=CARTESIAN_POINT('Ctrl Pts',(0.128588348481182,0.128879639534425,
2.92083783077814));
#26181=CARTESIAN_POINT('Ctrl Pts',(0.178213202383553,-0.0372153106656781,
2.9129405962523));
#26182=CARTESIAN_POINT('Ctrl Pts',(0.0662647529343645,-0.169569771398652,
2.90504336172647));
#26183=CARTESIAN_POINT('Ctrl Pts',(-0.105761260266122,-0.148187316178505,
2.89714612720063));
#26184=CARTESIAN_POINT('Ctrl Pts',(-0.181901020599063,0.00754609544484455,
2.8892488926748));
#26185=CARTESIAN_POINT('Ctrl Pts',(-0.0931239936920636,0.15643799622185,
2.88135165814895));
#26186=CARTESIAN_POINT('Ctrl Pts',(0.080081970475175,0.163498632518342,
2.87345442362313));
#26187=CARTESIAN_POINT('Ctrl Pts',(0.180683277203119,0.0223266252501708,
2.86555718909729));
#26188=CARTESIAN_POINT('Ctrl Pts',(0.11747183849698,-0.139087354145018,
2.85765995457145));
#26189=CARTESIAN_POINT('Ctrl Pts',(-0.0522430059551858,-0.174400668051551,
2.84976272004562));
#26190=CARTESIAN_POINT('Ctrl Pts',(-0.174592812644639,-0.0515972354582594,
2.84186548551978));
#26191=CARTESIAN_POINT('Ctrl Pts',(-0.138651667367148,0.117985763642445,
2.83396825099395));
#26192=CARTESIAN_POINT('Ctrl Pts',(0.0229951363840201,0.180599411232496,
2.82607101646811));
#26193=CARTESIAN_POINT('Ctrl Pts',(0.163793876249876,0.0794763606914083,
2.81817378194228));
#26194=CARTESIAN_POINT('Ctrl Pts',(0.1560922965942,-0.0937023067775016,
2.81027654741644));
#26195=CARTESIAN_POINT('Ctrl Pts',(0.00687287227597422,-0.181927677084725,
2.8023793128906));
#26196=CARTESIAN_POINT('Ctrl Pts',(-0.148577695856893,-0.105212177919503,
2.79448207836477));
#26197=CARTESIAN_POINT('Ctrl Pts',(-0.169323384214447,0.0668919241546485,
2.78658484383893));
#26198=CARTESIAN_POINT('Ctrl Pts',(-0.0365555263461618,0.178349534836247,
2.7786876093131));
#26199=CARTESIAN_POINT('Ctrl Pts',(0.129354617910885,0.128110846926664,
2.77079037478726));
#26200=CARTESIAN_POINT('Ctrl Pts',(0.177988125847537,-0.0382780523762908,
2.76289314026143));
#26201=CARTESIAN_POINT('Ctrl Pts',(0.0652523050728403,-0.169960699505811,
2.75499590573559));
#26202=CARTESIAN_POINT('Ctrl Pts',(-0.106642998487829,-0.147556332986489,
2.74709867120975));
#26203=CARTESIAN_POINT('Ctrl Pts',(-0.181852959134814,0.00863525184135577,
2.73920143668392));
#26204=CARTESIAN_POINT('Ctrl Pts',(-0.0921890914137533,0.156981837366664,
2.73130420215808));
#26205=CARTESIAN_POINT('Ctrl Pts',(0.081054919689294,0.163034936656946,
2.72340696763225));
#26206=CARTESIAN_POINT('Ctrl Pts',(0.180814453969382,0.0212164304176998,
2.71550973310641));
#26207=CARTESIAN_POINT('Ctrl Pts',(0.116637857196403,-0.139723086682139,
2.70761249858058));
#26208=CARTESIAN_POINT('Ctrl Pts',(-0.0532768903028442,-0.174207676028794,
2.69971526405474));
#26209=CARTESIAN_POINT('Ctrl Pts',(-0.17491212592378,-0.0503049553127666,
2.69181802952891));
#26210=CARTESIAN_POINT('Ctrl Pts',(-0.150223756874352,0.0620211357769783,
2.68655320651168));
#26211=CARTESIAN_POINT('Ctrl Pts',(-0.116913659442528,0.100696009035893,
2.68392079500307));
#26212=CARTESIAN_POINT('Ctrl Pts',(-0.0374537582415199,-0.140096572423086,
3.60535973499898));
#26213=CARTESIAN_POINT('Ctrl Pts',(-0.0837975063399586,-0.127706922146397,
3.60272732349037));
#26214=CARTESIAN_POINT('Ctrl Pts',(-0.162448861737804,-0.0535654059838928,
3.59746250047314));
#26215=CARTESIAN_POINT('Ctrl Pts',(-0.133618139567134,0.107050244683975,
3.5895652659473));
#26216=CARTESIAN_POINT('Ctrl Pts',(0.0165728676468313,0.170252964298069,
3.58166803142147));
#26217=CARTESIAN_POINT('Ctrl Pts',(0.151627908924514,0.0792766640535213,
3.57377079689563));
#26218=CARTESIAN_POINT('Ctrl Pts',(0.149269785166362,-0.0836653848533289,
3.5658735623698));
#26219=CARTESIAN_POINT('Ctrl Pts',(0.0115496459057422,-0.170706646687446,
3.55797632784397));
#26220=CARTESIAN_POINT('Ctrl Pts',(-0.136626328141362,-0.103004841170506,
3.55007909331813));
#26221=CARTESIAN_POINT('Ctrl Pts',(-0.160940885452871,0.0580969370885353,
3.54218185879229));
#26222=CARTESIAN_POINT('Ctrl Pts',(-0.0393375644751653,0.166519695593587,
3.53428462426645));
#26223=CARTESIAN_POINT('Ctrl Pts',(0.117928179856326,0.123974275440694,
3.52638738974062));
#26224=CARTESIAN_POINT('Ctrl Pts',(0.168277910483947,-0.0309716427010613,
3.51849015521478));
#26225=CARTESIAN_POINT('Ctrl Pts',(0.0660613796785464,-0.157836831705444,
3.51059292068895));
#26226=CARTESIAN_POINT('Ctrl Pts',(-0.0960480270061105,-0.141603015411306,
3.50269568616311));
#26227=CARTESIAN_POINT('Ctrl Pts',(-0.171077640137963,0.00301248927320663,
3.49479845163728));
#26228=CARTESIAN_POINT('Ctrl Pts',(-0.0910031773769663,0.144896652245428,
3.48690121711144));
#26229=CARTESIAN_POINT('Ctrl Pts',(0.0715773858794485,0.155413338959437,
3.47900398258561));
#26230=CARTESIAN_POINT('Ctrl Pts',(0.169263819083558,0.0250277102377205,
3.47110674805977));
#26231=CARTESIAN_POINT('Ctrl Pts',(0.113490710154562,-0.128048754471099,
3.46320951353393));
#26232=CARTESIAN_POINT('Ctrl Pts',(-0.0451763910679377,-0.165032481534694,
3.4553122790081));
#26233=CARTESIAN_POINT('Ctrl Pts',(-0.162885257511484,-0.0523929274428053,
3.44741504448226));
#26234=CARTESIAN_POINT('Ctrl Pts',(-0.132917582264447,0.107747584976454,
3.43951780995643));
#26235=CARTESIAN_POINT('Ctrl Pts',(0.0175570610580211,0.17020098577194,
3.43162057543059));
#26236=CARTESIAN_POINT('Ctrl Pts',(0.152113959586497,0.0783451925166497,
3.42372334090476));
#26237=CARTESIAN_POINT('Ctrl Pts',(0.148759891654226,-0.0845406440960262,
3.41582610637892));
#26238=CARTESIAN_POINT('Ctrl Pts',(0.0105357537251741,-0.170779459512285,
3.40792887185309));
#26239=CARTESIAN_POINT('Ctrl Pts',(-0.137240406842142,-0.102184620258639,
3.40003163732725));
#26240=CARTESIAN_POINT('Ctrl Pts',(-0.160590399224686,0.059053785336183,
3.39213440280142));
#26241=CARTESIAN_POINT('Ctrl Pts',(-0.0383444372147038,0.166752301406097,
3.38423716827558));
#26242=CARTESIAN_POINT('Ctrl Pts',(0.118665713444722,0.123268302253741,
3.37633993374974));
#26243=CARTESIAN_POINT('Ctrl Pts',(0.168090056429774,-0.0319743462358346,
3.36844269922391));
#26244=CARTESIAN_POINT('Ctrl Pts',(0.065119036364785,-0.158228116942597,
3.36054546469807));
#26245=CARTESIAN_POINT('Ctrl Pts',(-0.0968908072892766,-0.141027647469737,
3.35264823017224));
#26246=CARTESIAN_POINT('Ctrl Pts',(-0.171056610272434,0.00403261331316083,
3.3447509956464));
#26247=CARTESIAN_POINT('Ctrl Pts',(-0.090137485695877,0.145436788882724,
3.33685376112057));
#26248=CARTESIAN_POINT('Ctrl Pts',(0.0725029206093111,0.154983716535553,
3.32895652659473));
#26249=CARTESIAN_POINT('Ctrl Pts',(0.16941005783654,0.0240178723428656,
3.3210592920689));
#26250=CARTESIAN_POINT('Ctrl Pts',(0.112725080116148,-0.128723277618595,
3.31316205754306));
#26251=CARTESIAN_POINT('Ctrl Pts',(-0.0461597532904643,-0.164760137971002,
3.30526482301723));
#26252=CARTESIAN_POINT('Ctrl Pts',(-0.163194803845412,-0.0514206367708408,
3.29736758849139));
#26253=CARTESIAN_POINT('Ctrl Pts',(-0.132272670563786,0.108538318164536,
3.28947035396555));
#26254=CARTESIAN_POINT('Ctrl Pts',(0.0185717358172978,0.17009325829319,
3.28157311943971));
#26255=CARTESIAN_POINT('Ctrl Pts',(0.152578463144044,0.0774366739514488,
3.27367588491388));
#26256=CARTESIAN_POINT('Ctrl Pts',(0.148253091721553,-0.0854262645973846,
3.26577865038804));
#26257=CARTESIAN_POINT('Ctrl Pts',(0.00951712983096357,-0.170839252304153,
3.25788141586221));
#26258=CARTESIAN_POINT('Ctrl Pts',(-0.137847340411707,-0.101364375544273,
3.24998418133637));
#26259=CARTESIAN_POINT('Ctrl Pts',(-0.160235378769951,0.060010409751241,
3.24208694681054));
#26260=CARTESIAN_POINT('Ctrl Pts',(-0.0373493346503772,0.166978001812321,
3.2341897122847));
#26261=CARTESIAN_POINT('Ctrl Pts',(0.119398709011011,0.122558452073145,
3.22629247775887));
#26262=CARTESIAN_POINT('Ctrl Pts',(0.16789638977649,-0.0329761760682205,
3.21839524323303));
#26263=CARTESIAN_POINT('Ctrl Pts',(0.0641742913436723,-0.158613638185999,
3.2104980087072));
#26264=CARTESIAN_POINT('Ctrl Pts',(-0.0977300972000018,-0.14044733528743,
3.20260077418136));
#26265=CARTESIAN_POINT('Ctrl Pts',(-0.17102952028482,0.00505263091922082,
3.19470353965552));
#26266=CARTESIAN_POINT('Ctrl Pts',(-0.0892685763849535,0.145971734107207,
3.18680630512969));
#26267=CARTESIAN_POINT('Ctrl Pts',(0.0734258706399851,0.15454859238706,
3.17890907060385));
#26268=CARTESIAN_POINT('Ctrl Pts',(0.169550275086044,0.0230071751049201,
3.17101183607802));
#26269=CARTESIAN_POINT('Ctrl Pts',(0.11195543952363,-0.129393220259535,
3.16311460155218));
#26270=CARTESIAN_POINT('Ctrl Pts',(-0.0471414730460515,-0.164481936415857,
3.15521736702635));
#26271=CARTESIAN_POINT('Ctrl Pts',(-0.163498546911009,-0.0504465166889647,
3.14732013250051));
#26272=CARTESIAN_POINT('Ctrl Pts',(-0.131623054589357,0.109325191006596,
3.13942289797468));
#26273=CARTESIAN_POINT('Ctrl Pts',(0.0195857499831994,0.169979481954902,
3.13152566344884));
#26274=CARTESIAN_POINT('Ctrl Pts',(0.153037540591104,0.0765254013899147,
3.123628428923));
#26275=CARTESIAN_POINT('Ctrl Pts',(0.147741019404812,-0.0863088470163307,
3.11573119439717));
#26276=CARTESIAN_POINT('Ctrl Pts',(0.00849816749472986,-0.170892969537348,
3.10783395987133));
#26277=CARTESIAN_POINT('Ctrl Pts',(-0.138449371701125,-0.100540525976471,
3.09993672534551));
#26278=CARTESIAN_POINT('Ctrl Pts',(-0.159874659831641,0.0609648999981013,
3.09203949081965));
#26279=CARTESIAN_POINT('Ctrl Pts',(-0.0363529038275426,0.167197763954447,
3.08414225629384));
#26280=CARTESIAN_POINT('Ctrl Pts',(0.120127458381323,0.121844243322797,
3.07624502176798));
#26281=CARTESIAN_POINT('Ctrl Pts',(0.167696752193779,-0.0339768331620215,
3.06834778724216));
#26282=CARTESIAN_POINT('Ctrl Pts',(0.0632272640813166,-0.158993518625298,
3.06045055271632));
#26283=CARTESIAN_POINT('Ctrl Pts',(-0.0985659115183093,-0.139862028351609,
3.05255331819049));
#26284=CARTESIAN_POINT('Ctrl Pts',(-0.170996347944273,0.0060724688375345,
3.04465608366465));
#26285=CARTESIAN_POINT('Ctrl Pts',(-0.0883964924000305,0.146501488113373,
3.03675884913881));
#26286=CARTESIAN_POINT('Ctrl Pts',(0.0743462094135637,0.154107971999816,
3.02886161461298));
#26287=CARTESIAN_POINT('Ctrl Pts',(0.16968446258935,0.0219956596587875,
3.02096438008714));
#26288=CARTESIAN_POINT('Ctrl Pts',(0.111181817440176,-0.130058561266688,
3.01306714556131));
#26289=CARTESIAN_POINT('Ctrl Pts',(-0.048121516301165,-0.16419788536074,
3.00516991103547));
#26290=CARTESIAN_POINT('Ctrl Pts',(-0.163796475449092,-0.0494706025687624,
2.99727267650963));
#26291=CARTESIAN_POINT('Ctrl Pts',(-0.13096875768114,0.110108175897699,
2.9893754419838));
#26292=CARTESIAN_POINT('Ctrl Pts',(0.020599067617639,0.169859660606483,
2.98147820745796));
#26293=CARTESIAN_POINT('Ctrl Pts',(0.153491175537256,0.0756114073420768,
2.97358097293213));
#26294=CARTESIAN_POINT('Ctrl Pts',(0.147223692948271,-0.0871883600185597,
2.96568373840629));
#26295=CARTESIAN_POINT('Ctrl Pts',(0.00747890293667656,-0.17094060927397,
2.95778650388045));
#26296=CARTESIAN_POINT('Ctrl Pts',(-0.139046479291249,-0.0997131008681262,
2.94988926935462));
#26297=CARTESIAN_POINT('Ctrl Pts',(-0.159508255242737,0.0619172221391909,
2.94199203482878));
#26298=CARTESIAN_POINT('Ctrl Pts',(-0.0353551801800353,0.167411580013796,
2.93409480030295));
#26299=CARTESIAN_POINT('Ctrl Pts',(0.120851935637802,0.121125701403006,
2.92619756577711));
#26300=CARTESIAN_POINT('Ctrl Pts',(0.167491150781951,-0.0349762819293654,
2.91830033125128));
#26301=CARTESIAN_POINT('Ctrl Pts',(0.0622779882568489,-0.159367744754771,
2.91040309672545));
#26302=CARTESIAN_POINT('Ctrl Pts',(-0.0993982205201476,-0.139271747469127,
2.9025058621996));
#26303=CARTESIAN_POINT('Ctrl Pts',(-0.170957094429947,0.0070920907826306,
2.89460862767378));
#26304=CARTESIAN_POINT('Ctrl Pts',(-0.0875212647563887,0.147026032094007,
2.88671139314793));
#26305=CARTESIAN_POINT('Ctrl Pts',(0.0752639042022573,0.153661870981,2.8788141586221));
#26306=CARTESIAN_POINT('Ctrl Pts',(0.169812615569706,0.0209833620978328,
2.87091692409627));
#26307=CARTESIAN_POINT('Ctrl Pts',(0.110404241387148,-0.130719277210608,
2.86301968957043));
#26308=CARTESIAN_POINT('Ctrl Pts',(-0.0490998482194935,-0.163907994460633,
2.8551224550446));
#26309=CARTESIAN_POINT('Ctrl Pts',(-0.164088578831389,-0.0484929299764868,
2.84722522051876));
#26310=CARTESIAN_POINT('Ctrl Pts',(-0.130309803171479,0.110887246646458,
2.83932798599293));
#26311=CARTESIAN_POINT('Ctrl Pts',(0.0216116528059362,0.16973379532663,
2.83143075146709));
#26312=CARTESIAN_POINT('Ctrl Pts',(0.153939351614839,0.0746947304359413,
2.82353351694125));
#26313=CARTESIAN_POINT('Ctrl Pts',(0.146701131201786,-0.0880647841079112,
2.81563628241542));
#26314=CARTESIAN_POINT('Ctrl Pts',(0.00645937153523989,-0.170982147149946,
2.80773904788958));
#26315=CARTESIAN_POINT('Ctrl Pts',(-0.139638640273367,-0.0988821732639446,
2.79984181336375));
#26316=CARTESIAN_POINT('Ctrl Pts',(-0.15913618125404,0.0628674262334842,
2.79194457883791));
#26317=CARTESIAN_POINT('Ctrl Pts',(-0.0343561929939461,0.167619280904103,
2.78404734431207));
#26318=CARTESIAN_POINT('Ctrl Pts',(0.121572103093823,0.120403162573872,
2.77615010978624));
#26319=CARTESIAN_POINT('Ctrl Pts',(0.167279615791685,-0.0359750846539325,
2.7682528752604));
#26320=CARTESIAN_POINT('Ctrl Pts',(0.0613264534930637,-0.159735152992013,
2.76035564073457));
#26321=CARTESIAN_POINT('Ctrl Pts',(-0.100226909682718,-0.138678726864922,
2.75245840620873));
#26322=CARTESIAN_POINT('Ctrl Pts',(-0.170911924544395,0.00811571897511738,
2.74456117168289));
#26323=CARTESIAN_POINT('Ctrl Pts',(-0.0866426101092102,0.147537153481027,
2.73666393715706));
#26324=CARTESIAN_POINT('Ctrl Pts',(0.0761783167224614,0.153226073001953,
2.72876670263122));
#26325=CARTESIAN_POINT('Ctrl Pts',(0.169935900193086,0.0199399612296831,
2.72086946810539));
#26326=CARTESIAN_POINT('Ctrl Pts',(0.109620435889599,-0.131316761419452,
2.71297223357956));
#26327=CARTESIAN_POINT('Ctrl Pts',(-0.0500715297607526,-0.163726613645121,
2.70507499905371));
#26328=CARTESIAN_POINT('Ctrl Pts',(-0.164388680888184,-0.0472783988092873,
2.69717776452789));
#26329=CARTESIAN_POINT('Ctrl Pts',(-0.141185667375647,0.0582896848558531,
2.69191294151066));
#26330=CARTESIAN_POINT('Ctrl Pts',(-0.1098796447191,0.0946377159884756,
2.68928053000205));
#26331=CARTESIAN_POINT('Ctrl Pts',(-0.035056132297315,-0.13112820202432,
3.61071946999795));
#26332=CARTESIAN_POINT('Ctrl Pts',(-0.0784331561467214,-0.119531683020372,
3.60808705848934));
#26333=CARTESIAN_POINT('Ctrl Pts',(-0.152049595447957,-0.0501363827528818,
3.60282223547212));
#26334=CARTESIAN_POINT('Ctrl Pts',(-0.125064490131564,0.100197355787414,
3.59492500094628));
#26335=CARTESIAN_POINT('Ctrl Pts',(0.015511945077094,0.15935411346322,3.58702776642045));
#26336=CARTESIAN_POINT('Ctrl Pts',(0.141921352750402,0.074201718429132,
3.57913053189461));
#26337=CARTESIAN_POINT('Ctrl Pts',(0.139714185771159,-0.078309492500346,
3.57123329736877));
#26338=CARTESIAN_POINT('Ctrl Pts',(0.0108102880423358,-0.159778753088445,
3.56333606284294));
#26339=CARTESIAN_POINT('Ctrl Pts',(-0.127880107617888,-0.0964109213300309,
3.5554388283171));
#26340=CARTESIAN_POINT('Ctrl Pts',(-0.150638153215513,0.0543778250372407,
3.54754159379127));
#26341=CARTESIAN_POINT('Ctrl Pts',(-0.0368193454873861,0.155859832308261,
3.53964435926543));
#26342=CARTESIAN_POINT('Ctrl Pts',(0.110378933082395,0.116037984046548,
3.5317471247396));
#26343=CARTESIAN_POINT('Ctrl Pts',(0.157505493964057,-0.0289889734694223,
3.52384989021376));
#26344=CARTESIAN_POINT('Ctrl Pts',(0.0618324188141689,-0.147732807425485,
3.51595265568793));
#26345=CARTESIAN_POINT('Ctrl Pts',(-0.089899452009857,-0.132538209115007,
3.50805542116209));
#26346=CARTESIAN_POINT('Ctrl Pts',(-0.160125997159357,0.00281964287334723,
3.50015818663625));
#26347=CARTESIAN_POINT('Ctrl Pts',(-0.0851775516099315,0.135621001710926,
3.49226095211042));
#26348=CARTESIAN_POINT('Ctrl Pts',(0.0669953144008998,0.145464456095352,
3.48436371758458));
#26349=CARTESIAN_POINT('Ctrl Pts',(0.15842828900316,0.0234255455897019,
3.47646648305875));
#26350=CARTESIAN_POINT('Ctrl Pts',(0.106225530800914,-0.119851632733321,
3.46856924853291));
#26351=CARTESIAN_POINT('Ctrl Pts',(-0.0422843959151,-0.154467823194868,
3.46067201400708));
#26352=CARTESIAN_POINT('Ctrl Pts',(-0.152458055071087,-0.0490389611647173,
3.45277477948124));
#26353=CARTESIAN_POINT('Ctrl Pts',(-0.124408779446231,0.100850055401476,
3.44487754495541));
#26354=CARTESIAN_POINT('Ctrl Pts',(0.0164331347266433,0.159305462375208,
3.43698031042957));
#26355=CARTESIAN_POINT('Ctrl Pts',(0.142376288572858,0.0733298756298809,
3.42908307590374));
#26356=CARTESIAN_POINT('Ctrl Pts',(0.139236933413632,-0.0791287214708696,
3.4211858413779));
#26357=CARTESIAN_POINT('Ctrl Pts',(0.00986130080885162,-0.159846904754402,
3.41328860685207));
#26358=CARTESIAN_POINT('Ctrl Pts',(-0.128454875683531,-0.0956432073768941,
3.40539137232623));
#26359=CARTESIAN_POINT('Ctrl Pts',(-0.150310103584168,0.0552734200411303,
3.3974941378004));
#26360=CARTESIAN_POINT('Ctrl Pts',(-0.0358897938945578,0.15607754771305,
3.38959690327456));
#26361=CARTESIAN_POINT('Ctrl Pts',(0.111069252993198,0.115377204178194,
3.38169966874872));
#26362=CARTESIAN_POINT('Ctrl Pts',(0.157329665505583,-0.0299274883053255,
3.37380243422289));
#26363=CARTESIAN_POINT('Ctrl Pts',(0.060950400201679,-0.14809904429152,
3.36590519969705));
#26364=CARTESIAN_POINT('Ctrl Pts',(-0.090688281181918,-0.131999673714922,
3.35800796517121));
#26365=CARTESIAN_POINT('Ctrl Pts',(-0.160106313533927,0.00377446302981049,
3.35011073064538));
#26366=CARTESIAN_POINT('Ctrl Pts',(-0.0843672777275282,0.13612656116089,
3.34221349611954));
#26367=CARTESIAN_POINT('Ctrl Pts',(0.0678616004415848,0.145062336221761,
3.33431626159371));
#26368=CARTESIAN_POINT('Ctrl Pts',(0.158565166190183,0.0224803531042752,
3.32641902706787));
#26369=CARTESIAN_POINT('Ctrl Pts',(0.105508913052052,-0.12048297585632,
3.31852179254204));
#26370=CARTESIAN_POINT('Ctrl Pts',(-0.0432048075850524,-0.154212913876088,
3.3106245580162));
#26371=CARTESIAN_POINT('Ctrl Pts',(-0.152747785601314,-0.0481289122930385,
3.30272732349037));
#26372=CARTESIAN_POINT('Ctrl Pts',(-0.123805152174632,0.101590169306055,
3.29483008896453));
#26373=CARTESIAN_POINT('Ctrl Pts',(0.0173828544415669,0.159204631138919,
3.28693285443869));
#26374=CARTESIAN_POINT('Ctrl Pts',(0.142811056642351,0.0724795164533502,
3.27903561991286));
#26375=CARTESIAN_POINT('Ctrl Pts',(0.13876257659813,-0.0799576484175498,
3.27113838538702));
#26376=CARTESIAN_POINT('Ctrl Pts',(0.00890788476535658,-0.159902869873006,
3.26324115086119));
#26377=CARTESIAN_POINT('Ctrl Pts',(-0.129022956018037,-0.0948754711449903,
3.25534391633535));
#26378=CARTESIAN_POINT('Ctrl Pts',(-0.149977809987643,0.0561688055412144,
3.24744668180951));
#26379=CARTESIAN_POINT('Ctrl Pts',(-0.0349583934481866,0.156288799765492,
3.23954944728368));
#26380=CARTESIAN_POINT('Ctrl Pts',(0.111755325386239,0.11471279550439,3.23165221275784));
#26381=CARTESIAN_POINT('Ctrl Pts',(0.157148396545194,-0.0308651853694504,
3.22375497823201));
#26382=CARTESIAN_POINT('Ctrl Pts',(0.0600661336286481,-0.148459886149497,
3.21585774370617));
#26383=CARTESIAN_POINT('Ctrl Pts',(-0.0914738434199304,-0.131456510582787,
3.20796050918034));
#26384=CARTESIAN_POINT('Ctrl Pts',(-0.160080957728948,0.00472918356581254,
3.2000632746545));
#26385=CARTESIAN_POINT('Ctrl Pts',(-0.0835539921938928,0.136627261529605,
3.19216604012867));
#26386=CARTESIAN_POINT('Ctrl Pts',(0.0687254672442293,0.144655066819931,
3.18426880560283));
#26387=CARTESIAN_POINT('Ctrl Pts',(0.158696407344068,0.0215343562871474,
3.176371571077));
#26388=CARTESIAN_POINT('Ctrl Pts',(0.104788541487236,-0.121110031696776,
3.16847433655116));
#26389=CARTESIAN_POINT('Ctrl Pts',(-0.0441236819316221,-0.15395252156887,
3.16057710202533));
#26390=CARTESIAN_POINT('Ctrl Pts',(-0.153032084363091,-0.0472171511222767,
3.15267986749949));
#26391=CARTESIAN_POINT('Ctrl Pts',(-0.123197121776316,0.102326669987095,
3.14478263297366));
#26392=CARTESIAN_POINT('Ctrl Pts',(0.0183319558514166,0.159098138264651,
3.13688539844782));
#26393=CARTESIAN_POINT('Ctrl Pts',(0.143240745957241,0.0716265795792973,
3.12898816392198));
#26394=CARTESIAN_POINT('Ctrl Pts',(0.138283284913549,-0.0807837317665782,
3.12109092939615));
#26395=CARTESIAN_POINT('Ctrl Pts',(0.00795415194541781,-0.159953148363655,
3.11319369487031));
#26396=CARTESIAN_POINT('Ctrl Pts',(-0.12958644789495,-0.0941043608266151,
3.10529646034448));
#26397=CARTESIAN_POINT('Ctrl Pts',(-0.149640182699562,0.0570621934932236,
3.09739922581864));
#26398=CARTESIAN_POINT('Ctrl Pts',(-0.0340257497726133,0.156494493695554,
3.08950199129281));
#26399=CARTESIAN_POINT('Ctrl Pts',(0.112437423406217,0.114044307277423,
3.08160475676696));
#26400=CARTESIAN_POINT('Ctrl Pts',(0.156961538888189,-0.0318017847685902,
3.07370752224114));
#26401=CARTESIAN_POINT('Ctrl Pts',(0.0591797309134862,-0.148815448303003,
3.06581028771529));
#26402=CARTESIAN_POINT('Ctrl Pts',(-0.0922561525577649,-0.130908672439433,
3.05791305318946));
#26403=CARTESIAN_POINT('Ctrl Pts',(-0.160049908936692,0.00568373591689232,
3.05001581866362));
#26404=CARTESIAN_POINT('Ctrl Pts',(-0.0827377352150154,0.137123102999116,
3.04211858413779));
#26405=CARTESIAN_POINT('Ctrl Pts',(0.0695868899510474,0.144242653024537,
3.03422134961195));
#26406=CARTESIAN_POINT('Ctrl Pts',(0.15882200474976,0.0205875936399453,
3.02632411508612));
#26407=CARTESIAN_POINT('Ctrl Pts',(0.104064443309136,-0.121732780479934,
3.01842688056028));
#26408=CARTESIAN_POINT('Ctrl Pts',(-0.0450409870999527,-0.153686654221109,
3.01052964603445));
#26409=CARTESIAN_POINT('Ctrl Pts',(-0.153310940817998,-0.0463037107596828,
3.00263241150861));
#26410=CARTESIAN_POINT('Ctrl Pts',(-0.122584710097139,0.103059531606811,
2.99473517698278));
#26411=CARTESIAN_POINT('Ctrl Pts',(0.019280405318705,0.158985987355384,
2.98683794245694));
#26412=CARTESIAN_POINT('Ctrl Pts',(0.143665341176349,0.0707710954366019,
2.97894070793111));
#26413=CARTESIAN_POINT('Ctrl Pts',(0.13779907543624,-0.0816069421895357,
2.97104347340527));
#26414=CARTESIAN_POINT('Ctrl Pts',(0.00700013625057968,-0.159997738412506,
2.96314623887943));
#26415=CARTESIAN_POINT('Ctrl Pts',(-0.130145331266283,-0.0933299038581796,
2.9552490043536));
#26416=CARTESIAN_POINT('Ctrl Pts',(-0.149297233731393,0.0579535521321195,
2.94735176982776));
#26417=CARTESIAN_POINT('Ctrl Pts',(-0.0330918960333533,0.156694622185077,
2.93945453530193));
#26418=CARTESIAN_POINT('Ctrl Pts',(0.113115522794421,0.113371763271587,
2.93155730077609));
#26419=CARTESIAN_POINT('Ctrl Pts',(0.156769099180348,-0.0327372531930529,
2.92366006625026));
#26420=CARTESIAN_POINT('Ctrl Pts',(0.0582912235793329,-0.14916571811089,
2.91576283172442));
#26421=CARTESIAN_POINT('Ctrl Pts',(-0.0930351807741731,-0.130356178759748,
2.90786559719858));
#26422=CARTESIAN_POINT('Ctrl Pts',(-0.160013168260831,0.00663808612041647,
2.89996836267275));
#26423=CARTESIAN_POINT('Ctrl Pts',(-0.0819185358207136,0.137614067966164,
2.89207112814691));
#26424=CARTESIAN_POINT('Ctrl Pts',(0.0704458379293395,0.143825109443657,
2.88417389362108));
#26425=CARTESIAN_POINT('Ctrl Pts',(0.158941953936293,0.0196400989454948,
2.87627665909524));
#26426=CARTESIAN_POINT('Ctrl Pts',(0.103336644277317,-0.122351200276197,
2.86837942456941));
#26427=CARTESIAN_POINT('Ctrl Pts',(-0.0459566904838012,-0.153415320869716,
2.86048219004357));
#26428=CARTESIAN_POINT('Ctrl Pts',(-0.15358434501814,-0.0453886244947142,
2.85258495551773));
#26429=CARTESIAN_POINT('Ctrl Pts',(-0.12196793897581,0.103788729650472,
2.8446877209919));
#26430=CARTESIAN_POINT('Ctrl Pts',(0.0202281692278525,0.158868179420765,
2.83679048646607));
#26431=CARTESIAN_POINT('Ctrl Pts',(0.144084826979801,0.0699131001804741,
2.82889325194023));
#26432=CARTESIAN_POINT('Ctrl Pts',(0.137309965809371,-0.0824272614383206,
2.8209960174144));
#26433=CARTESIAN_POINT('Ctrl Pts',(0.00604587079450571,-0.160036617215166,
2.81309878288855));
#26434=CARTESIAN_POINT('Ctrl Pts',(-0.13069958468984,-0.0925521686083858,
2.80520154836272));
#26435=CARTESIAN_POINT('Ctrl Pts',(-0.148948978293633,0.0588429283123199,
2.79730431383689));
#26436=CARTESIAN_POINT('Ctrl Pts',(-0.0321568596417307,0.156889026971959,
2.78940707931105));
#26437=CARTESIAN_POINT('Ctrl Pts',(0.113789588276761,0.11269547822108,2.78150984478522));
#26438=CARTESIAN_POINT('Ctrl Pts',(0.156571105735832,-0.0336721169315741,
2.77361261025938));
#26439=CARTESIAN_POINT('Ctrl Pts',(0.0574006019132872,-0.149509606478216,
2.76571537573355));
#26440=CARTESIAN_POINT('Ctrl Pts',(-0.0938108208776064,-0.129801120743354,
2.75781814120771));
#26441=CARTESIAN_POINT('Ctrl Pts',(-0.159970889953977,0.00759618610887905,
2.74992090668187));
#26442=CARTESIAN_POINT('Ctrl Pts',(-0.0810961288046671,0.138092469595389,
2.74202367215604));
#26443=CARTESIAN_POINT('Ctrl Pts',(0.0713017137556289,0.143417209346961,
2.7341264376302));
#26444=CARTESIAN_POINT('Ctrl Pts',(0.15905734641679,0.0186634920416663,
2.72622920310437));
#26445=CARTESIAN_POINT('Ctrl Pts',(0.102603014582794,-0.122910436156766,
2.71833196857853));
#26446=CARTESIAN_POINT('Ctrl Pts',(-0.046866169218661,-0.153245551261449,
2.7104347340527));
#26447=CARTESIAN_POINT('Ctrl Pts',(-0.153865235852588,-0.044251842305808,
2.70253749952686));
#26448=CARTESIAN_POINT('Ctrl Pts',(-0.132147577876941,0.0545582339347279,
2.69727267650964));
#26449=CARTESIAN_POINT('Ctrl Pts',(-0.102845629995673,0.0885794229410579,
2.69464026500102));
#26450=CARTESIAN_POINT('Ctrl Pts',(-0.0326585063531101,-0.122159831625555,
3.61607920499693));
#26451=CARTESIAN_POINT('Ctrl Pts',(-0.0730688059534842,-0.111356443894347,
3.61344679348832));
#26452=CARTESIAN_POINT('Ctrl Pts',(-0.14165032915811,-0.0467073595218706,
3.60818197047109));
#26453=CARTESIAN_POINT('Ctrl Pts',(-0.116510840695994,0.0933444668908538,
3.60028473594526));
#26454=CARTESIAN_POINT('Ctrl Pts',(0.0144510225073566,0.148455262628371,
3.59238750141942));
#26455=CARTESIAN_POINT('Ctrl Pts',(0.132214796576289,0.0691267728047427,
3.58449026689359));
#26456=CARTESIAN_POINT('Ctrl Pts',(0.130158586375956,-0.0729536001473631,
3.57659303236775));
#26457=CARTESIAN_POINT('Ctrl Pts',(0.0100709301789295,-0.148850859489444,
3.56869579784192));
#26458=CARTESIAN_POINT('Ctrl Pts',(-0.119133887094416,-0.0898170014895561,
3.56079856331608));
#26459=CARTESIAN_POINT('Ctrl Pts',(-0.140335420978156,0.0506587129859461,
3.55290132879025));
#26460=CARTESIAN_POINT('Ctrl Pts',(-0.0343011264996069,0.145199969022934,
3.54500409426441));
#26461=CARTESIAN_POINT('Ctrl Pts',(0.102829686308464,0.108101692652402,
3.53710685973857));
#26462=CARTESIAN_POINT('Ctrl Pts',(0.146733077444168,-0.0270063042377832,
3.52920962521274));
#26463=CARTESIAN_POINT('Ctrl Pts',(0.0576034579497911,-0.137628783145524,
3.5213123906869));
#26464=CARTESIAN_POINT('Ctrl Pts',(-0.0837508770136032,-0.123473402818708,
3.51341515616107));
#26465=CARTESIAN_POINT('Ctrl Pts',(-0.149174354180752,0.00262679647348802,
3.50551792163523));
#26466=CARTESIAN_POINT('Ctrl Pts',(-0.0793519258428967,0.126345351176423,
3.4976206871094));
#26467=CARTESIAN_POINT('Ctrl Pts',(0.062413242922351,0.135515573231267,
3.48972345258356));
#26468=CARTESIAN_POINT('Ctrl Pts',(0.147592758922763,0.0218233809416831,
3.48182621805773));
#26469=CARTESIAN_POINT('Ctrl Pts',(0.0989603514472664,-0.111654510995544,
3.47392898353189));
#26470=CARTESIAN_POINT('Ctrl Pts',(-0.0393924007622622,-0.143903164855042,
3.46603174900606));
#26471=CARTESIAN_POINT('Ctrl Pts',(-0.14203085263069,-0.0456849948866295,
3.45813451448022));
#26472=CARTESIAN_POINT('Ctrl Pts',(-0.115899976628015,0.0939525258264977,
3.45023727995438));
#26473=CARTESIAN_POINT('Ctrl Pts',(0.0153092083952656,0.148409938978475,
3.44234004542855));
#26474=CARTESIAN_POINT('Ctrl Pts',(0.132638617559218,0.0683145587431124,
3.43444281090271));
#26475=CARTESIAN_POINT('Ctrl Pts',(0.129713975173039,-0.0737167988457132,
3.42654557637688));
#26476=CARTESIAN_POINT('Ctrl Pts',(0.00918684789252914,-0.148914349996519,
3.41864834185104));
#26477=CARTESIAN_POINT('Ctrl Pts',(-0.11966934452492,-0.0891017944951492,
3.4107511073252));
#26478=CARTESIAN_POINT('Ctrl Pts',(-0.140029807943649,0.0514930547460776,
3.40285387279937));
#26479=CARTESIAN_POINT('Ctrl Pts',(-0.0334351505744119,0.145402794020004,
3.39495663827353));
#26480=CARTESIAN_POINT('Ctrl Pts',(0.103472792541674,0.107486106102647,
3.3870594037477));
#26481=CARTESIAN_POINT('Ctrl Pts',(0.146569274581392,-0.0278806303748164,
3.37916216922186));
#26482=CARTESIAN_POINT('Ctrl Pts',(0.0567817640385731,-0.137969971640442,
3.37126493469603));
#26483=CARTESIAN_POINT('Ctrl Pts',(-0.0844857550745595,-0.122971699960107,
3.36336770017019));
#26484=CARTESIAN_POINT('Ctrl Pts',(-0.14915601679542,0.00351631274646034,
3.35547046564435));
#26485=CARTESIAN_POINT('Ctrl Pts',(-0.0785970697591793,0.126816333439056,
3.34757323111852));
#26486=CARTESIAN_POINT('Ctrl Pts',(0.0632202802738586,0.13514095590797,
3.33967599659268));
#26487=CARTESIAN_POINT('Ctrl Pts',(0.147720274543826,0.0209428338656845,
3.33177876206685));
#26488=CARTESIAN_POINT('Ctrl Pts',(0.0982927459879567,-0.112242674094044,
3.32388152754101));
#26489=CARTESIAN_POINT('Ctrl Pts',(-0.0402498618796406,-0.143665689781173,
3.31598429301518));
#26490=CARTESIAN_POINT('Ctrl Pts',(-0.142300767357216,-0.0448371878152361,
3.30808705848934));
#26491=CARTESIAN_POINT('Ctrl Pts',(-0.115337633785478,0.0946420204475735,
3.30018982396351));
#26492=CARTESIAN_POINT('Ctrl Pts',(0.0161939730658361,0.148316003984649,
3.29229258943767));
#26493=CARTESIAN_POINT('Ctrl Pts',(0.133043650140658,0.0675223589552513,
3.28439535491184));
#26494=CARTESIAN_POINT('Ctrl Pts',(0.129272061474707,-0.0744890322377149,
3.276498120386));
#26495=CARTESIAN_POINT('Ctrl Pts',(0.00829863969974947,-0.148966487441859,
3.26860088586017));
#26496=CARTESIAN_POINT('Ctrl Pts',(-0.120198571624367,-0.0883865667457073,
3.26070365133432));
#26497=CARTESIAN_POINT('Ctrl Pts',(-0.139720241205335,0.0523272013311878,
3.2528064168085));
#26498=CARTESIAN_POINT('Ctrl Pts',(-0.032567452245996,0.145599597718663,
3.24490918228265));
#26499=CARTESIAN_POINT('Ctrl Pts',(0.104111941761468,0.106867138935634,
3.23701194775683));
#26500=CARTESIAN_POINT('Ctrl Pts',(0.146400403313899,-0.0287541946706802,
3.22911471323098));
#26501=CARTESIAN_POINT('Ctrl Pts',(0.0559579759136239,-0.138306134112995,
3.22121747870515));
#26502=CARTESIAN_POINT('Ctrl Pts',(-0.085217589639859,-0.122465685878144,
3.21332024417931));
#26503=CARTESIAN_POINT('Ctrl Pts',(-0.149132395173076,0.00440573621240416,
3.20542300965348));
#26504=CARTESIAN_POINT('Ctrl Pts',(-0.077839408002832,0.127282788952003,
3.19752577512764));
#26505=CARTESIAN_POINT('Ctrl Pts',(0.0640250638484733,0.134761541252801,
3.18962854060181));
#26506=CARTESIAN_POINT('Ctrl Pts',(0.147842539602093,0.0200615374693747,
3.18173130607597));
#26507=CARTESIAN_POINT('Ctrl Pts',(0.0976216434508421,-0.112826843134018,
3.17383407155013));
#26508=CARTESIAN_POINT('Ctrl Pts',(-0.0411058908171925,-0.143423106721883,
3.1659368370243));
#26509=CARTESIAN_POINT('Ctrl Pts',(-0.142565621815174,-0.0439877855555886,
3.15803960249846));
#26510=CARTESIAN_POINT('Ctrl Pts',(-0.114771188963274,0.0953281489675947,
3.15014236797263));
#26511=CARTESIAN_POINT('Ctrl Pts',(0.0170781617196339,0.148216794574399,
3.14224513344679));
#26512=CARTESIAN_POINT('Ctrl Pts',(0.133443951323378,0.0667277577686799,
3.13434789892096));
#26513=CARTESIAN_POINT('Ctrl Pts',(0.128825550422286,-0.0752586165168258,
3.12645066439512));
#26514=CARTESIAN_POINT('Ctrl Pts',(0.00741013639610572,-0.149013327189962,
3.11855342986929));
#26515=CARTESIAN_POINT('Ctrl Pts',(-0.120723524088775,-0.0876681956767594,
3.11065619534345));
#26516=CARTESIAN_POINT('Ctrl Pts',(-0.139405705567482,0.0531594869883457,
3.10275896081762));
#26517=CARTESIAN_POINT('Ctrl Pts',(-0.0316985957176838,0.145791223436661,
3.09486172629178));
#26518=CARTESIAN_POINT('Ctrl Pts',(0.104747388431111,0.106244371232049,
3.08696449176594));
#26519=CARTESIAN_POINT('Ctrl Pts',(0.1462263255826,-0.0296267363751589,
3.07906725724011));
#26520=CARTESIAN_POINT('Ctrl Pts',(0.0551321977456556,-0.138637377980708,
3.07117002271428));
#26521=CARTESIAN_POINT('Ctrl Pts',(-0.0859463935972202,-0.121955316527256,
3.06327278818844));
#26522=CARTESIAN_POINT('Ctrl Pts',(-0.149103469929111,0.00529500299625034,
3.0553755536626));
#26523=CARTESIAN_POINT('Ctrl Pts',(-0.0770789780300003,0.127744717884859,
3.04747831913677));
#26524=CARTESIAN_POINT('Ctrl Pts',(0.064827570488531,0.134377334049259,
3.03958108461093));
#26525=CARTESIAN_POINT('Ctrl Pts',(0.147959546910171,0.0191795276211033,
3.0316838500851));
#26526=CARTESIAN_POINT('Ctrl Pts',(0.096947069178096,-0.11340699969318,
3.02378661555926));
#26527=CARTESIAN_POINT('Ctrl Pts',(-0.0419604578987403,-0.143175423081478,
3.01588938103343));
#26528=CARTESIAN_POINT('Ctrl Pts',(-0.142825406186904,-0.0431368189506033,
3.00799214650759));
#26529=CARTESIAN_POINT('Ctrl Pts',(-0.114200662513138,0.0960108873159227,
3.00009491198175));
#26530=CARTESIAN_POINT('Ctrl Pts',(0.0179617430197712,0.148112314104285,
2.99219767745592));
#26531=CARTESIAN_POINT('Ctrl Pts',(0.133839506815442,0.065930783531127,
2.98430044293008));
#26532=CARTESIAN_POINT('Ctrl Pts',(0.128374457924208,-0.0760255243605117,
2.97640320840425));
#26533=CARTESIAN_POINT('Ctrl Pts',(0.00652136956448273,-0.149054867551042,
2.96850597387841));
#26534=CARTESIAN_POINT('Ctrl Pts',(-0.121244183241318,-0.0869467068482327,
2.96060873935258));
#26535=CARTESIAN_POINT('Ctrl Pts',(-0.139086212220049,0.0539898821250478,
2.95271150482674));
#26536=CARTESIAN_POINT('Ctrl Pts',(-0.0308286118866713,0.145977664356358,
2.9448142703009));
#26537=CARTESIAN_POINT('Ctrl Pts',(0.10537910995104,0.105617825140169,2.93691703577507));
#26538=CARTESIAN_POINT('Ctrl Pts',(0.146047047578745,-0.0304982244567401,
2.92901980124923));
#26539=CARTESIAN_POINT('Ctrl Pts',(0.0543044589018171,-0.138963691467009,
2.9211225667234));
#26540=CARTESIAN_POINT('Ctrl Pts',(-0.0866721410281989,-0.121440610050369,
2.91322533219756));
#26541=CARTESIAN_POINT('Ctrl Pts',(-0.149069242091714,0.0061840814582022,
2.90532809767173));
#26542=CARTESIAN_POINT('Ctrl Pts',(-0.0763158068850386,0.128202103838321,
2.89743086314589));
#26543=CARTESIAN_POINT('Ctrl Pts',(0.0656277716564218,0.133988347906315,
2.88953362862006));
#26544=CARTESIAN_POINT('Ctrl Pts',(0.14807129230288,0.0182968357931569,
2.88163639409422));
#26545=CARTESIAN_POINT('Ctrl Pts',(0.0962690471674858,-0.113983123341786,
2.87373915956838));
#26546=CARTESIAN_POINT('Ctrl Pts',(-0.0428135327481091,-0.142922647278798,
2.86584192504255));
#26547=CARTESIAN_POINT('Ctrl Pts',(-0.14308011120489,-0.0422843190129418,
2.85794469051671));
#26548=CARTESIAN_POINT('Ctrl Pts',(-0.113626074780142,0.0966902126544859,
2.85004745599088));
#26549=CARTESIAN_POINT('Ctrl Pts',(0.0188446856497688,0.1480025635149,2.84215022146504));
#26550=CARTESIAN_POINT('Ctrl Pts',(0.134230302344763,0.0651314699250072,
2.8342529869392));
#26551=CARTESIAN_POINT('Ctrl Pts',(0.127918800416957,-0.0767897387687304,
2.82635575241337));
#26552=CARTESIAN_POINT('Ctrl Pts',(0.00563237005377145,-0.149091087280386,
2.81845851788753));
#26553=CARTESIAN_POINT('Ctrl Pts',(-0.121760529106313,-0.0862221639528271,
2.8105612833617));
#26554=CARTESIAN_POINT('Ctrl Pts',(-0.138761775333226,0.0548184303911556,
2.80266404883586));
#26555=CARTESIAN_POINT('Ctrl Pts',(-0.0299575262895149,0.146158773039815,
2.79476681431003));
#26556=CARTESIAN_POINT('Ctrl Pts',(0.106007073459698,0.104987793868287,
2.7868695797842));
#26557=CARTESIAN_POINT('Ctrl Pts',(0.145862595679981,-0.0313691492092156,
2.77897234525835));
#26558=CARTESIAN_POINT('Ctrl Pts',(0.0534747503335104,-0.139284059964419,
2.77107511073252));
#26559=CARTESIAN_POINT('Ctrl Pts',(-0.0873947320724949,-0.120923514621786,
2.76317787620668));
#26560=CARTESIAN_POINT('Ctrl Pts',(-0.149029855363559,0.00707665324264049,
2.75528064168085));
#26561=CARTESIAN_POINT('Ctrl Pts',(-0.0755496475001239,0.128647785709752,
2.74738340715502));
#26562=CARTESIAN_POINT('Ctrl Pts',(0.0664251107887961,0.133608345691969,
2.73948617262918));
#26563=CARTESIAN_POINT('Ctrl Pts',(0.148178792640495,0.0173870228536497,
2.73158893810334));
#26564=CARTESIAN_POINT('Ctrl Pts',(0.0955855932759896,-0.114504110894079,
2.72369170357751));
#26565=CARTESIAN_POINT('Ctrl Pts',(-0.0436608086765693,-0.142764488877777,
2.71579446905167));
#26566=CARTESIAN_POINT('Ctrl Pts',(-0.143341790816993,-0.0412252858023288,
2.70789723452584));
#26567=CARTESIAN_POINT('Ctrl Pts',(-0.123109488378236,0.0508267830136028,
2.70263241150861));
#26568=CARTESIAN_POINT('Ctrl Pts',(-0.0958116152722464,0.0825211298936403,
2.7));
#26569=CARTESIAN_POINT('Ctrl Pts',(-0.126320239448181,8.84447983197572E-5,
3.55565803263806));
#26570=CARTESIAN_POINT('Ctrl Pts',(-0.126416389705588,0.0147241557759941,
3.55473913135546));
#26571=CARTESIAN_POINT('Ctrl Pts',(-0.124064907197002,0.029329993953288,
3.55382023007285));
#26572=CARTESIAN_POINT('Ctrl Pts',(-0.119129449584441,0.0430029699128602,
3.55290132879025));
#26573=CARTESIAN_POINT('Ctrl Pts',(-0.104990656151973,0.0821724649982754,
3.55026891728164));
#26574=CARTESIAN_POINT('Ctrl Pts',(-0.0696458913257897,0.113686217010605,
3.54763650577302));
#26575=CARTESIAN_POINT('Ctrl Pts',(-0.0291183734446862,0.123260046955014,
3.54500409426441));
#26576=CARTESIAN_POINT('Ctrl Pts',(0.011409144436417,0.132833876899423,
3.5423716827558));
#26577=CARTESIAN_POINT('Ctrl Pts',(0.0571194153724406,0.120467784775912,
3.53973927124719));
#26578=CARTESIAN_POINT('Ctrl Pts',(0.0872917826964029,0.0917667392324598,
3.53710685973857));
#26579=CARTESIAN_POINT('Ctrl Pts',(0.117464150020365,0.0630656936890069,
3.53447444822996));
#26580=CARTESIAN_POINT('Ctrl Pts',(0.132098613732267,0.0180296947256118,
3.53184203672135));
#26581=CARTESIAN_POINT('Ctrl Pts',(0.124560909005821,-0.0229253845740426,
3.52920962521274));
#26582=CARTESIAN_POINT('Ctrl Pts',(0.117023204279375,-0.0638804638736969,
3.52657721370413));
#26583=CARTESIAN_POINT('Ctrl Pts',(0.0873133311145834,-0.100754623509611,
3.52394480219552));
#26584=CARTESIAN_POINT('Ctrl Pts',(0.048899338704955,-0.116832473273098,
3.5213123906869));
#26585=CARTESIAN_POINT('Ctrl Pts',(0.0104853462953266,-0.132910323036586,
3.51867997917829));
#26586=CARTESIAN_POINT('Ctrl Pts',(-0.0366327653591382,-0.128191862927647,
3.51604756766968));
#26587=CARTESIAN_POINT('Ctrl Pts',(-0.0710957340475621,-0.104815932991145,
3.51341515616107));
#26588=CARTESIAN_POINT('Ctrl Pts',(-0.104947268304411,-0.0818547336764444,
3.51082944832006));
#26589=CARTESIAN_POINT('Ctrl Pts',(-0.126588725667586,-0.0408922251827605,
3.50824374047906));
#26590=CARTESIAN_POINT('Ctrl Pts',(-0.12665116202208,1.34725138570783E-5,
3.50565803263806));
#26591=CARTESIAN_POINT('Ctrl Pts',(-0.0398513841857247,-0.149064942821851,
3.6));
#26592=CARTESIAN_POINT('Ctrl Pts',(-0.0498814435786606,-0.145400000402268,
3.6));
#26593=CARTESIAN_POINT('Ctrl Pts',(-0.059436150936811,-0.14063603073288,
3.6));
#26594=CARTESIAN_POINT('Ctrl Pts',(-0.0684043669488933,-0.134923276476459,
3.6));
#26595=CARTESIAN_POINT('Ctrl Pts',(-0.0756266237179617,-0.130322698385691,
3.6));
#26596=CARTESIAN_POINT('Ctrl Pts',(-0.0824683814027756,-0.125105404214097,
3.6));
#26597=CARTESIAN_POINT('Ctrl Pts',(-0.0888542192956036,-0.119334036703677,
3.6));
#26598=CARTESIAN_POINT('Ctrl Pts',(-0.091539386939335,-0.116907246428204,
3.6));
#26599=CARTESIAN_POINT('Ctrl Pts',(-0.0941378270474737,-0.114387469535812,
3.6));
#26600=CARTESIAN_POINT('Ctrl Pts',(-0.0966394276056281,-0.111785621852247,
3.6));
#26601=CARTESIAN_POINT('Ctrl Pts',(-0.103848676908048,-0.104287474901247,
3.6));
#26602=CARTESIAN_POINT('Ctrl Pts',(-0.110272002565724,-0.0960958678941195,
3.6));
#26603=CARTESIAN_POINT('Ctrl Pts',(-0.115776223647425,-0.0873309061633839,
3.6));
#26604=CARTESIAN_POINT('Ctrl Pts',(-0.118162872674894,-0.0835303888731155,
3.6));
#26605=CARTESIAN_POINT('Ctrl Pts',(-0.120376124201495,-0.0796218141710604,
3.6));
#26606=CARTESIAN_POINT('Ctrl Pts',(-0.122402049312502,-0.0756142631648066,
3.6));
#26607=CARTESIAN_POINT('Ctrl Pts',(-0.123825086107396,-0.0727993059344893,
3.6));
#26608=CARTESIAN_POINT('Ctrl Pts',(-0.125154691418473,-0.0699368314187636,
3.6));
#26609=CARTESIAN_POINT('Ctrl Pts',(-0.126381872197889,-0.0670411886576404,
3.6));
#26610=CARTESIAN_POINT('Ctrl Pts',(-0.129549149387792,-0.0595677149679855,
3.6));
#26611=CARTESIAN_POINT('Ctrl Pts',(-0.132046086846552,-0.0518539539453467,
3.6));
#26612=CARTESIAN_POINT('Ctrl Pts',(-0.133799060139059,-0.0439576297154888,
3.6));
#26613=CARTESIAN_POINT('Ctrl Pts',(-0.135388531616607,-0.0367978046374413,
3.6));
#26614=CARTESIAN_POINT('Ctrl Pts',(-0.136365840160023,-0.0294873792206846,
3.6));
#26615=CARTESIAN_POINT('Ctrl Pts',(-0.13674259160829,-0.0221011370783161,
3.6));
#26616=CARTESIAN_POINT('Ctrl Pts',(-0.136915659814306,-0.0187081211187088,
3.6));
#26617=CARTESIAN_POINT('Ctrl Pts',(-0.136961265679344,-0.0153067045798101,
3.6));
#26618=CARTESIAN_POINT('Ctrl Pts',(-0.136881936917631,-0.0119112232715221,
3.6));
#26619=CARTESIAN_POINT('Ctrl Pts',(-0.136684990383263,-0.0034813894794369,
3.6));
#26620=CARTESIAN_POINT('Ctrl Pts',(-0.135720534319688,0.00492632812693493,
3.6));
#26621=CARTESIAN_POINT('Ctrl Pts',(-0.134014244604164,0.0131981027910972,
3.6));
#26622=CARTESIAN_POINT('Ctrl Pts',(-0.133007067351581,0.0180807104774909,
3.6));
#26623=CARTESIAN_POINT('Ctrl Pts',(-0.131740913976379,0.0229158302155836,
3.6));
#26624=CARTESIAN_POINT('Ctrl Pts',(-0.130217237780107,0.0276776331326924,
3.6));
#26625=CARTESIAN_POINT('Ctrl Pts',(-0.129150755329031,0.0310106111361586,
3.6));
#26626=CARTESIAN_POINT('Ctrl Pts',(-0.127957851528495,0.0343071390648417,
3.6));
#26627=CARTESIAN_POINT('Ctrl Pts',(-0.126644351454204,0.0375455932808108,
3.6));
#26628=CARTESIAN_POINT('Ctrl Pts',(-0.12454778430103,0.0427147111736446,
3.6));
#26629=CARTESIAN_POINT('Ctrl Pts',(-0.122141614879321,0.0477447959908898,
3.6));
#26630=CARTESIAN_POINT('Ctrl Pts',(-0.11942949850221,0.0525991124010946,
3.6));
#26631=CARTESIAN_POINT('Ctrl Pts',(-0.116867678035268,0.0571844197417489,
3.6));
#26632=CARTESIAN_POINT('Ctrl Pts',(-0.11402973916396,0.0616160698651957,
3.6));
#26633=CARTESIAN_POINT('Ctrl Pts',(-0.110933547566151,0.0658375038383711,
3.6));
#26634=CARTESIAN_POINT('Ctrl Pts',(-0.107383747559623,0.0706774001665366,
3.6));
#26635=CARTESIAN_POINT('Ctrl Pts',(-0.103491800365401,0.0752476578095535,
3.6));
#26636=CARTESIAN_POINT('Ctrl Pts',(-0.0992594032733973,0.0794964740507377,
3.6));
#26637=CARTESIAN_POINT('Ctrl Pts',(-0.0981916513129811,0.080568368245057,
3.6));
#26638=CARTESIAN_POINT('Ctrl Pts',(-0.0971022039419119,0.081619760070457,
3.6));
#26639=CARTESIAN_POINT('Ctrl Pts',(-0.0959917963302726,0.0826503396631628,
3.6));
#26640=CARTESIAN_POINT('Origin',(0.,0.,3.1));
#26641=CARTESIAN_POINT('Origin',(0.,0.,2.6));
#26642=CARTESIAN_POINT('Origin',(4.61329551933804E-18,0.,1.7));
#26643=CARTESIAN_POINT('Ctrl Pts',(0.163512932725146,-0.0319230454628286,
1.7));
#26644=CARTESIAN_POINT('Ctrl Pts',(0.162868713265022,-0.0402193660776135,
1.7));
#26645=CARTESIAN_POINT('Ctrl Pts',(0.161556142957416,-0.0484298106643142,
1.7));
#26646=CARTESIAN_POINT('Ctrl Pts',(0.159633648446255,-0.0565030284772356,
1.7));
#26647=CARTESIAN_POINT('Ctrl Pts',(0.15857220935963,-0.0609603774536462,
1.7));
#26648=CARTESIAN_POINT('Ctrl Pts',(0.15732455882578,-0.0653759608776499,
1.7));
#26649=CARTESIAN_POINT('Ctrl Pts',(0.155898537051345,-0.0697413060244838,
1.7));
#26650=CARTESIAN_POINT('Ctrl Pts',(0.154359565759251,-0.0744524128122629,
1.7));
#26651=CARTESIAN_POINT('Ctrl Pts',(0.152615240924071,-0.0790971028454583,
1.7));
#26652=CARTESIAN_POINT('Ctrl Pts',(0.150679159438777,-0.0836586618069671,
1.7));
#26653=CARTESIAN_POINT('Ctrl Pts',(0.147458757270998,-0.0912461804520635,
1.7));
#26654=CARTESIAN_POINT('Ctrl Pts',(0.143706663154478,-0.098609365081655,
1.7));
#26655=CARTESIAN_POINT('Ctrl Pts',(0.139465780840256,-0.105699927668597,
1.7));
#26656=CARTESIAN_POINT('Ctrl Pts',(0.137613322919106,-0.108797153164702,
1.7));
#26657=CARTESIAN_POINT('Ctrl Pts',(0.135667748856481,-0.111841429389798,
1.7));
#26658=CARTESIAN_POINT('Ctrl Pts',(0.133638504154441,-0.114820282936825,
1.7));
#26659=CARTESIAN_POINT('Ctrl Pts',(0.126764362615545,-0.124911259587064,
1.7));
#26660=CARTESIAN_POINT('Ctrl Pts',(0.118918297697151,-0.134279562536914,
1.7));
#26661=CARTESIAN_POINT('Ctrl Pts',(0.110233695412878,-0.142776634038112,
1.7));
#26662=CARTESIAN_POINT('Ctrl Pts',(0.1060042704444,-0.146914731004415,1.7));
#26663=CARTESIAN_POINT('Ctrl Pts',(0.101575189643516,-0.150846009251356,
1.7));
#26664=CARTESIAN_POINT('Ctrl Pts',(0.0969579219100265,-0.154551255269456,
1.7));
#26665=CARTESIAN_POINT('Ctrl Pts',(0.0930558717128837,-0.157682556460965,
1.7));
#26666=CARTESIAN_POINT('Ctrl Pts',(0.089014879864356,-0.160654885938173,
1.7));
#26667=CARTESIAN_POINT('Ctrl Pts',(0.084867234382875,-0.163439189909414,
1.7));
#26668=CARTESIAN_POINT('Ctrl Pts',(0.0797924645177416,-0.166845870145637,
1.7));
#26669=CARTESIAN_POINT('Ctrl Pts',(0.0745525511585738,-0.169976381556328,
1.7));
#26670=CARTESIAN_POINT('Ctrl Pts',(0.069162704388918,-0.172812601917057,
1.7));
#26671=CARTESIAN_POINT('Ctrl Pts',(0.0615917910053332,-0.176796533113158,
1.7));
#26672=CARTESIAN_POINT('Ctrl Pts',(0.0537253644412386,-0.180200415745643,
1.7));
#26673=CARTESIAN_POINT('Ctrl Pts',(0.0456302879589726,-0.183039981733068,
1.7));
#26674=CARTESIAN_POINT('Ctrl Pts',(0.039725979220554,-0.185111076961087,
1.7));
#26675=CARTESIAN_POINT('Ctrl Pts',(0.0336998028892366,-0.186881755092485,
1.7));
#26676=CARTESIAN_POINT('Ctrl Pts',(0.027575472779275,-0.188354488495274,
1.7));
#26677=CARTESIAN_POINT('Ctrl Pts',(0.0240503901388611,-0.189202174178265,
1.7));
#26678=CARTESIAN_POINT('Ctrl Pts',(0.0204971902089821,-0.189949869388286,
1.7));
#26679=CARTESIAN_POINT('Ctrl Pts',(0.0169287682122467,-0.190597281499825,
1.7));
#26680=CARTESIAN_POINT('Ctrl Pts',(0.00540716645046445,-0.192687624102725,
1.7));
#26681=CARTESIAN_POINT('Ctrl Pts',(-0.00629626416002409,-0.193741044106324,
1.7));
#26682=CARTESIAN_POINT('Ctrl Pts',(-0.0180243092057446,-0.193790924616578,
1.7));
#26683=CARTESIAN_POINT('Ctrl Pts',(-0.0246815057039127,-0.193819238317361,
1.7));
#26684=CARTESIAN_POINT('Ctrl Pts',(-0.0313470218059255,-0.19352361589825,
1.7));
#26685=CARTESIAN_POINT('Ctrl Pts',(-0.0379937712674718,-0.192905366089908,
1.7));
#26686=CARTESIAN_POINT('Ctrl Pts',(-0.0421040672802865,-0.192523045417697,
1.7));
#26687=CARTESIAN_POINT('Ctrl Pts',(-0.0462092418665425,-0.192016959216387,
1.7));
#26688=CARTESIAN_POINT('Ctrl Pts',(-0.0502964475671879,-0.191387744025229,
1.7));
#26689=CARTESIAN_POINT('Ctrl Pts',(-0.0635557644152557,-0.189346505047739,
1.7));
#26690=CARTESIAN_POINT('Ctrl Pts',(-0.076538642829352,-0.186027878905466,
1.7));
#26691=CARTESIAN_POINT('Ctrl Pts',(-0.0890304894083597,-0.181464562959599,
1.7));
#26692=CARTESIAN_POINT('Ctrl Pts',(-0.0993708472336289,-0.177687193500922,
1.7));
#26693=CARTESIAN_POINT('Ctrl Pts',(-0.109375752092602,-0.173056097632409,
1.7));
#26694=CARTESIAN_POINT('Ctrl Pts',(-0.118921685270779,-0.167562801749516,
1.7));
#26695=CARTESIAN_POINT('Ctrl Pts',(-0.120076087508369,-0.166898490263086,
1.7));
#26696=CARTESIAN_POINT('Ctrl Pts',(-0.121223766120909,-0.16622153952215,
1.7));
#26697=CARTESIAN_POINT('Ctrl Pts',(-0.122364641233049,-0.165532117868825,
1.7));
#26698=CARTESIAN_POINT('Ctrl Pts',(-0.188262750966375,-0.0823232180103074,
1.7));
#26699=CARTESIAN_POINT('Ctrl Pts',(-0.190918693248964,-0.0742705707004131,
1.7));
#26700=CARTESIAN_POINT('Ctrl Pts',(-0.193028471001937,-0.0660604959755095,
1.7));
#26701=CARTESIAN_POINT('Ctrl Pts',(-0.194604369739905,-0.0577442961437627,
1.7));
#26702=CARTESIAN_POINT('Ctrl Pts',(-0.195791431603972,-0.0514800334494749,
1.7));
#26703=CARTESIAN_POINT('Ctrl Pts',(-0.196675380086104,-0.0451554970342283,
1.7));
#26704=CARTESIAN_POINT('Ctrl Pts',(-0.197258353741452,-0.0387928833243269,
1.7));
#26705=CARTESIAN_POINT('Ctrl Pts',(-0.197694864529353,-0.0340287752070089,
1.7));
#26706=CARTESIAN_POINT('Ctrl Pts',(-0.197962173616876,-0.0292446940334784,
1.7));
#26707=CARTESIAN_POINT('Ctrl Pts',(-0.198061149421263,-0.0244622127102265,
1.7));
#26708=CARTESIAN_POINT('Ctrl Pts',(-0.198268317226716,-0.0144519261913088,
1.7));
#26709=CARTESIAN_POINT('Ctrl Pts',(-0.197740578304783,-0.00443368324017007,
1.7));
#26710=CARTESIAN_POINT('Ctrl Pts',(-0.196485470149517,0.00550410801291526,
1.7));
#26711=CARTESIAN_POINT('Ctrl Pts',(-0.19583094903621,0.0106865252950324,
1.7));
#26712=CARTESIAN_POINT('Ctrl Pts',(-0.194977340636945,0.0158499464463904,
1.7));
#26713=CARTESIAN_POINT('Ctrl Pts',(-0.193930228257619,0.0209568152791792,
1.7));
#26714=CARTESIAN_POINT('Ctrl Pts',(-0.191365358848382,0.0334659326431063,
1.7));
#26715=CARTESIAN_POINT('Ctrl Pts',(-0.187640262305008,0.0456682931313192,
1.7));
#26716=CARTESIAN_POINT('Ctrl Pts',(-0.18276823303275,0.0573755743540122,
1.7));
#26717=CARTESIAN_POINT('Ctrl Pts',(-0.180530605205125,0.0627524998168591,
1.7));
#26718=CARTESIAN_POINT('Ctrl Pts',(-0.178050427357818,0.0680246443278264,
1.7));
#26719=CARTESIAN_POINT('Ctrl Pts',(-0.175326059031915,0.0731713030262629,
1.7));
#26720=CARTESIAN_POINT('Ctrl Pts',(-0.173546095954943,0.0765338668785476,
1.7));
#26721=CARTESIAN_POINT('Ctrl Pts',(-0.171660782837765,0.0798445731517242,
1.7));
#26722=CARTESIAN_POINT('Ctrl Pts',(-0.169672721187811,0.0830915804684565,
1.7));
#26723=CARTESIAN_POINT('Ctrl Pts',(-0.165401890376176,0.0900669269795776,
1.7));
#26724=CARTESIAN_POINT('Ctrl Pts',(-0.160674569826176,0.0967219627994757,
1.7));
#26725=CARTESIAN_POINT('Ctrl Pts',(-0.15549277623518,0.103004446710986,
1.7));
#26726=CARTESIAN_POINT('Ctrl Pts',(-0.149788864011586,0.109919955047648,
1.7));
#26727=CARTESIAN_POINT('Ctrl Pts',(-0.143534087392955,0.116384355174537,
1.7));
#26728=CARTESIAN_POINT('Ctrl Pts',(-0.1368007840805,0.122364607652698,1.7));
#26729=CARTESIAN_POINT('Ctrl Pts',(-0.132573081040691,0.126119485519849,
1.7));
#26730=CARTESIAN_POINT('Ctrl Pts',(-0.128156557788873,0.129683253321797,
1.7));
#26731=CARTESIAN_POINT('Ctrl Pts',(-0.123568264594465,0.133044997940945,
1.7));
#26732=CARTESIAN_POINT('Ctrl Pts',(-0.120777285576228,0.135089888774893,
1.7));
#26733=CARTESIAN_POINT('Ctrl Pts',(-0.117925900172203,0.137057490795076,
1.7));
#26734=CARTESIAN_POINT('Ctrl Pts',(-0.115025210475747,0.138941543144738,
1.7));
#26735=CARTESIAN_POINT('Ctrl Pts',(-0.106405133477763,0.144540444792911,
1.7));
#26736=CARTESIAN_POINT('Ctrl Pts',(-0.0973325886051703,0.149416450333531,
1.7));
#26737=CARTESIAN_POINT('Ctrl Pts',(-0.0879171639429846,0.15351829690281,
1.7));
#26738=CARTESIAN_POINT('Ctrl Pts',(-0.0791136675584941,0.157353555825057,
1.7));
#26739=CARTESIAN_POINT('Ctrl Pts',(-0.0700097444331976,0.160511945106675,
1.7));
#26740=CARTESIAN_POINT('Ctrl Pts',(-0.0606944403481407,0.162929898574301,
1.7));
#26741=CARTESIAN_POINT('Ctrl Pts',(-0.0571572012739495,0.163848052121106,
1.7));
#26742=CARTESIAN_POINT('Ctrl Pts',(-0.0535976091548405,0.16465702786045,
1.7));
#26743=CARTESIAN_POINT('Ctrl Pts',(-0.0500249348171965,0.165353504526832,
1.7));
#26744=CARTESIAN_POINT('Ctrl Pts',(-0.0389427731093366,0.16751392171383,
1.7));
#26745=CARTESIAN_POINT('Ctrl Pts',(-0.0277208597802445,0.168598940439913,
1.7));
#26746=CARTESIAN_POINT('Ctrl Pts',(-0.016510036378599,0.168511954471149,
1.7));
#26747=CARTESIAN_POINT('Ctrl Pts',(-0.0103145529256217,0.168463883057408,
1.7));
#26748=CARTESIAN_POINT('Ctrl Pts',(-0.00412256070196868,0.168057036314866,
1.7));
#26749=CARTESIAN_POINT('Ctrl Pts',(0.00203815650313415,0.16726854038896,
1.7));
#26750=CARTESIAN_POINT('Ctrl Pts',(0.00311390584534565,0.167130857722252,
1.7));
#26751=CARTESIAN_POINT('Ctrl Pts',(0.00418869523159273,0.166981526327298,
1.7));
#26752=CARTESIAN_POINT('Ctrl Pts',(0.00526237188779194,0.16682061735739,
1.7));
#26753=CARTESIAN_POINT('Origin',(0.,0.,0.645407471946233));
#26754=CARTESIAN_POINT('Ctrl Pts',(0.205654271051376,0.000148184871923513,
0.820407471946232));
#26755=CARTESIAN_POINT('Ctrl Pts',(0.20573642152142,0.00997667026911825,
0.820941869468311));
#26756=CARTESIAN_POINT('Ctrl Pts',(0.200629007389055,0.0878566204334846,
0.825180863342659));
#26757=CARTESIAN_POINT('Ctrl Pts',(0.101090873180113,0.220844643128561,
0.833124453569275));
#26758=CARTESIAN_POINT('Ctrl Pts',(-0.130696704329673,0.204681987270635,
0.844238242626078));
#26759=CARTESIAN_POINT('Ctrl Pts',(-0.242858579725743,0.00121498249237738,
0.855352031682883));
#26760=CARTESIAN_POINT('Ctrl Pts',(-0.132727951496213,-0.203386773400678,
0.866465820739686));
#26761=CARTESIAN_POINT('Ctrl Pts',(0.0988894015246068,-0.221814471640749,
0.877579609796491));
#26762=CARTESIAN_POINT('Ctrl Pts',(0.200212227802606,-0.0892608439806378,
0.885560160198673));
#26763=CARTESIAN_POINT('Ctrl Pts',(0.205725385245381,-0.0106740336596208,
0.889836114248587));
#26764=CARTESIAN_POINT('Ctrl Pts',(0.205635165348036,-0.000160487501855345,
0.890407471946233));
#26765=CARTESIAN_POINT('Ctrl Pts',(0.205269394176581,-0.000252214316689755,
0.814592528053767));
#26766=CARTESIAN_POINT('Ctrl Pts',(0.204912576919524,0.0467765744646069,
0.817137544740381));
#26767=CARTESIAN_POINT('Ctrl Pts',(0.165648098003252,0.162976258711784,
0.823387157779263));
#26768=CARTESIAN_POINT('Ctrl Pts',(-0.0272119409517698,0.241262826763902,
0.833341367170412));
#26769=CARTESIAN_POINT('Ctrl Pts',(-0.217470922739143,0.108102090643486,
0.844455156227217));
#26770=CARTESIAN_POINT('Ctrl Pts',(-0.208759451561279,-0.124141896006793,
0.85556894528402));
#26771=CARTESIAN_POINT('Ctrl Pts',(-0.00892472216375234,-0.242686445659381,
0.866682734340826));
#26772=CARTESIAN_POINT('Ctrl Pts',(0.172122246966409,-0.152544606240875,
0.87635726193074));
#26773=CARTESIAN_POINT('Ctrl Pts',(0.20498850808804,-0.0417917950361515,
0.882327193168388));
#26774=CARTESIAN_POINT('Ctrl Pts',(0.205205445749305,0.000116004416325009,
0.884592528053768));
#26775=CARTESIAN_POINT('Ctrl Pts',(-0.126907087985236,0.107935865304854,
0.8));
#26776=CARTESIAN_POINT('Ctrl Pts',(-0.162798331100657,0.0657362393039544,
0.803704596352268));
#26777=CARTESIAN_POINT('Ctrl Pts',(-0.188554427056889,-0.0565517713871986,
0.811113789056805));
#26778=CARTESIAN_POINT('Ctrl Pts',(-0.0544936724634594,-0.189356862721456,
0.822227578113607));
#26779=CARTESIAN_POINT('Ctrl Pts',(0.12941144825895,-0.14834225030535,0.833341367170414));
#26780=CARTESIAN_POINT('Ctrl Pts',(0.194879695227305,0.0282018585329969,
0.844455156227216));
#26781=CARTESIAN_POINT('Ctrl Pts',(0.0819649080024663,0.179061771725117,
0.855568945284021));
#26782=CARTESIAN_POINT('Ctrl Pts',(-0.105969441252334,0.165957021921342,
0.866682734340825));
#26783=CARTESIAN_POINT('Ctrl Pts',(-0.196910764727139,0.000985112949166876,
0.877796523397629));
#26784=CARTESIAN_POINT('Ctrl Pts',(-0.107616385055452,-0.164906857031527,
0.888910312454434));
#26785=CARTESIAN_POINT('Ctrl Pts',(0.0801799454629491,-0.179848112789142,
0.900024101511237));
#26786=CARTESIAN_POINT('Ctrl Pts',(0.194586948216313,-0.0301773643334041,
0.911137890568042));
#26787=CARTESIAN_POINT('Ctrl Pts',(0.13088616131906,0.147117686303235,0.922251679624846));
#26788=CARTESIAN_POINT('Ctrl Pts',(-0.0526161354638876,0.18975288262963,
0.93336546868165));
#26789=CARTESIAN_POINT('Ctrl Pts',(-0.187958327447607,0.0587058278606146,
0.944479257738454));
#26790=CARTESIAN_POINT('Ctrl Pts',(-0.151260109468812,-0.126075710016806,
0.955593046795258));
#26791=CARTESIAN_POINT('Ctrl Pts',(0.0238881910101356,-0.195458525846084,
0.966706835852062));
#26792=CARTESIAN_POINT('Ctrl Pts',(0.177171365146215,-0.0859360381031547,
0.977820624908868));
#26793=CARTESIAN_POINT('Ctrl Pts',(0.168287576475019,0.102244733060238,
0.98893441396567));
#26794=CARTESIAN_POINT('Ctrl Pts',(0.00536826212740452,0.196839712751384,
1.00004820302248));
#26795=CARTESIAN_POINT('Ctrl Pts',(-0.162464684252001,0.111265085550637,
1.01116199207928));
#26796=CARTESIAN_POINT('Ctrl Pts',(-0.181591862229106,-0.076151743861926,
1.02227578113608));
#26797=CARTESIAN_POINT('Ctrl Pts',(-0.0345059495415616,-0.193866014541413,
1.03338957019289));
#26798=CARTESIAN_POINT('Ctrl Pts',(0.144163650203206,-0.134132525587662,
1.04450335924969));
#26799=CARTESIAN_POINT('Ctrl Pts',(0.190878625928487,0.0483739862822188,
1.0556171483065));
#26800=CARTESIAN_POINT('Ctrl Pts',(0.062880230662697,0.186603239345861,
1.0667309373633));
#26801=CARTESIAN_POINT('Ctrl Pts',(-0.122673152855754,0.154032431506053,
1.07784472642011));
#26802=CARTESIAN_POINT('Ctrl Pts',(-0.195942408348395,-0.019526007891641,
1.08895851547691));
#26803=CARTESIAN_POINT('Ctrl Pts',(-0.0898633553462809,-0.175212070745787,
1.10007230453371));
#26804=CARTESIAN_POINT('Ctrl Pts',(0.0984686459264395,-0.170524538248248,
1.11118609359052));
#26805=CARTESIAN_POINT('Ctrl Pts',(0.196671178871044,-0.00975396199037572,
1.12229988264732));
#26806=CARTESIAN_POINT('Ctrl Pts',(0.114858351392768,0.159944526283292,
1.13341367170412));
#26807=CARTESIAN_POINT('Ctrl Pts',(-0.0720856276979479,0.183243975761544,
1.14452746076093));
#26808=CARTESIAN_POINT('Ctrl Pts',(-0.193048814249935,0.0388181360941049,
1.15564124981773));
#26809=CARTESIAN_POINT('Ctrl Pts',(-0.13731223179659,-0.141138383766243,
1.16675503887454));
#26810=CARTESIAN_POINT('Ctrl Pts',(0.0441077936468435,-0.191909340348063,
1.17786882793134));
#26811=CARTESIAN_POINT('Ctrl Pts',(0.185155455348894,-0.0670235013089116,
1.18898261698815));
#26812=CARTESIAN_POINT('Ctrl Pts',(0.156728228964436,0.119209708576257,
1.20009640604495));
#26813=CARTESIAN_POINT('Ctrl Pts',(-0.0151541228101832,0.196328920271653,
1.21121019510176));
#26814=CARTESIAN_POINT('Ctrl Pts',(-0.173165734117196,0.0937460447209521,
1.22232398415856));
#26815=CARTESIAN_POINT('Ctrl Pts',(-0.172676785153749,-0.0946436487152594,
1.23343777321536));
#26816=CARTESIAN_POINT('Ctrl Pts',(-0.0141348164511399,-0.196404937150434,
1.24455156227217));
#26817=CARTESIAN_POINT('Ctrl Pts',(0.157344910048918,-0.118394559228326,
1.25566535132897));
#26818=CARTESIAN_POINT('Ctrl Pts',(0.184805055968556,0.0679837014410847,
1.26677914038578));
#26819=CARTESIAN_POINT('Ctrl Pts',(0.0431110383282961,0.192135709193865,
1.27789292944258));
#26820=CARTESIAN_POINT('Ctrl Pts',(-0.138043001606285,0.140423723354349,
1.28900671849938));
#26821=CARTESIAN_POINT('Ctrl Pts',(-0.192844716656512,-0.0398196889847226,
1.30012050755619));
#26822=CARTESIAN_POINT('Ctrl Pts',(-0.0711334755432105,-0.183615688410121,
1.31123429661299));
#26823=CARTESIAN_POINT('Ctrl Pts',(0.115687042443292,-0.159346165890141,
1.32234808566979));
#26824=CARTESIAN_POINT('Ctrl Pts',(0.196617898501115,0.0107747093774004,
1.3334618747266));
#26825=CARTESIAN_POINT('Ctrl Pts',(0.0975821622623196,0.171033370958511,
1.3445756637834));
#26826=CARTESIAN_POINT('Ctrl Pts',(-0.0907716337523168,0.174743248450528,
1.35568945284021));
#26827=CARTESIAN_POINT('Ctrl Pts',(-0.196041123972824,0.0185086489133565,
1.36680324189701));
#26828=CARTESIAN_POINT('Ctrl Pts',(-0.121871950164007,-0.1546671268781,
1.37791703095382));
#26829=CARTESIAN_POINT('Ctrl Pts',(0.0638480017529153,-0.186274327390575,
1.38903082001062));
#26830=CARTESIAN_POINT('Ctrl Pts',(0.191127153577756,-0.0473825235535316,
1.40014460906743));
#26831=CARTESIAN_POINT('Ctrl Pts',(0.143465454207459,0.134879041457197,
1.41125839812423));
#26832=CARTESIAN_POINT('Ctrl Pts',(-0.0355118024153517,0.193684290169161,
1.42237218718103));
#26833=CARTESIAN_POINT('Ctrl Pts',(-0.181984703541769,0.0752081115995363,
1.43348597623784));
#26834=CARTESIAN_POINT('Ctrl Pts',(-0.16188494169705,-0.112106904510744,
1.44459976529464));
#26835=CARTESIAN_POINT('Ctrl Pts',(0.00638994323583646,-0.196809199398823,
1.45571355435144));
#26836=CARTESIAN_POINT('Ctrl Pts',(0.168816040557079,-0.101369802386164,
1.46682734340825));
#26837=CARTESIAN_POINT('Ctrl Pts',(0.17672290164568,0.0868545248928826,
1.47794113246505));
#26838=CARTESIAN_POINT('Ctrl Pts',(0.0228732863137639,0.195579919524334,
1.48905492152186));
#26839=CARTESIAN_POINT('Ctrl Pts',(-0.15191250667306,0.125288797732896,
1.50016871057866));
#26840=CARTESIAN_POINT('Ctrl Pts',(-0.187651060854054,-0.0596805852186566,
1.51128249963547));
#26841=CARTESIAN_POINT('Ctrl Pts',(-0.0516304683294577,-0.190023644566662,
1.52239628869227));
#26842=CARTESIAN_POINT('Ctrl Pts',(0.131648072412201,-0.146435920677088,
1.53351007774908));
#26843=CARTESIAN_POINT('Ctrl Pts',(0.194427649007747,0.0311862882363455,
1.54462386680588));
#26844=CARTESIAN_POINT('Ctrl Pts',(0.0792453752737409,0.180263283819487,
1.55573765586268));
#26845=CARTESIAN_POINT('Ctrl Pts',(-0.108471054243311,0.164343347185408,
1.56685144491949));
#26846=CARTESIAN_POINT('Ctrl Pts',(-0.196902764500876,-0.00200210229874768,
1.57796523397629));
#26847=CARTESIAN_POINT('Ctrl Pts',(-0.105107013422145,-0.16651465373019,
1.5890790230331));
#26848=CARTESIAN_POINT('Ctrl Pts',(0.0828941340502818,-0.178615126425815,
1.6001928120899));
#26849=CARTESIAN_POINT('Ctrl Pts',(0.195021809584276,-0.0272258612485208,
1.61130660114671));
#26850=CARTESIAN_POINT('Ctrl Pts',(0.128642913099457,0.149081079408297,
1.62242039020351));
#26851=CARTESIAN_POINT('Ctrl Pts',(-0.0554825813599488,0.188937135031884,
1.63353417926031));
#26852=CARTESIAN_POINT('Ctrl Pts',(-0.188827531603801,0.0558478560140352,
1.64464796831712));
#26853=CARTESIAN_POINT('Ctrl Pts',(-0.149330198326453,-0.128342305854753,
1.65576175737392));
#26854=CARTESIAN_POINT('Ctrl Pts',(0.0268386909069323,-0.195092411199392,
1.66687554643073));
#26855=CARTESIAN_POINT('Ctrl Pts',(0.178464943022445,-0.0832088009083063,
1.67798933548753));
#26856=CARTESIAN_POINT('Ctrl Pts',(0.166695798680381,0.104715122443915,
1.68910312454433));
#26857=CARTESIAN_POINT('Ctrl Pts',(0.00243441762381693,0.197027042329472,
1.70021691360114));
#26858=CARTESIAN_POINT('Ctrl Pts',(-0.164232046005026,0.108529764925501,
1.71133070265794));
#26859=CARTESIAN_POINT('Ctrl Pts',(-0.174839538171076,-0.0159901738299179,
1.71873989536248));
#26860=CARTESIAN_POINT('Ctrl Pts',(-0.152644235605294,-0.0667480137268189,
1.72244449171475));
#26861=CARTESIAN_POINT('Ctrl Pts',(-0.136778062465881,0.116331236980977,
0.792518502761751));
#26862=CARTESIAN_POINT('Ctrl Pts',(-0.175460966397852,0.0708492771249652,
0.796223099114019));
#26863=CARTESIAN_POINT('Ctrl Pts',(-0.203220400149799,-0.0609504310764289,
0.803632291818556));
#26864=CARTESIAN_POINT('Ctrl Pts',(-0.0587322509288797,-0.204085250153022,
0.814746080875359));
#26865=CARTESIAN_POINT('Ctrl Pts',(0.139477214667647,-0.159880475556692,
0.825859869932165));
#26866=CARTESIAN_POINT('Ctrl Pts',(0.210037654715023,0.0303954304627091,
0.836973658988967));
#26867=CARTESIAN_POINT('Ctrl Pts',(0.0883402297283485,0.192989395526265,
0.848087448045772));
#26868=CARTESIAN_POINT('Ctrl Pts',(-0.114211862278114,0.178865343704439,
0.859201237102576));
#26869=CARTESIAN_POINT('Ctrl Pts',(-0.212226703060007,0.00106173613023704,
0.87031502615938));
#26870=CARTESIAN_POINT('Ctrl Pts',(-0.115986907202372,-0.177733495821244,
0.881428815216186));
#26871=CARTESIAN_POINT('Ctrl Pts',(0.0864164308168349,-0.193836899073011,
0.892542604272987));
#26872=CARTESIAN_POINT('Ctrl Pts',(0.209722137515851,-0.0325245933019137,
0.903656393329794));
#26873=CARTESIAN_POINT('Ctrl Pts',(0.141066632550109,0.158560663604232,
0.914770182386597));
#26874=CARTESIAN_POINT('Ctrl Pts',(-0.0567086770128242,0.204512072930204,
0.925883971443401));
#26875=CARTESIAN_POINT('Ctrl Pts',(-0.20257793524978,0.0632720324586165,
0.936997760500206));
#26876=CARTESIAN_POINT('Ctrl Pts',(-0.163025289051846,-0.135882018994204,
0.948111549557009));
#26877=CARTESIAN_POINT('Ctrl Pts',(0.025746241081202,-0.210661507423248,
0.959225338613814));
#26878=CARTESIAN_POINT('Ctrl Pts',(0.190951951020682,-0.0926202387459321,
0.970339127670618));
#26879=CARTESIAN_POINT('Ctrl Pts',(0.181377171383915,0.110197442139303,
0.981452916727422));
#26880=CARTESIAN_POINT('Ctrl Pts',(0.00578581152757031,0.212150124582537,
0.992566705784226));
#26881=CARTESIAN_POINT('Ctrl Pts',(-0.175101368126144,0.119919407681051,
1.00368049484103));
#26882=CARTESIAN_POINT('Ctrl Pts',(-0.195716279284241,-0.0820749112141317,
1.01479428389783));
#26883=CARTESIAN_POINT('Ctrl Pts',(-0.0371898606828745,-0.208945128817718,
1.02590807295464));
#26884=CARTESIAN_POINT('Ctrl Pts',(0.15537685929014,-0.144565502642925,
1.03702186201144));
#26885=CARTESIAN_POINT('Ctrl Pts',(0.205725377795173,0.0521365687486478,
1.04813565106825));
#26886=CARTESIAN_POINT('Ctrl Pts',(0.0677711249544383,0.201117446888019,
1.05924944012505));
#26887=CARTESIAN_POINT('Ctrl Pts',(-0.132214807152008,0.166013245381199,
1.07036322918185));
#26888=CARTESIAN_POINT('Ctrl Pts',(-0.211183026844882,-0.0210447625070621,
1.08147701823866));
#26889=CARTESIAN_POINT('Ctrl Pts',(-0.0968530270931527,-0.188840260522183,
1.09259080729546));
#26890=CARTESIAN_POINT('Ctrl Pts',(0.106127646747548,-0.183788126532363,
1.10370459635227));
#26891=CARTESIAN_POINT('Ctrl Pts',(0.211968481949499,-0.0105126360047333,
1.11481838540907));
#26892=CARTESIAN_POINT('Ctrl Pts',(0.123792161737694,0.172385189467092,
1.12593217446588));
#26893=CARTESIAN_POINT('Ctrl Pts',(-0.0776925280115889,0.197496896045118,
1.13704596352268));
#26894=CARTESIAN_POINT('Ctrl Pts',(-0.208064365778478,0.0418374539025449,
1.14815975257949));
#26895=CARTESIAN_POINT('Ctrl Pts',(-0.147992529938032,-0.152116284264268,
1.15927354163629));
#26896=CARTESIAN_POINT('Ctrl Pts',(0.0475385469041886,-0.206836262328918,
1.17038733069309));
#26897=CARTESIAN_POINT('Ctrl Pts',(0.199557052641187,-0.0722366638006762,
1.1815011197499));
#26898=CARTESIAN_POINT('Ctrl Pts',(0.168918724964821,0.12848197232356,1.1926149088067));
#26899=CARTESIAN_POINT('Ctrl Pts',(-0.0163328273404871,0.211599602095504,
1.2037286978635));
#26900=CARTESIAN_POINT('Ctrl Pts',(-0.186634757554183,0.101037716366665,
1.21484248692031));
#26901=CARTESIAN_POINT('Ctrl Pts',(-0.18610777759643,-0.102005136998184,
1.22595627597711));
#26902=CARTESIAN_POINT('Ctrl Pts',(-0.0152342381989151,-0.211681531651681,
1.23707006503392));
#26903=CARTESIAN_POINT('Ctrl Pts',(0.169583372190078,-0.127603419752538,
1.24818385409072));
#26904=CARTESIAN_POINT('Ctrl Pts',(0.199179398807247,0.0732715493672994,
1.25929764314753));
#26905=CARTESIAN_POINT('Ctrl Pts',(0.046464262848129,0.207080238395369,
1.27041143220433));
#26906=CARTESIAN_POINT('Ctrl Pts',(-0.148780139836465,0.151346036770516,
1.28152522126114));
#26907=CARTESIAN_POINT('Ctrl Pts',(-0.207844393247192,-0.0429169086911673,
1.29263901031794));
#26908=CARTESIAN_POINT('Ctrl Pts',(-0.0766663164030391,-0.197897520917011,
1.30375279937474));
#26909=CARTESIAN_POINT('Ctrl Pts',(0.124685309300001,-0.171740287936918,
1.31486658843155));
#26910=CARTESIAN_POINT('Ctrl Pts',(0.211911057373125,0.0116127782590458,
1.32598037748835));
#26911=CARTESIAN_POINT('Ctrl Pts',(0.105172211397869,0.184336536816879,
1.33709416654516));
#26912=CARTESIAN_POINT('Ctrl Pts',(-0.0978319524040202,0.188334972707259,
1.34820795560196));
#26913=CARTESIAN_POINT('Ctrl Pts',(-0.211289420680394,0.0199482722156909,
1.35932174465877));
#26914=CARTESIAN_POINT('Ctrl Pts',(-0.131351286023602,-0.166697308065347,
1.37043553371557));
#26915=CARTESIAN_POINT('Ctrl Pts',(0.068814170356646,-0.200762951794954,
1.38154932277237));
#26916=CARTESIAN_POINT('Ctrl Pts',(0.205993236201476,-0.0510679889459757,
1.39266311182918));
#26917=CARTESIAN_POINT('Ctrl Pts',(0.154624356833139,0.14537008334725,1.40377690088598));
#26918=CARTESIAN_POINT('Ctrl Pts',(-0.0382739499121438,0.208749269721634,
1.41489068994279));
#26919=CARTESIAN_POINT('Ctrl Pts',(-0.196139676231217,0.0810578821846344,
1.42600447899959));
#26920=CARTESIAN_POINT('Ctrl Pts',(-0.174476532550337,-0.120826704256352,
1.43711826805639));
#26921=CARTESIAN_POINT('Ctrl Pts',(0.00688696012917997,-0.212117237867469,
1.4482320571132));
#26922=CARTESIAN_POINT('Ctrl Pts',(0.181946739990165,-0.109254458384087,
1.45934584617));
#26923=CARTESIAN_POINT('Ctrl Pts',(0.190468605530186,0.0936101664599312,
1.47045963522681));
#26924=CARTESIAN_POINT('Ctrl Pts',(0.0246523959685209,0.210792343236835,
1.48157342428361));
#26925=CARTESIAN_POINT('Ctrl Pts',(-0.163728430436396,0.135033899797455,
1.49268721334042));
#26926=CARTESIAN_POINT('Ctrl Pts',(-0.202246769118763,-0.0643226075283309,
1.50380100239722));
#26927=CARTESIAN_POINT('Ctrl Pts',(-0.0556463435921781,-0.204803895031906,
1.51491479145403));
#26928=CARTESIAN_POINT('Ctrl Pts',(0.141887805935659,-0.157825869489257,
1.52602858051082));
#26929=CARTESIAN_POINT('Ctrl Pts',(0.209550447837631,0.0336119924283981,
1.53714236956763));
#26930=CARTESIAN_POINT('Ctrl Pts',(0.0854091687186523,0.194284362567952,
1.54825615862443));
#26931=CARTESIAN_POINT('Ctrl Pts',(-0.116908053510435,0.177126155552421,
1.55936994768124));
#26932=CARTESIAN_POINT('Ctrl Pts',(-0.212218080567246,-0.00215782804277307,
1.57048373673804));
#26933=CARTESIAN_POINT('Ctrl Pts',(-0.113282353851889,-0.179466348735714,
1.58159752579485));
#26934=CARTESIAN_POINT('Ctrl Pts',(0.089341732011876,-0.192508009658716,
1.59271131485165));
#26935=CARTESIAN_POINT('Ctrl Pts',(0.210190822884773,-0.0293435190237031,
1.60382510390846));
#26936=CARTESIAN_POINT('Ctrl Pts',(0.138648901988495,0.160676771609172,
1.61493889296526));
#26937=CARTESIAN_POINT('Ctrl Pts',(-0.0597980782594448,0.203632875576831,
1.62605268202207));
#26938=CARTESIAN_POINT('Ctrl Pts',(-0.203514747072184,0.0601917643824736,
1.63716647107887));
#26939=CARTESIAN_POINT('Ctrl Pts',(-0.160945267273914,-0.13832491317789,
1.64828026013567));
#26940=CARTESIAN_POINT('Ctrl Pts',(0.0289262341422404,-0.210266915972054,
1.65939404919248));
#26941=CARTESIAN_POINT('Ctrl Pts',(0.19234614482316,-0.0896808740081667,
1.67050783824928));
#26942=CARTESIAN_POINT('Ctrl Pts',(0.179661583341645,0.112859981157414,
1.68162162730609));
#26943=CARTESIAN_POINT('Ctrl Pts',(0.00262376933475311,0.212352024863603,
1.69273541636289));
#26944=CARTESIAN_POINT('Ctrl Pts',(-0.177006197242412,0.116971330774799,
1.7038492054197));
#26945=CARTESIAN_POINT('Ctrl Pts',(-0.188438751949388,-0.0172339073385976,
1.71125839812423));
#26946=CARTESIAN_POINT('Ctrl Pts',(-0.164517074058987,-0.0719397484879835,
1.7149629944765));
#26947=CARTESIAN_POINT('Ctrl Pts',(-0.146649036946525,0.124726608657099,
0.785037005523502));
#26948=CARTESIAN_POINT('Ctrl Pts',(-0.188123601695047,0.0759623149459762,
0.78874160187577));
#26949=CARTESIAN_POINT('Ctrl Pts',(-0.217886373242709,-0.0653490907656594,
0.796150794580307));
#26950=CARTESIAN_POINT('Ctrl Pts',(-0.0629708293942997,-0.218813637584587,
0.807264583637111));
#26951=CARTESIAN_POINT('Ctrl Pts',(0.149542981076344,-0.171418700808033,
0.818378372693914));
#26952=CARTESIAN_POINT('Ctrl Pts',(0.225195614202741,0.0325890023924215,
0.829492161750719));
#26953=CARTESIAN_POINT('Ctrl Pts',(0.0947155514542305,0.206917019327413,
0.840605950807523));
#26954=CARTESIAN_POINT('Ctrl Pts',(-0.122454283303893,0.191773665487537,
0.851719739864327));
#26955=CARTESIAN_POINT('Ctrl Pts',(-0.227542641392875,0.00113835931130726,
0.862833528921131));
#26956=CARTESIAN_POINT('Ctrl Pts',(-0.124357429349293,-0.190560134610961,
0.873947317977936));
#26957=CARTESIAN_POINT('Ctrl Pts',(0.0926529161707207,-0.20782568535688,
0.885061107034739));
#26958=CARTESIAN_POINT('Ctrl Pts',(0.224857326815389,-0.0348718222704234,
0.896174896091545));
#26959=CARTESIAN_POINT('Ctrl Pts',(0.151247103781158,0.170003640905229,
0.907288685148347));
#26960=CARTESIAN_POINT('Ctrl Pts',(-0.0608012185617612,0.219271263230777,
0.918402474205154));
#26961=CARTESIAN_POINT('Ctrl Pts',(-0.217197543051952,0.0678382370566187,
0.929516263261956));
#26962=CARTESIAN_POINT('Ctrl Pts',(-0.174790468634879,-0.145688327971602,
0.940630052318761));
#26963=CARTESIAN_POINT('Ctrl Pts',(0.0276042911522686,-0.225864489000412,
0.951743841375564));
#26964=CARTESIAN_POINT('Ctrl Pts',(0.20473253689515,-0.0993044393887096,
0.962857630432368));
#26965=CARTESIAN_POINT('Ctrl Pts',(0.194466766292811,0.118150151218368,
0.973971419489174));
#26966=CARTESIAN_POINT('Ctrl Pts',(0.00620336092773602,0.227460536413689,
0.985085208545976));
#26967=CARTESIAN_POINT('Ctrl Pts',(-0.187738052000287,0.128573729811465,
0.996198997602783));
#26968=CARTESIAN_POINT('Ctrl Pts',(-0.209840696339377,-0.0879980785663373,
1.00731278665958));
#26969=CARTESIAN_POINT('Ctrl Pts',(-0.0398737718241875,-0.224024243094024,
1.01842657571639));
#26970=CARTESIAN_POINT('Ctrl Pts',(0.166590068377075,-0.154998479698188,
1.02954036477319));
#26971=CARTESIAN_POINT('Ctrl Pts',(0.22057212966186,0.055899151215077,1.04065415383));
#26972=CARTESIAN_POINT('Ctrl Pts',(0.0726620192461797,0.215631654430176,
1.0517679428868));
#26973=CARTESIAN_POINT('Ctrl Pts',(-0.141756461448261,0.177994059256345,
1.06288173194361));
#26974=CARTESIAN_POINT('Ctrl Pts',(-0.226423645341368,-0.0225635171224834,
1.07399552100041));
#26975=CARTESIAN_POINT('Ctrl Pts',(-0.103842698840025,-0.202468450298578,
1.08510931005722));
#26976=CARTESIAN_POINT('Ctrl Pts',(0.113786647568658,-0.197051714816478,
1.09622309911402));
#26977=CARTESIAN_POINT('Ctrl Pts',(0.227265785027954,-0.0112713100190907,
1.10733688817082));
#26978=CARTESIAN_POINT('Ctrl Pts',(0.132725972082619,0.184825852650891,
1.11845067722763));
#26979=CARTESIAN_POINT('Ctrl Pts',(-0.0832994283252297,0.211749816328691,
1.12956446628443));
#26980=CARTESIAN_POINT('Ctrl Pts',(-0.223079917307022,0.0448567717109849,
1.14067825534124));
#26981=CARTESIAN_POINT('Ctrl Pts',(-0.158672828079473,-0.163094184762292,
1.15179204439804));
#26982=CARTESIAN_POINT('Ctrl Pts',(0.0509693001615336,-0.221763184309772,
1.16290583345485));
#26983=CARTESIAN_POINT('Ctrl Pts',(0.213958649933481,-0.0774498262924409,
1.17401962251165));
#26984=CARTESIAN_POINT('Ctrl Pts',(0.181109220965206,0.137754236070862,
1.18513341156845));
#26985=CARTESIAN_POINT('Ctrl Pts',(-0.0175115318707909,0.226870283919355,
1.19624720062525));
#26986=CARTESIAN_POINT('Ctrl Pts',(-0.20010378099117,0.108329388012377,
1.20736098968206));
#26987=CARTESIAN_POINT('Ctrl Pts',(-0.199538770039111,-0.109366625281109,
1.21847477873886));
#26988=CARTESIAN_POINT('Ctrl Pts',(-0.0163336599466904,-0.226958126152927,
1.22958856779567));
#26989=CARTESIAN_POINT('Ctrl Pts',(0.181821834331238,-0.13681228027675,
1.24070235685247));
#26990=CARTESIAN_POINT('Ctrl Pts',(0.213553741645938,0.0785593972935142,
1.25181614590928));
#26991=CARTESIAN_POINT('Ctrl Pts',(0.0498174873679621,0.222024767596873,
1.26292993496608));
#26992=CARTESIAN_POINT('Ctrl Pts',(-0.159517278066646,0.162268350186683,
1.27404372402289));
#26993=CARTESIAN_POINT('Ctrl Pts',(-0.222844069837872,-0.0460141283976122,
1.28515751307969));
#26994=CARTESIAN_POINT('Ctrl Pts',(-0.0821991572628677,-0.212179353423901,
1.29627130213649));
#26995=CARTESIAN_POINT('Ctrl Pts',(0.13368357615671,-0.184134409983696,
1.3073850911933));
#26996=CARTESIAN_POINT('Ctrl Pts',(0.227204216245135,0.0124508471406916,
1.3184988802501));
#26997=CARTESIAN_POINT('Ctrl Pts',(0.112762260533419,0.197639702675246,
1.32961266930691));
#26998=CARTESIAN_POINT('Ctrl Pts',(-0.104892271055723,0.20192669696399,
1.34072645836371));
#26999=CARTESIAN_POINT('Ctrl Pts',(-0.226537717387964,0.0213878955180253,
1.35184024742052));
#27000=CARTESIAN_POINT('Ctrl Pts',(-0.140830621883197,-0.178727489252595,
1.36295403647732));
#27001=CARTESIAN_POINT('Ctrl Pts',(0.0737803389603765,-0.215251576199333,
1.37406782553412));
#27002=CARTESIAN_POINT('Ctrl Pts',(0.220859318825196,-0.0547534543384197,
1.38518161459093));
#27003=CARTESIAN_POINT('Ctrl Pts',(0.165783259458819,0.155861125237303,
1.39629540364773));
#27004=CARTESIAN_POINT('Ctrl Pts',(-0.0410360974089359,0.223814249274108,
1.40740919270454));
#27005=CARTESIAN_POINT('Ctrl Pts',(-0.210294648920666,0.0869076527697323,
1.41852298176134));
#27006=CARTESIAN_POINT('Ctrl Pts',(-0.187068123403623,-0.129546504001961,
1.42963677081815));
#27007=CARTESIAN_POINT('Ctrl Pts',(0.0073839770225235,-0.227425276336115,
1.44075055987495));
#27008=CARTESIAN_POINT('Ctrl Pts',(0.195077439423252,-0.117139114382011,
1.45186434893176));
#27009=CARTESIAN_POINT('Ctrl Pts',(0.204214309414691,0.10036580802698,1.46297813798855));
#27010=CARTESIAN_POINT('Ctrl Pts',(0.0264315056232782,0.226004766949337,
1.47409192704536));
#27011=CARTESIAN_POINT('Ctrl Pts',(-0.175544354199732,0.144779001862013,
1.48520571610217));
#27012=CARTESIAN_POINT('Ctrl Pts',(-0.216842477383471,-0.0689646298380053,
1.49631950515897));
#27013=CARTESIAN_POINT('Ctrl Pts',(-0.0596622188548986,-0.21958414549715,
1.50743329421577));
#27014=CARTESIAN_POINT('Ctrl Pts',(0.152127539459117,-0.169215818301425,
1.51854708327258));
#27015=CARTESIAN_POINT('Ctrl Pts',(0.224673246667516,0.0360376966204509,
1.52966087232938));
#27016=CARTESIAN_POINT('Ctrl Pts',(0.0915729621635637,0.208305441316416,
1.54077466138618));
#27017=CARTESIAN_POINT('Ctrl Pts',(-0.125345052777559,0.189908963919433,
1.55188845044299));
#27018=CARTESIAN_POINT('Ctrl Pts',(-0.227533396633615,-0.00231355378679829,
1.56300223949979));
#27019=CARTESIAN_POINT('Ctrl Pts',(-0.121457694281633,-0.192418043741239,
1.5741160285566));
#27020=CARTESIAN_POINT('Ctrl Pts',(0.09578932997347,-0.206400892891616,
1.5852298176134));
#27021=CARTESIAN_POINT('Ctrl Pts',(0.225359836185271,-0.0314611767988859,
1.59634360667021));
#27022=CARTESIAN_POINT('Ctrl Pts',(0.148654890877534,0.172272463810048,
1.60745739572701));
#27023=CARTESIAN_POINT('Ctrl Pts',(-0.0641135751589405,0.218328616121778,
1.61857118478381));
#27024=CARTESIAN_POINT('Ctrl Pts',(-0.218201962540567,0.0645356727509123,
1.62968497384062));
#27025=CARTESIAN_POINT('Ctrl Pts',(-0.172560336221374,-0.148307520501026,
1.64079876289742));
#27026=CARTESIAN_POINT('Ctrl Pts',(0.0310137773775485,-0.225441420744716,
1.65191255195423));
#27027=CARTESIAN_POINT('Ctrl Pts',(0.206227346623875,-0.0961529471080275,
1.66302634101103));
#27028=CARTESIAN_POINT('Ctrl Pts',(0.192627368002909,0.121004839870914,
1.67414013006784));
#27029=CARTESIAN_POINT('Ctrl Pts',(0.00281312104568935,0.227677007397733,
1.68525391912464));
#27030=CARTESIAN_POINT('Ctrl Pts',(-0.189780348479797,0.125412896624096,
1.69636770818145));
#27031=CARTESIAN_POINT('Ctrl Pts',(-0.202037965727701,-0.0184776408472769,
1.70377690088598));
#27032=CARTESIAN_POINT('Ctrl Pts',(-0.17638991251268,-0.0771314832491481,
1.70748149723825));
#27033=CARTESIAN_POINT('Ctrl Pts',(-0.156520011427169,0.133121980333222,
0.777555508285253));
#27034=CARTESIAN_POINT('Ctrl Pts',(-0.200786236992242,0.081075352766987,
0.781260104637521));
#27035=CARTESIAN_POINT('Ctrl Pts',(-0.232552346335619,-0.0697477504548899,
0.788669297342057));
#27036=CARTESIAN_POINT('Ctrl Pts',(-0.06720940785972,-0.233542025016153,
0.799783086398862));
#27037=CARTESIAN_POINT('Ctrl Pts',(0.159608747485041,-0.182956926059375,
0.810896875455666));
#27038=CARTESIAN_POINT('Ctrl Pts',(0.240353573690459,0.0347825743221341,
0.82201066451247));
#27039=CARTESIAN_POINT('Ctrl Pts',(0.101090873180113,0.220844643128561,
0.833124453569275));
#27040=CARTESIAN_POINT('Ctrl Pts',(-0.130696704329673,0.204681987270635,
0.844238242626078));
#27041=CARTESIAN_POINT('Ctrl Pts',(-0.242858579725743,0.00121498249237738,
0.855352031682883));
#27042=CARTESIAN_POINT('Ctrl Pts',(-0.132727951496213,-0.203386773400678,
0.866465820739686));
#27043=CARTESIAN_POINT('Ctrl Pts',(0.0988894015246068,-0.221814471640749,
0.877579609796491));
#27044=CARTESIAN_POINT('Ctrl Pts',(0.239992516114928,-0.0372190512389329,
0.888693398853296));
#27045=CARTESIAN_POINT('Ctrl Pts',(0.161427575012208,0.181446618206226,
0.899807187910099));
#27046=CARTESIAN_POINT('Ctrl Pts',(-0.0648937601106981,0.234030453531351,
0.910920976966904));
#27047=CARTESIAN_POINT('Ctrl Pts',(-0.231817150854124,0.0724044416546206,
0.922034766023707));
#27048=CARTESIAN_POINT('Ctrl Pts',(-0.186555648217912,-0.155494636948999,
0.933148555080512));
#27049=CARTESIAN_POINT('Ctrl Pts',(0.029462341223335,-0.241067470577576,
0.944262344137316));
#27050=CARTESIAN_POINT('Ctrl Pts',(0.218513122769618,-0.105988640031487,
0.95537613319412));
#27051=CARTESIAN_POINT('Ctrl Pts',(0.207556361201707,0.126102860297433,
0.966489922250924));
#27052=CARTESIAN_POINT('Ctrl Pts',(0.00662091032790181,0.242770948244842,
0.977603711307729));
#27053=CARTESIAN_POINT('Ctrl Pts',(-0.200374735874429,0.13722805194188,
0.988717500364533));
#27054=CARTESIAN_POINT('Ctrl Pts',(-0.223965113394512,-0.0939212459185429,
0.999831289421336));
#27055=CARTESIAN_POINT('Ctrl Pts',(-0.0425576829655005,-0.239103357370329,
1.01094507847814));
#27056=CARTESIAN_POINT('Ctrl Pts',(0.177803277464009,-0.16543145675345,
1.02205886753495));
#27057=CARTESIAN_POINT('Ctrl Pts',(0.235418881528546,0.0596617336815061,
1.03317265659175));
#27058=CARTESIAN_POINT('Ctrl Pts',(0.0775529135379212,0.230145861972334,
1.04428644564855));
#27059=CARTESIAN_POINT('Ctrl Pts',(-0.151298115744515,0.18997487313149,
1.05540023470536));
#27060=CARTESIAN_POINT('Ctrl Pts',(-0.241664263837854,-0.0240822717379046,
1.06651402376216));
#27061=CARTESIAN_POINT('Ctrl Pts',(-0.110832370586897,-0.216096640074974,
1.07762781281897));
#27062=CARTESIAN_POINT('Ctrl Pts',(0.121445648389767,-0.210315303100593,
1.08874160187577));
#27063=CARTESIAN_POINT('Ctrl Pts',(0.242563088106409,-0.0120299840334481,
1.09985539093258));
#27064=CARTESIAN_POINT('Ctrl Pts',(0.141659782427545,0.197266515834691,
1.11096917998938));
#27065=CARTESIAN_POINT('Ctrl Pts',(-0.0889063286388705,0.226002736612265,
1.12208296904618));
#27066=CARTESIAN_POINT('Ctrl Pts',(-0.238095468835566,0.0478760895194249,
1.13319675810299));
#27067=CARTESIAN_POINT('Ctrl Pts',(-0.169353126220915,-0.174072085260317,
1.14431054715979));
#27068=CARTESIAN_POINT('Ctrl Pts',(0.0544000534188783,-0.236690106290626,
1.1554243362166));
#27069=CARTESIAN_POINT('Ctrl Pts',(0.228360247225775,-0.0826629887842052,
1.1665381252734));
#27070=CARTESIAN_POINT('Ctrl Pts',(0.193299716965591,0.147026499818165,
1.1776519143302));
#27071=CARTESIAN_POINT('Ctrl Pts',(-0.0186902364010947,0.242140965743205,
1.18876570338701));
#27072=CARTESIAN_POINT('Ctrl Pts',(-0.213572804428157,0.115621059658089,
1.19987949244381));
#27073=CARTESIAN_POINT('Ctrl Pts',(-0.212969762481792,-0.116728113564033,
1.21099328150062));
#27074=CARTESIAN_POINT('Ctrl Pts',(-0.0174330816944656,-0.242234720654174,
1.22210707055742));
#27075=CARTESIAN_POINT('Ctrl Pts',(0.194060296472398,-0.146021140800962,
1.23322085961423));
#27076=CARTESIAN_POINT('Ctrl Pts',(0.227928084484629,0.0838472452197288,
1.24433464867103));
#27077=CARTESIAN_POINT('Ctrl Pts',(0.053170711887795,0.236969296798376,
1.25544843772783));
#27078=CARTESIAN_POINT('Ctrl Pts',(-0.170254416296827,0.17319066360285,
1.26656222678464));
#27079=CARTESIAN_POINT('Ctrl Pts',(-0.237843746428552,-0.0491113481040567,
1.27767601584144));
#27080=CARTESIAN_POINT('Ctrl Pts',(-0.0877319981226961,-0.226461185930791,
1.28878980489824));
#27081=CARTESIAN_POINT('Ctrl Pts',(0.142681843013418,-0.196528532030473,
1.29990359395505));
#27082=CARTESIAN_POINT('Ctrl Pts',(0.242497375117146,0.0132889160223372,
1.31101738301185));
#27083=CARTESIAN_POINT('Ctrl Pts',(0.120352309668968,0.210942868533614,
1.32213117206866));
#27084=CARTESIAN_POINT('Ctrl Pts',(-0.111952589707427,0.215518421220722,
1.33324496112546));
#27085=CARTESIAN_POINT('Ctrl Pts',(-0.241786014095534,0.0228275188203595,
1.34435875018226));
#27086=CARTESIAN_POINT('Ctrl Pts',(-0.150309957742793,-0.190757670439842,
1.35547253923907));
#27087=CARTESIAN_POINT('Ctrl Pts',(0.0787465075641072,-0.229740200603712,
1.36658632829588));
#27088=CARTESIAN_POINT('Ctrl Pts',(0.235725401448916,-0.0584389197308638,
1.37770011735268));
#27089=CARTESIAN_POINT('Ctrl Pts',(0.176942162084499,0.166352167127356,
1.38881390640948));
#27090=CARTESIAN_POINT('Ctrl Pts',(-0.0437982449057285,0.238879228826581,
1.39992769546629));
#27091=CARTESIAN_POINT('Ctrl Pts',(-0.224449621610114,0.0927574233548304,
1.41104148452309));
#27092=CARTESIAN_POINT('Ctrl Pts',(-0.199659714256911,-0.13826630374757,
1.42215527357989));
#27093=CARTESIAN_POINT('Ctrl Pts',(0.00788099391586731,-0.242733314804761,
1.4332690626367));
#27094=CARTESIAN_POINT('Ctrl Pts',(0.208208138856338,-0.125023770379934,
1.4443828516935));
#27095=CARTESIAN_POINT('Ctrl Pts',(0.217960013299196,0.107121449594028,
1.45549664075031));
#27096=CARTESIAN_POINT('Ctrl Pts',(0.028210615278035,0.241217190661839,
1.46661042980711));
#27097=CARTESIAN_POINT('Ctrl Pts',(-0.187360277963068,0.154524103926572,
1.47772421886392));
#27098=CARTESIAN_POINT('Ctrl Pts',(-0.23143818564818,-0.0736066521476796,
1.48883800792072));
#27099=CARTESIAN_POINT('Ctrl Pts',(-0.0636780941176189,-0.234364395962394,
1.49995179697753));
#27100=CARTESIAN_POINT('Ctrl Pts',(0.162367272982574,-0.180605767113594,
1.51106558603433));
#27101=CARTESIAN_POINT('Ctrl Pts',(0.2397960454974,0.0384634008125035,1.52217937509113));
#27102=CARTESIAN_POINT('Ctrl Pts',(0.0977367556084749,0.222326520064881,
1.53329316414794));
#27103=CARTESIAN_POINT('Ctrl Pts',(-0.133782052044684,0.202691772286445,
1.54440695320474));
#27104=CARTESIAN_POINT('Ctrl Pts',(-0.242848712699985,-0.00246927953082339,
1.55552074226155));
#27105=CARTESIAN_POINT('Ctrl Pts',(-0.129633034711377,-0.205369738746763,
1.56663453131835));
#27106=CARTESIAN_POINT('Ctrl Pts',(0.102236927935064,-0.220293776124516,
1.57774832037515));
#27107=CARTESIAN_POINT('Ctrl Pts',(0.240528849485768,-0.0335788345740686,
1.58886210943196));
#27108=CARTESIAN_POINT('Ctrl Pts',(0.158660879766572,0.183868156010923,
1.59997589848876));
#27109=CARTESIAN_POINT('Ctrl Pts',(-0.0684290720584363,0.233024356666725,
1.61108968754557));
#27110=CARTESIAN_POINT('Ctrl Pts',(-0.23288917800895,0.0688795811193509,
1.62220347660237));
#27111=CARTESIAN_POINT('Ctrl Pts',(-0.184175405168835,-0.158290127824162,
1.63331726565918));
#27112=CARTESIAN_POINT('Ctrl Pts',(0.0331013206128567,-0.240615925517378,
1.64443105471598));
#27113=CARTESIAN_POINT('Ctrl Pts',(0.220108548424591,-0.102625020207888,
1.65554484377279));
#27114=CARTESIAN_POINT('Ctrl Pts',(0.205593152664173,0.129149698584414,
1.66665863282959));
#27115=CARTESIAN_POINT('Ctrl Pts',(0.00300247275662535,0.243001989931863,
1.67777242188639));
#27116=CARTESIAN_POINT('Ctrl Pts',(-0.202554499717183,0.133854462473394,
1.6888862109432));
#27117=CARTESIAN_POINT('Ctrl Pts',(-0.215637179506013,-0.0197213743559566,
1.69629540364773));
#27118=CARTESIAN_POINT('Ctrl Pts',(-0.188262750966373,-0.0823232180103128,
1.7));
#27119=CARTESIAN_POINT('Ctrl Pts',(-0.126907087985236,0.107935865304854,
0.8));
#27120=CARTESIAN_POINT('Ctrl Pts',(-0.135120815820747,0.100273328983374,
0.8));
#27121=CARTESIAN_POINT('Ctrl Pts',(-0.142440162795362,0.0917707005673423,
0.8));
#27122=CARTESIAN_POINT('Ctrl Pts',(-0.148860420961125,0.0826220371750322,
0.8));
#27123=CARTESIAN_POINT('Ctrl Pts',(-0.153630780718642,0.0758244264629785,
0.8));
#27124=CARTESIAN_POINT('Ctrl Pts',(-0.157904437427575,0.0686688635836137,
0.8));
#27125=CARTESIAN_POINT('Ctrl Pts',(-0.161669292800466,0.0612205436816197,
0.8));
#27126=CARTESIAN_POINT('Ctrl Pts',(-0.163886790527543,0.0568334873893247,
0.8));
#27127=CARTESIAN_POINT('Ctrl Pts',(-0.165929164676721,0.0523396591094527,
0.8));
#27128=CARTESIAN_POINT('Ctrl Pts',(-0.167781485419322,0.0477808011974605,
0.8));
#27129=CARTESIAN_POINT('Ctrl Pts',(-0.172341905336402,0.0365568776388491,
0.8));
#27130=CARTESIAN_POINT('Ctrl Pts',(-0.175769282371032,0.024914892102173,
0.8));
#27131=CARTESIAN_POINT('Ctrl Pts',(-0.178035222124413,0.0130530737274266,
0.8));
#27132=CARTESIAN_POINT('Ctrl Pts',(-0.179475251863618,0.00551475714368376,
0.8));
#27133=CARTESIAN_POINT('Ctrl Pts',(-0.180445476974817,-0.00211322491662525,
0.8));
#27134=CARTESIAN_POINT('Ctrl Pts',(-0.180929041702956,-0.00978511330991493,
0.8));
#27135=CARTESIAN_POINT('Ctrl Pts',(-0.181154762272538,-0.0133662326867636,
0.8));
#27136=CARTESIAN_POINT('Ctrl Pts',(-0.181273901675413,-0.0169534510679824,
0.8));
#27137=CARTESIAN_POINT('Ctrl Pts',(-0.181285306139082,-0.0205319858475477,
0.8));
#27138=CARTESIAN_POINT('Ctrl Pts',(-0.18132084415518,-0.0316832359459324,
0.8));
#27139=CARTESIAN_POINT('Ctrl Pts',(-0.180314596981932,-0.0427772557222799,
0.8));
#27140=CARTESIAN_POINT('Ctrl Pts',(-0.178232649680767,-0.053673233795859,
0.8));
#27141=CARTESIAN_POINT('Ctrl Pts',(-0.177072367625385,-0.0597456294936455,
0.8));
#27142=CARTESIAN_POINT('Ctrl Pts',(-0.175577442236952,-0.0657567536750286,
0.8));
#27143=CARTESIAN_POINT('Ctrl Pts',(-0.173766632602371,-0.0716904360104152,
0.8));
#27144=CARTESIAN_POINT('Ctrl Pts',(-0.17263375533703,-0.0754026615746807,
0.8));
#27145=CARTESIAN_POINT('Ctrl Pts',(-0.171376588698951,-0.0790860937830887,
0.8));
#27146=CARTESIAN_POINT('Ctrl Pts',(-0.17000084111904,-0.0827319119339195,
0.8));
#27147=CARTESIAN_POINT('Ctrl Pts',(-0.165618690539351,-0.0943448882941177,
0.8));
#27148=CARTESIAN_POINT('Ctrl Pts',(-0.160069009775015,-0.105495622492882,
0.8));
#27149=CARTESIAN_POINT('Ctrl Pts',(-0.153517412526831,-0.116061366452211,
0.8));
#27150=CARTESIAN_POINT('Ctrl Pts',(-0.149177021710609,-0.123061103510275,
0.8));
#27151=CARTESIAN_POINT('Ctrl Pts',(-0.144395700078728,-0.129804236115551,
0.8));
#27152=CARTESIAN_POINT('Ctrl Pts',(-0.139210064136084,-0.136252864813496,
0.8));
#27153=CARTESIAN_POINT('Ctrl Pts',(-0.13649895134849,-0.139624285391187,
0.8));
#27154=CARTESIAN_POINT('Ctrl Pts',(-0.133675938748059,-0.142916515743411,
0.8));
#27155=CARTESIAN_POINT('Ctrl Pts',(-0.130749381376745,-0.146119375612755,
0.8));
#27156=CARTESIAN_POINT('Ctrl Pts',(-0.124483125872831,-0.152977241609597,
0.8));
#27157=CARTESIAN_POINT('Ctrl Pts',(-0.117767487241387,-0.159399582279811,
0.8));
#27158=CARTESIAN_POINT('Ctrl Pts',(-0.110656616745505,-0.165335584860524,
0.8));
#27159=CARTESIAN_POINT('Ctrl Pts',(-0.106173937599239,-0.169077629522446,
0.8));
#27160=CARTESIAN_POINT('Ctrl Pts',(-0.10153394483554,-0.172626328540978,
0.8));
#27161=CARTESIAN_POINT('Ctrl Pts',(-0.0967480797506452,-0.175967583788754,
0.8));
#27162=CARTESIAN_POINT('Ctrl Pts',(-0.0926327467056763,-0.178840706597052,
0.8));
#27163=CARTESIAN_POINT('Ctrl Pts',(-0.0884162860091264,-0.181555556620875,
0.8));
#27164=CARTESIAN_POINT('Ctrl Pts',(-0.0841104480426287,-0.184101786598396,
0.8));
#27165=CARTESIAN_POINT('Ctrl Pts',(-0.0753786167196158,-0.189265299681399,
0.8));
#27166=CARTESIAN_POINT('Ctrl Pts',(-0.0662752406232737,-0.193739549767325,
0.8));
#27167=CARTESIAN_POINT('Ctrl Pts',(-0.0568593821206139,-0.197450435399565,
0.8));
#27168=CARTESIAN_POINT('Ctrl Pts',(-0.0556199805901397,-0.197938896152316,
0.8));
#27169=CARTESIAN_POINT('Ctrl Pts',(-0.0543751496950137,-0.198414110578975,
0.8));
#27170=CARTESIAN_POINT('Ctrl Pts',(-0.0531250805644623,-0.198876136975596,
0.8));
#27171=CARTESIAN_POINT('Ctrl Pts',(0.166729862742343,-0.000130123946020723,
0.912851963660979));
#27172=CARTESIAN_POINT('Ctrl Pts',(0.166803013417109,-0.0086545516860567,
0.912280605963333));
#27173=CARTESIAN_POINT('Ctrl Pts',(0.166205714872852,-0.0171686904331816,
0.911709248265688));
#27174=CARTESIAN_POINT('Ctrl Pts',(0.164902316607877,-0.0255733139699205,
0.911137890568042));
#27175=CARTESIAN_POINT('Ctrl Pts',(0.156451280631859,-0.08006761381865,
0.907433294215774));
#27176=CARTESIAN_POINT('Ctrl Pts',(0.118315613047404,-0.129957863303896,
0.903728697863506));
#27177=CARTESIAN_POINT('Ctrl Pts',(0.0679483908354429,-0.152412778753583,
0.900024101511237));
#27178=CARTESIAN_POINT('Ctrl Pts',(0.017581168623482,-0.17486769420327,
0.896319505158969));
#27179=CARTESIAN_POINT('Ctrl Pts',(-0.045017608215985,-0.169887275617398,
0.892614908806701));
#27180=CARTESIAN_POINT('Ctrl Pts',(-0.0911993932476663,-0.139748404661014,
0.888910312454434));
#27181=CARTESIAN_POINT('Ctrl Pts',(-0.137381178279348,-0.109609533704629,
0.885205716102165));
#27182=CARTESIAN_POINT('Ctrl Pts',(-0.167145971503243,-0.0543122103777309,
0.881501119749897));
#27183=CARTESIAN_POINT('Ctrl Pts',(-0.16687148086939,0.000831769447747308,
0.877796523397629));
#27184=CARTESIAN_POINT('Ctrl Pts',(-0.166596990235537,0.0559757492732252,
0.874091927045361));
#27185=CARTESIAN_POINT('Ctrl Pts',(-0.136283215743936,0.110966385597283,
0.870387330693093));
#27186=CARTESIAN_POINT('Ctrl Pts',(-0.0898039369556689,0.140645828726608,
0.866682734340825));
#27187=CARTESIAN_POINT('Ctrl Pts',(-0.0433246581674013,0.170325271855933,
0.862978137988557));
#27188=CARTESIAN_POINT('Ctrl Pts',(0.0193201249175325,0.174693521790525,
0.859273541636289));
#27189=CARTESIAN_POINT('Ctrl Pts',(0.0694616476641393,0.151734327892468,
0.855568945284021));
#27190=CARTESIAN_POINT('Ctrl Pts',(0.119603170410746,0.12877513399441,0.851864348931753));
#27191=CARTESIAN_POINT('Ctrl Pts',(0.157241432819026,0.0784884962637034,
0.848159752579484));
#27192=CARTESIAN_POINT('Ctrl Pts',(0.16514918952844,0.0239211592586256,
0.844455156227216));
#27193=CARTESIAN_POINT('Ctrl Pts',(0.166289903708577,0.0160496809897125,
0.843920758705137));
#27194=CARTESIAN_POINT('Ctrl Pts',(0.16681196167645,0.00808912649634021,
0.843386361183058));
#27195=CARTESIAN_POINT('Ctrl Pts',(0.166745353727506,0.000120148921586877,
0.842851963660979));
#27196=CARTESIAN_POINT('Ctrl Pts',(0.0530170217188587,-0.198517432567173,
0.8));
#27197=CARTESIAN_POINT('Ctrl Pts',(0.119028790974553,-0.18088801151799,
0.803704596352268));
#27198=CARTESIAN_POINT('Ctrl Pts',(0.230942256426658,-0.0749063428374961,
0.811113789056804));
#27199=CARTESIAN_POINT('Ctrl Pts',(0.188114631577322,0.153856547759368,
0.822227578113608));
#27200=CARTESIAN_POINT('Ctrl Pts',(-0.0272119409517698,0.241262826763902,
0.833341367170412));
#27201=CARTESIAN_POINT('Ctrl Pts',(-0.217470922739143,0.108102090643486,
0.844455156227217));
#27202=CARTESIAN_POINT('Ctrl Pts',(-0.208759451561279,-0.124141896006793,
0.85556894528402));
#27203=CARTESIAN_POINT('Ctrl Pts',(-0.00892472216375234,-0.242686445659381,
0.866682734340826));
#27204=CARTESIAN_POINT('Ctrl Pts',(0.199056267666047,-0.139134372529335,
0.877796523397629));
#27205=CARTESIAN_POINT('Ctrl Pts',(0.224850619698646,0.091788306500609,
0.888910312454433));
#27206=CARTESIAN_POINT('Ctrl Pts',(0.0448304764247631,0.238686010114805,
0.900024101511237));
#27207=CARTESIAN_POINT('Ctrl Pts',(-0.176220286722883,0.167116974718297,
0.911137890568042));
#27208=CARTESIAN_POINT('Ctrl Pts',(-0.235976306336092,-0.0574188764093974,
0.922251679624847));
#27209=CARTESIAN_POINT('Ctrl Pts',(-0.0797396575425977,-0.229397140881452,
0.933365468681649));
#27210=CARTESIAN_POINT('Ctrl Pts',(0.14948314505928,-0.19140635164143,0.944479257738454));
#27211=CARTESIAN_POINT('Ctrl Pts',(0.241882569451173,0.0217812340617926,
0.955593046795258));
#27212=CARTESIAN_POINT('Ctrl Pts',(0.112884009708659,0.215032004451281,
0.966706835852063));
#27213=CARTESIAN_POINT('Ctrl Pts',(-0.119438498942156,0.211461649464463,
0.977820624908867));
#27214=CARTESIAN_POINT('Ctrl Pts',(-0.242437629122786,0.0143379927471741,
0.988934413965671));
#27215=CARTESIAN_POINT('Ctrl Pts',(-0.143530830111561,-0.195909362177039,
1.00004820302247));
#27216=CARTESIAN_POINT('Ctrl Pts',(0.086751356142284,-0.226838671363958,
1.01116199207928));
#27217=CARTESIAN_POINT('Ctrl Pts',(0.237629047152892,-0.05013996417456,
1.02227578113608));
#27218=CARTESIAN_POINT('Ctrl Pts',(0.1710021738693,0.172452416697446,1.03338957019289));
#27219=CARTESIAN_POINT('Ctrl Pts',(-0.0521449271278155,0.237197146991165,
1.04450335924969));
#27220=CARTESIAN_POINT('Ctrl Pts',(-0.227563185653378,0.0848326375129703,
1.0556171483065));
#27221=CARTESIAN_POINT('Ctrl Pts',(-0.194690279246867,-0.145180146557101,
1.0667309373633));
#27222=CARTESIAN_POINT('Ctrl Pts',(0.0163848475034698,-0.242307896337387,
1.0778447264201));
#27223=CARTESIAN_POINT('Ctrl Pts',(0.212462737615647,-0.117648480480376,
1.08895851547691));
#27224=CARTESIAN_POINT('Ctrl Pts',(0.214071074445423,0.114695923700636,
1.10007230453371));
#27225=CARTESIAN_POINT('Ctrl Pts',(0.019737729131079,0.242057848222183,
1.11118609359052));
#27226=CARTESIAN_POINT('Ctrl Pts',(-0.192661783512051,0.147861479120299,
1.12229988264732));
#27227=CARTESIAN_POINT('Ctrl Pts',(-0.228715780766039,-0.0816741786716276,
1.13341367170413));
#27228=CARTESIAN_POINT('Ctrl Pts',(-0.0554236300753314,-0.236452534483491,
1.14452746076093));
#27229=CARTESIAN_POINT('Ctrl Pts',(0.168598397772042,-0.174803203925221,
1.15564124981773));
#27230=CARTESIAN_POINT('Ctrl Pts',(0.238300400101745,0.0468454815872605,
1.16675503887454));
#27231=CARTESIAN_POINT('Ctrl Pts',(0.0898833437085198,0.225615966539919,
1.17786882793134));
#27232=CARTESIAN_POINT('Ctrl Pts',(-0.140804956527845,0.197877598659039,
1.18898261698814));
#27233=CARTESIAN_POINT('Ctrl Pts',(-0.242612883217311,-0.0109803793588139,
1.20009640604495));
#27234=CARTESIAN_POINT('Ctrl Pts',(-0.12235448648082,-0.2097878916237,1.21121019510175));
#27235=CARTESIAN_POINT('Ctrl Pts',(0.109896359325859,-0.21657416752884,
1.22232398415856));
#27236=CARTESIAN_POINT('Ctrl Pts',(0.241557821132076,-0.0251276517767584,
1.23343777321536));
#27237=CARTESIAN_POINT('Ctrl Pts',(0.152118669804104,0.189318488613562,
1.24455156227217));
#27238=CARTESIAN_POINT('Ctrl Pts',(-0.0765564251386213,0.230479269358191,
1.25566535132897));
#27239=CARTESIAN_POINT('Ctrl Pts',(-0.23515855594305,0.0606797610465845,
1.26677914038578));
#27240=CARTESIAN_POINT('Ctrl Pts',(-0.178517393613401,-0.164660620706261,
1.27789292944258));
#27241=CARTESIAN_POINT('Ctrl Pts',(0.0415227636155418,-0.239285268948212,
1.28900671849938));
#27242=CARTESIAN_POINT('Ctrl Pts',(0.223556664406995,-0.0948893968423596,
1.30012050755619));
#27243=CARTESIAN_POINT('Ctrl Pts',(0.200966614961749,0.136359816312279,
1.31123429661299));
#27244=CARTESIAN_POINT('Ctrl Pts',(-0.00557045627447471,0.242797343170749,
1.3223480856698));
#27245=CARTESIAN_POINT('Ctrl Pts',(-0.207008825709279,0.126999708315969,
1.3334618747266));
#27246=CARTESIAN_POINT('Ctrl Pts',(-0.218969669332857,-0.105042199835232,
1.3445756637834));
#27247=CARTESIAN_POINT('Ctrl Pts',(-0.0305050913306782,-0.240937791217362,
1.35568945284021));
#27248=CARTESIAN_POINT('Ctrl Pts',(0.185881142716884,-0.15630028987845,
1.36680324189701));
#27249=CARTESIAN_POINT('Ctrl Pts',(0.23212825880178,0.0714006393532108,
1.37791703095382));
#27250=CARTESIAN_POINT('Ctrl Pts',(0.0659057470887793,0.233747753644337,
1.38903082001062));
#27251=CARTESIAN_POINT('Ctrl Pts',(-0.160641042350602,0.182142898149225,
1.40014460906743));
#27252=CARTESIAN_POINT('Ctrl Pts',(-0.240151263944613,-0.0361794176709605,
1.41125839812423));
#27253=CARTESIAN_POINT('Ctrl Pts',(-0.0998483101275995,-0.221386302178844,
1.42237218718103));
#27254=CARTESIAN_POINT('Ctrl Pts',(0.131846934264022,-0.203955793640817,
1.43348597623784));
#27255=CARTESIAN_POINT('Ctrl Pts',(0.242861184558351,0.00015776588975909,
1.44459976529464));
#27256=CARTESIAN_POINT('Ctrl Pts',(0.13158183823911,0.204126920402922,1.45571355435144));
#27257=CARTESIAN_POINT('Ctrl Pts',(-0.10013585656473,0.221256389923926,
1.46682734340825));
#27258=CARTESIAN_POINT('Ctrl Pts',(-0.240198066802314,0.0358673761285168,
1.47794113246505));
#27259=CARTESIAN_POINT('Ctrl Pts',(-0.160404261381875,-0.182351453033287,
1.48905492152186));
#27260=CARTESIAN_POINT('Ctrl Pts',(0.0662093815164626,-0.233661930697804,
1.50016871057866));
#27261=CARTESIAN_POINT('Ctrl Pts',(0.232220830617013,-0.0710989904726924,
1.51128249963547));
#27262=CARTESIAN_POINT('Ctrl Pts',(0.185677912288661,0.156541656658069,
1.52239628869227));
#27263=CARTESIAN_POINT('Ctrl Pts',(-0.0308180903310451,0.240897960470908,
1.53351007774908));
#27264=CARTESIAN_POINT('Ctrl Pts',(-0.219105973246366,0.104757609325286,
1.54462386680588));
#27265=CARTESIAN_POINT('Ctrl Pts',(-0.206843620635952,-0.127268531807556,
1.55573765586268));
#27266=CARTESIAN_POINT('Ctrl Pts',(-0.00525505851706014,-0.242804414954791,
1.56685144491949));
#27267=CARTESIAN_POINT('Ctrl Pts',(0.201143714017778,-0.136098524667356,
1.57796523397629));
#27268=CARTESIAN_POINT('Ctrl Pts',(0.223432989115882,0.0951796228419585,
1.5890790230331));
#27269=CARTESIAN_POINT('Ctrl Pts',(0.041212233239435,0.2393392912824,1.6001928120899));
#27270=CARTESIAN_POINT('Ctrl Pts',(-0.178731921787321,0.164428017156146,
1.6113066011467));
#27271=CARTESIAN_POINT('Ctrl Pts',(-0.235078089364662,-0.0609842187918821,
1.62242039020351));
#27272=CARTESIAN_POINT('Ctrl Pts',(-0.0762596568913861,-0.230580482955351,
1.63353417926032));
#27273=CARTESIAN_POINT('Ctrl Pts',(0.15236975797671,-0.18911696954633,1.64464796831712));
#27274=CARTESIAN_POINT('Ctrl Pts',(0.241514918660579,0.0254343397173533,
1.65576175737392));
#27275=CARTESIAN_POINT('Ctrl Pts',(0.109634140470589,0.216730418270261,
1.66687554643072));
#27276=CARTESIAN_POINT('Ctrl Pts',(-0.122663843019391,0.209602590285094,
1.67798933548753));
#27277=CARTESIAN_POINT('Ctrl Pts',(-0.242556018767321,0.0107153659861808,
1.68910312454434));
#27278=CARTESIAN_POINT('Ctrl Pts',(-0.140685982558438,-0.198157528783211,
1.70021691360114));
#27279=CARTESIAN_POINT('Ctrl Pts',(0.0904627772969653,-0.225303732602113,
1.71133070265794));
#27280=CARTESIAN_POINT('Ctrl Pts',(0.188575434363683,-0.106431345694512,
1.71873989536248));
#27281=CARTESIAN_POINT('Ctrl Pts',(0.201667586144654,-0.0393720754290199,
1.72244449171475));
#27282=CARTESIAN_POINT('Ctrl Pts',(0.0496734897087673,-0.185997880000277,
0.792518502761751));
#27283=CARTESIAN_POINT('Ctrl Pts',(0.111522209883364,-0.169480262890401,
0.796223099114019));
#27284=CARTESIAN_POINT('Ctrl Pts',(0.216377824064917,-0.0701823552026538,
0.803632291818555));
#27285=CARTESIAN_POINT('Ctrl Pts',(0.176251134310715,0.144153545294923,
0.814746080875359));
#27286=CARTESIAN_POINT('Ctrl Pts',(-0.025495812948363,0.226047524998972,
0.825859869932164));
#27287=CARTESIAN_POINT('Ctrl Pts',(-0.203756063475674,0.101284604698293,
0.836973658988968));
#27288=CARTESIAN_POINT('Ctrl Pts',(-0.195593983451704,-0.116312855641356,
0.848087448045772));
#27289=CARTESIAN_POINT('Ctrl Pts',(-0.0083618822819891,-0.227381363005354,
0.859201237102576));
#27290=CARTESIAN_POINT('Ctrl Pts',(0.186502733326074,-0.130359827804384,
0.87031502615938));
#27291=CARTESIAN_POINT('Ctrl Pts',(0.210670357962369,0.0859996535173407,
0.881428815216184));
#27292=CARTESIAN_POINT('Ctrl Pts',(0.0420032309836913,0.223633215949719,
0.892542604272988));
#27293=CARTESIAN_POINT('Ctrl Pts',(-0.16510690935118,0.156577700042264,
0.903656393329793));
#27294=CARTESIAN_POINT('Ctrl Pts',(-0.221094400331606,-0.0537977403094414,
0.914770182386598));
#27295=CARTESIAN_POINT('Ctrl Pts',(-0.0747108556819193,-0.214930151626042,
0.925883971443401));
#27296=CARTESIAN_POINT('Ctrl Pts',(0.140055952352658,-0.179335261208594,
0.936997760500206));
#27297=CARTESIAN_POINT('Ctrl Pts',(0.226628183455449,0.0204075949748767,
0.948111549557009));
#27298=CARTESIAN_POINT('Ctrl Pts',(0.105764950816784,0.201470956192298,
0.959225338613814));
#27299=CARTESIAN_POINT('Ctrl Pts',(-0.111906079513391,0.198125766554245,
0.970339127670618));
#27300=CARTESIAN_POINT('Ctrl Pts',(-0.227148238147163,0.0134337635740443,
0.981452916727423));
#27301=CARTESIAN_POINT('Ctrl Pts',(-0.134479021666759,-0.183554288235144,
0.992566705784226));
#27302=CARTESIAN_POINT('Ctrl Pts',(0.0812803597193106,-0.212533032641853,
1.00368049484103));
#27303=CARTESIAN_POINT('Ctrl Pts',(0.222642910626845,-0.0469778745330203,
1.01479428389783));
#27304=CARTESIAN_POINT('Ctrl Pts',(0.160217878116906,0.161576661010844,
1.02590807295464));
#27305=CARTESIAN_POINT('Ctrl Pts',(-0.0488563939857563,0.222238248359082,
1.03702186201144));
#27306=CARTESIAN_POINT('Ctrl Pts',(-0.21321185525264,0.0794826455702088,
1.04813565106825));
#27307=CARTESIAN_POINT('Ctrl Pts',(-0.182412087081199,-0.136024323549586,
1.05924944012505));
#27308=CARTESIAN_POINT('Ctrl Pts',(0.0153515329125665,-0.227026686992996,
1.07036322918186));
#27309=CARTESIAN_POINT('Ctrl Pts',(0.199063720825595,-0.110228949022901,
1.08147701823866));
#27310=CARTESIAN_POINT('Ctrl Pts',(0.200570627482587,0.107462595990271,
1.09259080729546));
#27311=CARTESIAN_POINT('Ctrl Pts',(0.0184929642043311,0.226792408226016,
1.10370459635227));
#27312=CARTESIAN_POINT('Ctrl Pts',(-0.180511518947779,0.138536557190134,
1.11481838540907));
#27313=CARTESIAN_POINT('Ctrl Pts',(-0.214291761660261,-0.0765233757420587,
1.12593217446588));
#27314=CARTESIAN_POINT('Ctrl Pts',(-0.0519283246948251,-0.221540595029306,
1.13704596352268));
#27315=CARTESIAN_POINT('Ctrl Pts',(0.157965696772913,-0.163779195241938,
1.14815975257948));
#27316=CARTESIAN_POINT('Ctrl Pts',(0.22327192453058,0.0438911593311794,
1.15927354163629));
#27317=CARTESIAN_POINT('Ctrl Pts',(0.0842148276900768,0.211387438009701,
1.17038733069309));
#27318=CARTESIAN_POINT('Ctrl Pts',(-0.131925055996524,0.185398397380911,
1.1815011197499));
#27319=CARTESIAN_POINT('Ctrl Pts',(-0.227312439797474,-0.0102878989312292,
1.1926149088067));
#27320=CARTESIAN_POINT('Ctrl Pts',(-0.114638169553469,-0.196557564679025,
1.20372869786351));
#27321=CARTESIAN_POINT('Ctrl Pts',(0.102965717368131,-0.202915862361653,
1.21484248692031));
#27322=CARTESIAN_POINT('Ctrl Pts',(0.226323915472005,-0.0235429700022985,
1.22595627597712));
#27323=CARTESIAN_POINT('Ctrl Pts',(0.142525267056592,0.177379069795616,
1.23707006503392));
#27324=CARTESIAN_POINT('Ctrl Pts',(-0.071728374642188,0.215944035394125,
1.24818385409072));
#27325=CARTESIAN_POINT('Ctrl Pts',(-0.220328221575874,0.0568529764244717,
1.25929764314753));
#27326=CARTESIAN_POINT('Ctrl Pts',(-0.16725914860919,-0.154276256623111,
1.27041143220433));
#27327=CARTESIAN_POINT('Ctrl Pts',(0.0389041199272518,-0.224194682371805,
1.28152522126113));
#27328=CARTESIAN_POINT('Ctrl Pts',(0.209458006291536,-0.088905172804972,
1.29263901031794));
#27329=CARTESIAN_POINT('Ctrl Pts',(0.188292604081856,0.127760249683509,
1.30375279937474));
#27330=CARTESIAN_POINT('Ctrl Pts',(-0.0052191540273722,0.227485266736855,
1.31486658843155));
#27331=CARTESIAN_POINT('Ctrl Pts',(-0.193953761266,0.118990439287648,1.32598037748835));
#27332=CARTESIAN_POINT('Ctrl Pts',(-0.205160291232821,-0.0984176866850601,
1.33709416654516));
#27333=CARTESIAN_POINT('Ctrl Pts',(-0.028581279957875,-0.225742987902158,
1.34820795560196));
#27334=CARTESIAN_POINT('Ctrl Pts',(0.174158500995476,-0.146443172193371,
1.35932174465876));
#27335=CARTESIAN_POINT('Ctrl Pts',(0.217489030897462,0.0668977398036206,
1.37043553371557));
#27336=CARTESIAN_POINT('Ctrl Pts',(0.0617493843227067,0.219006391884312,
1.38154932277237));
#27337=CARTESIAN_POINT('Ctrl Pts',(-0.150510174002661,0.17065600977586,
1.39266311182918));
#27338=CARTESIAN_POINT('Ctrl Pts',(-0.225006063172667,-0.0338977534588365,
1.40377690088598));
#27339=CARTESIAN_POINT('Ctrl Pts',(-0.0935513509578539,-0.207424518511403,
1.41489068994279));
#27340=CARTESIAN_POINT('Ctrl Pts',(0.123531973693776,-0.191093269444383,
1.42600447899959));
#27341=CARTESIAN_POINT('Ctrl Pts',(0.22754508195105,0.000147816343643338,
1.43711826805639));
#27342=CARTESIAN_POINT('Ctrl Pts',(0.123283596017355,0.191253604053547,
1.4482320571132));
#27343=CARTESIAN_POINT('Ctrl Pts',(-0.0938207632055154,0.207302799206008,
1.45934584617));
#27344=CARTESIAN_POINT('Ctrl Pts',(-0.225049914396199,0.033605390895932,
1.4704596352268));
#27345=CARTESIAN_POINT('Ctrl Pts',(-0.150288325686177,-0.170851412092914,
1.48157342428361));
#27346=CARTESIAN_POINT('Ctrl Pts',(0.0620338699676892,-0.218925981383812,
1.49268721334041));
#27347=CARTESIAN_POINT('Ctrl Pts',(0.217575764647534,-0.066615114486764,
1.50380100239722));
#27348=CARTESIAN_POINT('Ctrl Pts',(0.173968087346094,0.146669317115412,
1.51491479145402));
#27349=CARTESIAN_POINT('Ctrl Pts',(-0.0288745395963744,0.225705669091897,
1.52602858051083));
#27350=CARTESIAN_POINT('Ctrl Pts',(-0.205287999105225,0.0981510439482811,
1.53714236956763));
#27351=CARTESIAN_POINT('Ctrl Pts',(-0.1937989748928,-0.119242309357106,
1.54825615862444));
#27352=CARTESIAN_POINT('Ctrl Pts',(-0.00492364691005069,-0.227491892537031,
1.55936994768124));
#27353=CARTESIAN_POINT('Ctrl Pts',(0.188458534340702,-0.127515436462881,
1.57048373673804));
#27354=CARTESIAN_POINT('Ctrl Pts',(0.209342130614232,0.0891770956278107,
1.58159752579485));
#27355=CARTESIAN_POINT('Ctrl Pts',(0.0386131732285934,0.224245297773695,
1.59271131485165));
#27356=CARTESIAN_POINT('Ctrl Pts',(-0.167460147509052,0.154058322275268,
1.60382510390846));
#27357=CARTESIAN_POINT('Ctrl Pts',(-0.220252829642796,-0.057138233464333,
1.61493889296526));
#27358=CARTESIAN_POINT('Ctrl Pts',(-0.0714503221602304,-0.21603886592994,
1.62605268202207));
#27359=CARTESIAN_POINT('Ctrl Pts',(0.14276052028949,-0.177190259579807,
1.63716647107887));
#27360=CARTESIAN_POINT('Ctrl Pts',(0.226283718655826,0.0238303165896214,
1.64828026013567));
#27361=CARTESIAN_POINT('Ctrl Pts',(0.102720035411913,0.203062259110174,
1.65939404919248));
#27362=CARTESIAN_POINT('Ctrl Pts',(-0.114928016442956,0.196383949416646,
1.67050783824928));
#27363=CARTESIAN_POINT('Ctrl Pts',(-0.227259161518541,0.0100395986945998,
1.68162162730609));
#27364=CARTESIAN_POINT('Ctrl Pts',(-0.131813585150871,-0.185660673640335,
1.69273541636289));
#27365=CARTESIAN_POINT('Ctrl Pts',(0.0847577191513361,-0.211094895184898,
1.70384920541969));
#27366=CARTESIAN_POINT('Ctrl Pts',(0.176682876451709,-0.0997192257060721,
1.71125839812423));
#27367=CARTESIAN_POINT('Ctrl Pts',(0.188949368338152,-0.0368890654402894,
1.7149629944765));
#27368=CARTESIAN_POINT('Ctrl Pts',(0.0463299576986758,-0.173478327433381,
0.785037005523502));
#27369=CARTESIAN_POINT('Ctrl Pts',(0.104015628792176,-0.158072514262811,
0.78874160187577));
#27370=CARTESIAN_POINT('Ctrl Pts',(0.201813391703176,-0.0654583675678116,
0.796150794580307));
#27371=CARTESIAN_POINT('Ctrl Pts',(0.164387637044107,0.134450542830478,
0.80726458363711));
#27372=CARTESIAN_POINT('Ctrl Pts',(-0.0237796849449563,0.210832223234042,
0.818378372693916));
#27373=CARTESIAN_POINT('Ctrl Pts',(-0.190041204212204,0.0944671187531002,
0.829492161750717));
#27374=CARTESIAN_POINT('Ctrl Pts',(-0.182428515342129,-0.10848381527592,
0.840605950807524));
#27375=CARTESIAN_POINT('Ctrl Pts',(-0.00779904240022581,-0.212076280351327,
0.851719739864326));
#27376=CARTESIAN_POINT('Ctrl Pts',(0.173949198986102,-0.121585283079433,
0.862833528921132));
#27377=CARTESIAN_POINT('Ctrl Pts',(0.196490096226091,0.0802110005340724,
0.873947317977935));
#27378=CARTESIAN_POINT('Ctrl Pts',(0.0391759855426195,0.208580421784633,
0.885061107034741));
#27379=CARTESIAN_POINT('Ctrl Pts',(-0.153993531979477,0.146038425366231,
0.896174896091543));
#27380=CARTESIAN_POINT('Ctrl Pts',(-0.206212494327119,-0.0501766042094856,
0.907288685148349));
#27381=CARTESIAN_POINT('Ctrl Pts',(-0.0696820538212414,-0.200463162370631,
0.918402474205152));
#27382=CARTESIAN_POINT('Ctrl Pts',(0.130628759646036,-0.167264170775759,
0.929516263261957));
#27383=CARTESIAN_POINT('Ctrl Pts',(0.211373797459724,0.0190339558879606,
0.94063005231876));
#27384=CARTESIAN_POINT('Ctrl Pts',(0.098645891924909,0.187909907933315,
0.951743841375565));
#27385=CARTESIAN_POINT('Ctrl Pts',(-0.104373660084627,0.184789883644027,
0.962857630432369));
#27386=CARTESIAN_POINT('Ctrl Pts',(-0.21185884717154,0.0125295344009149,
0.973971419489173));
#27387=CARTESIAN_POINT('Ctrl Pts',(-0.125427213221957,-0.17119921429325,
0.985085208545978));
#27388=CARTESIAN_POINT('Ctrl Pts',(0.0758093632963375,-0.198227393919747,
0.996198997602781));
#27389=CARTESIAN_POINT('Ctrl Pts',(0.207656774100798,-0.0438157848914807,
1.00731278665959));
#27390=CARTESIAN_POINT('Ctrl Pts',(0.149433582364513,0.150700905324243,
1.01842657571639));
#27391=CARTESIAN_POINT('Ctrl Pts',(-0.0455678608436973,0.207279349727,1.0295403647732));
#27392=CARTESIAN_POINT('Ctrl Pts',(-0.198860524851901,0.0741326536274474,
1.04065415383));
#27393=CARTESIAN_POINT('Ctrl Pts',(-0.170133894915531,-0.126868500542071,
1.0517679428868));
#27394=CARTESIAN_POINT('Ctrl Pts',(0.0143182183216636,-0.211745477648606,
1.06288173194361));
#27395=CARTESIAN_POINT('Ctrl Pts',(0.185664704035542,-0.102809417565425,
1.07399552100041));
#27396=CARTESIAN_POINT('Ctrl Pts',(0.187070180519752,0.100229268279905,
1.08510931005721));
#27397=CARTESIAN_POINT('Ctrl Pts',(0.017248199277583,0.211526968229848,
1.09622309911402));
#27398=CARTESIAN_POINT('Ctrl Pts',(-0.168361254383508,0.12921163525997,
1.10733688817082));
#27399=CARTESIAN_POINT('Ctrl Pts',(-0.199867742554481,-0.07137257281249,
1.11845067722763));
#27400=CARTESIAN_POINT('Ctrl Pts',(-0.0484330193143192,-0.206628655575122,
1.12956446628443));
#27401=CARTESIAN_POINT('Ctrl Pts',(0.147332995773784,-0.152755186558655,
1.14067825534124));
#27402=CARTESIAN_POINT('Ctrl Pts',(0.208243448959415,0.0409368370750985,
1.15179204439804));
#27403=CARTESIAN_POINT('Ctrl Pts',(0.0785463116716341,0.197158909479484,
1.16290583345485));
#27404=CARTESIAN_POINT('Ctrl Pts',(-0.123045155465202,0.172919196102783,
1.17401962251165));
#27405=CARTESIAN_POINT('Ctrl Pts',(-0.212011996377637,-0.00959541850364452,
1.18513341156845));
#27406=CARTESIAN_POINT('Ctrl Pts',(-0.106921852626119,-0.18332723773435,
1.19624720062526));
#27407=CARTESIAN_POINT('Ctrl Pts',(0.0960350754104022,-0.189257557194465,
1.20736098968206));
#27408=CARTESIAN_POINT('Ctrl Pts',(0.211090009811934,-0.0219582882278384,
1.21847477873886));
#27409=CARTESIAN_POINT('Ctrl Pts',(0.132931864309081,0.16543965097767,1.22958856779567));
#27410=CARTESIAN_POINT('Ctrl Pts',(-0.0669003241457547,0.201408801430058,
1.24070235685247));
#27411=CARTESIAN_POINT('Ctrl Pts',(-0.205497887208699,0.0530261918023587,
1.25181614590928));
#27412=CARTESIAN_POINT('Ctrl Pts',(-0.156000903604979,-0.143891892539961,
1.26292993496608));
#27413=CARTESIAN_POINT('Ctrl Pts',(0.0362854762389619,-0.209104095795397,
1.27404372402289));
#27414=CARTESIAN_POINT('Ctrl Pts',(0.195359348176077,-0.0829209487675844,
1.28515751307969));
#27415=CARTESIAN_POINT('Ctrl Pts',(0.175618593201963,0.119160683054738,
1.2962713021365));
#27416=CARTESIAN_POINT('Ctrl Pts',(-0.00486785178026968,0.212173190302961,
1.3073850911933));
#27417=CARTESIAN_POINT('Ctrl Pts',(-0.180898696822721,0.110981170259326,
1.3184988802501));
#27418=CARTESIAN_POINT('Ctrl Pts',(-0.191350913132785,-0.0917931735348885,
1.32961266930691));
#27419=CARTESIAN_POINT('Ctrl Pts',(-0.026657468585072,-0.210548184586953,
1.34072645836371));
#27420=CARTESIAN_POINT('Ctrl Pts',(0.162435859274068,-0.136586054508292,
1.35184024742051));
#27421=CARTESIAN_POINT('Ctrl Pts',(0.202849802993145,0.0623948402540306,
1.36295403647732));
#27422=CARTESIAN_POINT('Ctrl Pts',(0.057593021556634,0.204265030124287,
1.37406782553412));
#27423=CARTESIAN_POINT('Ctrl Pts',(-0.14037930565472,0.159169121402496,
1.38518161459093));
#27424=CARTESIAN_POINT('Ctrl Pts',(-0.209860862400721,-0.0316160892467124,
1.39629540364773));
#27425=CARTESIAN_POINT('Ctrl Pts',(-0.0872543917881084,-0.193462734843961,
1.40740919270454));
#27426=CARTESIAN_POINT('Ctrl Pts',(0.11521701312353,-0.178230745247949,
1.41852298176134));
#27427=CARTESIAN_POINT('Ctrl Pts',(0.212228979343748,0.000137866797527619,
1.42963677081814));
#27428=CARTESIAN_POINT('Ctrl Pts',(0.1149853537956,0.178380287704172,1.44075055987495));
#27429=CARTESIAN_POINT('Ctrl Pts',(-0.0875056698463009,0.19334920848809,
1.45186434893175));
#27430=CARTESIAN_POINT('Ctrl Pts',(-0.209901761990083,0.0313434056633472,
1.46297813798856));
#27431=CARTESIAN_POINT('Ctrl Pts',(-0.14017238999048,-0.159351371152542,
1.47409192704536));
#27432=CARTESIAN_POINT('Ctrl Pts',(0.0578583584189162,-0.204190032069821,
1.48520571610217));
#27433=CARTESIAN_POINT('Ctrl Pts',(0.202930698678054,-0.0621312385008357,
1.49631950515897));
#27434=CARTESIAN_POINT('Ctrl Pts',(0.162258262403527,0.136796977572755,
1.50743329421577));
#27435=CARTESIAN_POINT('Ctrl Pts',(-0.0269309888617035,0.210513377712887,
1.51854708327258));
#27436=CARTESIAN_POINT('Ctrl Pts',(-0.191470024964085,0.0915444785712757,
1.52966087232938));
#27437=CARTESIAN_POINT('Ctrl Pts',(-0.180754329149647,-0.111216086906656,
1.54077466138619));
#27438=CARTESIAN_POINT('Ctrl Pts',(-0.00459223530304152,-0.212179370119272,
1.55188845044299));
#27439=CARTESIAN_POINT('Ctrl Pts',(0.175773354663627,-0.118932348258406,
1.5630022394998));
#27440=CARTESIAN_POINT('Ctrl Pts',(0.195251272112581,0.0831745684136627,
1.5741160285566));
#27441=CARTESIAN_POINT('Ctrl Pts',(0.0360141132177518,0.20915130426499,
1.5852298176134));
#27442=CARTESIAN_POINT('Ctrl Pts',(-0.156188373230783,0.14368862739439,
1.59634360667021));
#27443=CARTESIAN_POINT('Ctrl Pts',(-0.20542756992093,-0.0532922481367839,
1.60745739572701));
#27444=CARTESIAN_POINT('Ctrl Pts',(-0.0666409874290749,-0.201497248904528,
1.61857118478382));
#27445=CARTESIAN_POINT('Ctrl Pts',(0.13315128260227,-0.165263549613285,
1.62968497384062));
#27446=CARTESIAN_POINT('Ctrl Pts',(0.211052518651072,0.0222262934618894,
1.64079876289742));
#27447=CARTESIAN_POINT('Ctrl Pts',(0.095805930353238,0.189394099950088,
1.65191255195423));
#27448=CARTESIAN_POINT('Ctrl Pts',(-0.107192189866521,0.183165308548198,
1.66302634101103));
#27449=CARTESIAN_POINT('Ctrl Pts',(-0.21196230426976,0.00936383140301889,
1.67414013006784));
#27450=CARTESIAN_POINT('Ctrl Pts',(-0.122941187743304,-0.173163818497459,
1.68525391912464));
#27451=CARTESIAN_POINT('Ctrl Pts',(0.0790526610057068,-0.196886057767682,
1.69636770818145));
#27452=CARTESIAN_POINT('Ctrl Pts',(0.164790318539736,-0.0930071057176319,
1.70377690088598));
#27453=CARTESIAN_POINT('Ctrl Pts',(0.176231150531649,-0.034406055451559,
1.70748149723825));
#27454=CARTESIAN_POINT('Ctrl Pts',(0.0429864256885843,-0.160958774866485,
0.777555508285253));
#27455=CARTESIAN_POINT('Ctrl Pts',(0.0965090477009877,-0.146664765635222,
0.781260104637521));
#27456=CARTESIAN_POINT('Ctrl Pts',(0.187248959341434,-0.0607343799329692,
0.788669297342056));
#27457=CARTESIAN_POINT('Ctrl Pts',(0.1525241397775,0.124747540366033,0.799783086398862));
#27458=CARTESIAN_POINT('Ctrl Pts',(-0.0220635569415495,0.195616921469113,
0.810896875455666));
#27459=CARTESIAN_POINT('Ctrl Pts',(-0.176326344948735,0.0876496328079073,
0.82201066451247));
#27460=CARTESIAN_POINT('Ctrl Pts',(-0.169263047232554,-0.100654774910484,
0.833124453569274));
#27461=CARTESIAN_POINT('Ctrl Pts',(-0.00723620251846265,-0.196771197697301,
0.844238242626078));
#27462=CARTESIAN_POINT('Ctrl Pts',(0.161395664646129,-0.112810738354482,
0.855352031682883));
#27463=CARTESIAN_POINT('Ctrl Pts',(0.182309834489814,0.0744223475508041,
0.866465820739686));
#27464=CARTESIAN_POINT('Ctrl Pts',(0.0363487401015477,0.193527627619547,
0.877579609796491));
#27465=CARTESIAN_POINT('Ctrl Pts',(-0.142880154607774,0.135499150690198,
0.888693398853294));
#27466=CARTESIAN_POINT('Ctrl Pts',(-0.191330588322633,-0.0465554681095297,
0.8998071879101));
#27467=CARTESIAN_POINT('Ctrl Pts',(-0.0646532519605634,-0.185996173115221,
0.910920976966903));
#27468=CARTESIAN_POINT('Ctrl Pts',(0.121201566939414,-0.155193080342923,
0.922034766023707));
#27469=CARTESIAN_POINT('Ctrl Pts',(0.196119411464,0.0176603168010446,0.933148555080512));
#27470=CARTESIAN_POINT('Ctrl Pts',(0.0915268330330338,0.174348859674332,
0.944262344137316));
#27471=CARTESIAN_POINT('Ctrl Pts',(-0.0968412406558618,0.17145400073381,
0.95537613319412));
#27472=CARTESIAN_POINT('Ctrl Pts',(-0.196569456195918,0.0116253052277854,
0.966489922250924));
#27473=CARTESIAN_POINT('Ctrl Pts',(-0.116375404777155,-0.158844140351355,
0.977603711307728));
#27474=CARTESIAN_POINT('Ctrl Pts',(0.0703383668733642,-0.183921755197642,
0.988717500364533));
#27475=CARTESIAN_POINT('Ctrl Pts',(0.19267063757475,-0.0406536952499414,
0.999831289421336));
#27476=CARTESIAN_POINT('Ctrl Pts',(0.13864928661212,0.139825149637642,1.01094507847814));
#27477=CARTESIAN_POINT('Ctrl Pts',(-0.0422793277016381,0.192320451094917,
1.02205886753494));
#27478=CARTESIAN_POINT('Ctrl Pts',(-0.184509194451163,0.0687826616846859,
1.03317265659175));
#27479=CARTESIAN_POINT('Ctrl Pts',(-0.157855702749863,-0.117712677534557,
1.04428644564855));
#27480=CARTESIAN_POINT('Ctrl Pts',(0.0132849037307607,-0.196464268304215,
1.05540023470536));
#27481=CARTESIAN_POINT('Ctrl Pts',(0.172265687245489,-0.0953898861079487,
1.06651402376216));
#27482=CARTESIAN_POINT('Ctrl Pts',(0.173569733556916,0.0929959405695393,
1.07762781281897));
#27483=CARTESIAN_POINT('Ctrl Pts',(0.0160034343508349,0.196261528233681,
1.08874160187577));
#27484=CARTESIAN_POINT('Ctrl Pts',(-0.156210989819237,0.119886713329805,
1.09985539093257));
#27485=CARTESIAN_POINT('Ctrl Pts',(-0.185443723448703,-0.066221769882921,
1.11096917998938));
#27486=CARTESIAN_POINT('Ctrl Pts',(-0.0449377139338128,-0.191716716120937,
1.12208296904618));
#27487=CARTESIAN_POINT('Ctrl Pts',(0.136700294774655,-0.141731177875371,
1.13319675810299));
#27488=CARTESIAN_POINT('Ctrl Pts',(0.193214973388251,0.0379825148190173,
1.14431054715979));
#27489=CARTESIAN_POINT('Ctrl Pts',(0.0728777956531908,0.182930380949266,
1.1554243362166));
#27490=CARTESIAN_POINT('Ctrl Pts',(-0.11416525493388,0.160439994824655,
1.1665381252734));
#27491=CARTESIAN_POINT('Ctrl Pts',(-0.196711552957801,-0.00890293807605981,
1.1776519143302));
#27492=CARTESIAN_POINT('Ctrl Pts',(-0.0992055356987686,-0.170096910789675,
1.18876570338701));
#27493=CARTESIAN_POINT('Ctrl Pts',(0.0891044334526734,-0.175599252027278,
1.19987949244381));
#27494=CARTESIAN_POINT('Ctrl Pts',(0.195856104151863,-0.0203736064533785,
1.21099328150062));
#27495=CARTESIAN_POINT('Ctrl Pts',(0.12333846156157,0.153500232159725,1.22210707055742));
#27496=CARTESIAN_POINT('Ctrl Pts',(-0.0620722736493212,0.186873567465992,
1.23322085961422));
#27497=CARTESIAN_POINT('Ctrl Pts',(-0.190667552841524,0.0491994071802457,
1.24433464867103));
#27498=CARTESIAN_POINT('Ctrl Pts',(-0.144742658600767,-0.13350752845681,
1.25544843772783));
#27499=CARTESIAN_POINT('Ctrl Pts',(0.0336668325506717,-0.194013509218991,
1.26656222678464));
#27500=CARTESIAN_POINT('Ctrl Pts',(0.181260690060617,-0.0769367247301966,
1.27767601584144));
#27501=CARTESIAN_POINT('Ctrl Pts',(0.16294458232207,0.110561116425968,1.28878980489824));
#27502=CARTESIAN_POINT('Ctrl Pts',(-0.00451654953316709,0.196861113869068,
1.29990359395505));
#27503=CARTESIAN_POINT('Ctrl Pts',(-0.167843632379442,0.102971901231004,
1.31101738301185));
#27504=CARTESIAN_POINT('Ctrl Pts',(-0.177541535032749,-0.0851686603847167,
1.32213117206866));
#27505=CARTESIAN_POINT('Ctrl Pts',(-0.0247336572122691,-0.195353381271748,
1.33324496112546));
#27506=CARTESIAN_POINT('Ctrl Pts',(0.15071321755266,-0.126728936823214,
1.34435875018226));
#27507=CARTESIAN_POINT('Ctrl Pts',(0.188210575088826,0.0578919407044404,
1.35547253923907));
#27508=CARTESIAN_POINT('Ctrl Pts',(0.0534366587905616,0.189523668364262,
1.36658632829587));
#27509=CARTESIAN_POINT('Ctrl Pts',(-0.130248437306779,0.147682233029131,
1.37770011735268));
#27510=CARTESIAN_POINT('Ctrl Pts',(-0.194715661628775,-0.0293344250345881,
1.38881390640948));
#27511=CARTESIAN_POINT('Ctrl Pts',(-0.0809574326183627,-0.17950095117652,
1.39992769546629));
#27512=CARTESIAN_POINT('Ctrl Pts',(0.106902052553284,-0.165368221051515,
1.41104148452309));
#27513=CARTESIAN_POINT('Ctrl Pts',(0.196912876736446,0.000127917251411783,
1.4221552735799));
#27514=CARTESIAN_POINT('Ctrl Pts',(0.106687111573845,0.165506971354797,
1.4332690626367));
#27515=CARTESIAN_POINT('Ctrl Pts',(-0.0811905764870862,0.179395617770172,
1.44438285169351));
#27516=CARTESIAN_POINT('Ctrl Pts',(-0.194753609583967,0.0290814204307625,
1.45549664075031));
#27517=CARTESIAN_POINT('Ctrl Pts',(-0.130056454294782,-0.14785133021217,
1.46661042980711));
#27518=CARTESIAN_POINT('Ctrl Pts',(0.053682846870143,-0.189454082755829,
1.47772421886392));
#27519=CARTESIAN_POINT('Ctrl Pts',(0.188285632708575,-0.0576473625149073,
1.48883800792072));
#27520=CARTESIAN_POINT('Ctrl Pts',(0.15054843746096,0.126924638030098,1.49995179697752));
#27521=CARTESIAN_POINT('Ctrl Pts',(-0.024987438127033,0.195321086333876,
1.51106558603433));
#27522=CARTESIAN_POINT('Ctrl Pts',(-0.177652050822945,0.0849379131942705,
1.52217937509113));
#27523=CARTESIAN_POINT('Ctrl Pts',(-0.167709683406495,-0.103189864456206,
1.53329316414794));
#27524=CARTESIAN_POINT('Ctrl Pts',(-0.00426082369603206,-0.196866847701512,
1.54440695320474));
#27525=CARTESIAN_POINT('Ctrl Pts',(0.163088174986552,-0.110349260053931,
1.55552074226154));
#27526=CARTESIAN_POINT('Ctrl Pts',(0.181160413610931,0.0771720411995148,
1.56663453131835));
#27527=CARTESIAN_POINT('Ctrl Pts',(0.03341505320691,0.194057310756286,1.57774832037515));
#27528=CARTESIAN_POINT('Ctrl Pts',(-0.144916598952513,0.133318932513512,
1.58886210943196));
#27529=CARTESIAN_POINT('Ctrl Pts',(-0.190602310199064,-0.049446262809235,
1.59997589848876));
#27530=CARTESIAN_POINT('Ctrl Pts',(-0.0618316526979189,-0.186955631879117,
1.61108968754557));
#27531=CARTESIAN_POINT('Ctrl Pts',(0.12354204491505,-0.153336839646763,
1.62220347660237));
#27532=CARTESIAN_POINT('Ctrl Pts',(0.195821318646319,0.0206222703341576,
1.63331726565918));
#27533=CARTESIAN_POINT('Ctrl Pts',(0.0888918252945621,0.175725940790001,
1.64443105471598));
#27534=CARTESIAN_POINT('Ctrl Pts',(-0.0994563632900866,0.16994666767975,
1.65554484377278));
#27535=CARTESIAN_POINT('Ctrl Pts',(-0.19666544702098,0.008688064111438,
1.66665863282959));
#27536=CARTESIAN_POINT('Ctrl Pts',(-0.114068790335738,-0.160666963354583,
1.67777242188639));
#27537=CARTESIAN_POINT('Ctrl Pts',(0.0733476028600775,-0.182677220350466,
1.6888862109432));
#27538=CARTESIAN_POINT('Ctrl Pts',(0.152897760627763,-0.0862949857291919,
1.69629540364773));
#27539=CARTESIAN_POINT('Ctrl Pts',(0.163512932725146,-0.0319230454628286,
1.7));
#27540=CARTESIAN_POINT('Ctrl Pts',(0.166381444272219,9.40568719243839E-5,
0.86214803633902));
#27541=CARTESIAN_POINT('Ctrl Pts',(0.166493197029431,0.0216823422355625,
0.863587297805909));
#27542=CARTESIAN_POINT('Ctrl Pts',(0.162594223870085,0.0432319486948127,
0.865026559272798));
#27543=CARTESIAN_POINT('Ctrl Pts',(0.154497290451155,0.0630677132447136,
0.866465820739686));
#27544=CARTESIAN_POINT('Ctrl Pts',(0.133656136360392,0.114124107573719,
0.870170417091954));
#27545=CARTESIAN_POINT('Ctrl Pts',(0.0850024382309698,0.153825867596633,
0.873875013444223));
#27546=CARTESIAN_POINT('Ctrl Pts',(0.0308041067147051,0.164005334786532,
0.877579609796491));
#27547=CARTESIAN_POINT('Ctrl Pts',(-0.0233942248015594,0.174184801976431,
0.881284206148759));
#27548=CARTESIAN_POINT('Ctrl Pts',(-0.0831371897046666,0.154841976333314,
0.884988802501027));
#27549=CARTESIAN_POINT('Ctrl Pts',(-0.12108374444203,0.114828127045135,
0.888693398853295));
#27550=CARTESIAN_POINT('Ctrl Pts',(-0.159030299179393,0.0748142777569551,
0.892397995205563));
#27551=CARTESIAN_POINT('Ctrl Pts',(-0.175180443751013,0.0141294048237127,
0.896102591557831));
#27552=CARTESIAN_POINT('Ctrl Pts',(-0.162142626643145,-0.039453149143857,
0.899807187910099));
#27553=CARTESIAN_POINT('Ctrl Pts',(-0.149104809535276,-0.0930357031114267,
0.903511784262367));
#27554=CARTESIAN_POINT('Ctrl Pts',(-0.10687903074792,-0.139515938113324,
0.907216380614635));
#27555=CARTESIAN_POINT('Ctrl Pts',(-0.0547903382042454,-0.157622206818889,
0.910920976966903));
#27556=CARTESIAN_POINT('Ctrl Pts',(-0.00270164566057092,-0.175728475524455,
0.914625573319171));
#27557=CARTESIAN_POINT('Ctrl Pts',(0.0592499606394216,-0.165460777933689,
0.918330169671439));
#27558=CARTESIAN_POINT('Ctrl Pts',(0.102712071210182,-0.131518029614312,
0.922034766023707));
#27559=CARTESIAN_POINT('Ctrl Pts',(0.142261505739626,-0.100630976850939,
0.925405856128812));
#27560=CARTESIAN_POINT('Ctrl Pts',(0.166500629757864,-0.0501396913203886,
0.928776946233916));
#27561=CARTESIAN_POINT('Ctrl Pts',(0.16681765906064,8.64047405809373E-5,
0.93214803633902));
#27562=CARTESIAN_POINT('Ctrl Pts',(0.0530170217188587,-0.198517432567173,
0.8));
#27563=CARTESIAN_POINT('Ctrl Pts',(0.0654219024915668,-0.193924365121538,
0.8));
#27564=CARTESIAN_POINT('Ctrl Pts',(0.0772726753754473,-0.188065368475528,
0.8));
#27565=CARTESIAN_POINT('Ctrl Pts',(0.0884514733522922,-0.181103303150236,
0.8));
#27566=CARTESIAN_POINT('Ctrl Pts',(0.09412650504638,-0.177568939128346,
0.8));
#27567=CARTESIAN_POINT('Ctrl Pts',(0.0996279181736098,-0.173749544851002,
0.8));
#27568=CARTESIAN_POINT('Ctrl Pts',(0.104936837602987,-0.16966283510169,
0.8));
#27569=CARTESIAN_POINT('Ctrl Pts',(0.10962098777257,-0.166057061380704,
0.8));
#27570=CARTESIAN_POINT('Ctrl Pts',(0.114155265023366,-0.162243133727946,
0.8));
#27571=CARTESIAN_POINT('Ctrl Pts',(0.118524756406352,-0.158232269033094,
0.8));
#27572=CARTESIAN_POINT('Ctrl Pts',(0.121396569737292,-0.155596160230106,
0.8));
#27573=CARTESIAN_POINT('Ctrl Pts',(0.124191187364035,-0.152880333162932,
0.8));
#27574=CARTESIAN_POINT('Ctrl Pts',(0.126901910586196,-0.150092210881471,
0.8));
#27575=CARTESIAN_POINT('Ctrl Pts',(0.135875513595552,-0.140862385316535,
0.8));
#27576=CARTESIAN_POINT('Ctrl Pts',(0.143945927205397,-0.130830324459656,
0.8));
#27577=CARTESIAN_POINT('Ctrl Pts',(0.150974563153614,-0.120127060905897,
0.8));
#27578=CARTESIAN_POINT('Ctrl Pts',(0.155531899783608,-0.113187111901085,
0.8));
#27579=CARTESIAN_POINT('Ctrl Pts',(0.159650421905677,-0.105964391211092,
0.8));
#27580=CARTESIAN_POINT('Ctrl Pts',(0.163280590687062,-0.0984918775736134,
0.8));
#27581=CARTESIAN_POINT('Ctrl Pts',(0.165013714615195,-0.0949243321044268,
0.8));
#27582=CARTESIAN_POINT('Ctrl Pts',(0.166631773157808,-0.0913069558365289,
0.8));
#27583=CARTESIAN_POINT('Ctrl Pts',(0.168128066663937,-0.0876495022602451,
0.8));
#27584=CARTESIAN_POINT('Ctrl Pts',(0.172146949722996,-0.0778259762228617,
0.8));
#27585=CARTESIAN_POINT('Ctrl Pts',(0.175295994023174,-0.0677004884915743,
0.8));
#27586=CARTESIAN_POINT('Ctrl Pts',(0.177480263226672,-0.0573468152173212,
0.8));
#27587=CARTESIAN_POINT('Ctrl Pts',(0.179333801272362,-0.048560843554235,
0.8));
#27588=CARTESIAN_POINT('Ctrl Pts',(0.180491858406323,-0.0396100717078052,
0.8));
#27589=CARTESIAN_POINT('Ctrl Pts',(0.18096708784323,-0.0305729202789466,
0.8));
#27590=CARTESIAN_POINT('Ctrl Pts',(0.181136159028966,-0.0273577955642423,
0.8));
#27591=CARTESIAN_POINT('Ctrl Pts',(0.181218443079545,-0.0241331712280784,
0.8));
#27592=CARTESIAN_POINT('Ctrl Pts',(0.181214870924098,-0.0209122942089756,
0.8));
#27593=CARTESIAN_POINT('Ctrl Pts',(0.1812018830209,-0.00920159472786908,
0.8));
#27594=CARTESIAN_POINT('Ctrl Pts',(0.180059445076844,0.00249593154933228,
0.8));
#27595=CARTESIAN_POINT('Ctrl Pts',(0.177833010924532,0.0140076329059244,
0.8));
#27596=CARTESIAN_POINT('Ctrl Pts',(0.176687470499003,0.019930610352574,
0.8));
#27597=CARTESIAN_POINT('Ctrl Pts',(0.17525426981669,0.0258042115192748,
0.8));
#27598=CARTESIAN_POINT('Ctrl Pts',(0.173535645755736,0.0316026384872638,
0.8));
#27599=CARTESIAN_POINT('Ctrl Pts',(0.171850920647243,0.0372866945438873,
0.8));
#27600=CARTESIAN_POINT('Ctrl Pts',(0.169889181319091,0.0429039115259332,
0.8));
#27601=CARTESIAN_POINT('Ctrl Pts',(0.167664346683561,0.0483972355746533,
0.8));
#27602=CARTESIAN_POINT('Ctrl Pts',(0.16420912784319,0.0569284928853236,
0.8));
#27603=CARTESIAN_POINT('Ctrl Pts',(0.160117674787075,0.065174591642692,
0.8));
#27604=CARTESIAN_POINT('Ctrl Pts',(0.155399354804051,0.073039643321633,
0.8));
#27605=CARTESIAN_POINT('Ctrl Pts',(0.15298274940935,0.0770679259275847,
0.8));
#27606=CARTESIAN_POINT('Ctrl Pts',(0.150400765188628,0.0809963604120499,
0.8));
#27607=CARTESIAN_POINT('Ctrl Pts',(0.147663479517856,0.0847983168718068,
0.8));
#27608=CARTESIAN_POINT('Ctrl Pts',(0.142228073022467,0.0923478317277872,
0.8));
#27609=CARTESIAN_POINT('Ctrl Pts',(0.136173701728632,0.0994134091821942,
0.8));
#27610=CARTESIAN_POINT('Ctrl Pts',(0.129505054411736,0.105883695181419,
0.8));
#27611=CARTESIAN_POINT('Ctrl Pts',(0.128726565799248,0.106639027369579,
0.8));
#27612=CARTESIAN_POINT('Ctrl Pts',(0.127939691591626,0.107386221438147,
0.8));
#27613=CARTESIAN_POINT('Ctrl Pts',(0.127144588893496,0.108125211870903,
0.8));
#27614=CARTESIAN_POINT('Origin',(0.,0.,1.3));
#27615=CARTESIAN_POINT('Origin',(0.,0.,1.8));
#27616=CARTESIAN_POINT('Origin',(0.4,0.6,0.8));
#27617=CARTESIAN_POINT('',(0.4,0.6,0.8));
#27618=CARTESIAN_POINT('',(-0.4,0.6,0.8));
#27619=CARTESIAN_POINT('',(0.4,0.6,0.8));
#27620=CARTESIAN_POINT('',(-0.4,0.6,3.6));
#27621=CARTESIAN_POINT('',(-0.4,0.6,0.8));
#27622=CARTESIAN_POINT('',(0.4,0.6,3.6));
#27623=CARTESIAN_POINT('',(0.4,0.6,3.6));
#27624=CARTESIAN_POINT('',(0.4,0.6,0.8));
#27625=CARTESIAN_POINT('Origin',(0.4,-0.6,0.8));
#27626=CARTESIAN_POINT('',(0.4,-0.6,0.8));
#27627=CARTESIAN_POINT('',(0.4,-0.6,0.8));
#27628=CARTESIAN_POINT('',(0.4,-0.6,3.6));
#27629=CARTESIAN_POINT('',(0.4,-0.6,3.6));
#27630=CARTESIAN_POINT('',(0.4,-0.6,0.8));
#27631=CARTESIAN_POINT('Origin',(-0.4,-0.6,0.8));
#27632=CARTESIAN_POINT('',(-0.4,-0.6,0.8));
#27633=CARTESIAN_POINT('',(-0.4,-0.6,0.8));
#27634=CARTESIAN_POINT('',(-0.4,-0.6,3.6));
#27635=CARTESIAN_POINT('',(-0.4,-0.6,3.6));
#27636=CARTESIAN_POINT('',(-0.4,-0.6,0.8));
#27637=CARTESIAN_POINT('Origin',(-0.4,0.6,0.8));
#27638=CARTESIAN_POINT('',(-0.4,0.6,0.8));
#27639=CARTESIAN_POINT('',(-0.4,0.6,3.6));
#27640=CARTESIAN_POINT('Origin',(0.,0.,3.6));
#27641=CARTESIAN_POINT('Origin',(0.,0.,0.8));
#27642=CARTESIAN_POINT('',(0.,0.,0.));
#27643=CARTESIAN_POINT('Origin',(0.,0.,3.7));
#27644=CARTESIAN_POINT('',(-0.126245375007135,3.12536796039931E-5,3.51934196736194));
#27645=CARTESIAN_POINT('',(-0.126365398388193,-0.00016976464794081,3.50565803263806));
#27646=CARTESIAN_POINT('',(-0.12645,1.54856587752183E-17,3.7));
#27647=CARTESIAN_POINT('',(-0.0958116152722475,0.0825211298936389,3.5));
#27648=CARTESIAN_POINT('Ctrl Pts',(-0.126365398388193,-0.00016976464794081,
3.50565803263806));
#27649=CARTESIAN_POINT('Ctrl Pts',(-0.126096583499468,0.0297434857833807,
3.5037720217587));
#27650=CARTESIAN_POINT('Ctrl Pts',(-0.115369380269343,0.0598134784363466,
3.50188601087935));
#27651=CARTESIAN_POINT('Ctrl Pts',(-0.0958116152722475,0.0825211298936389,
3.5));
#27652=CARTESIAN_POINT('',(-0.12645,1.54856587752183E-17,3.5));
#27653=CARTESIAN_POINT('Origin',(0.,0.,3.5));
#27654=CARTESIAN_POINT('',(-0.12645,-1.54856587752183E-17,3.4));
#27655=CARTESIAN_POINT('',(-0.12645,1.54856587752183E-17,3.7));
#27656=CARTESIAN_POINT('Origin',(0.,0.,3.4));
#27657=CARTESIAN_POINT('',(0.095993992990581,0.0826600147079878,3.5));
#27658=CARTESIAN_POINT('Origin',(0.,0.,3.5));
#27659=CARTESIAN_POINT('Ctrl Pts',(0.0959941578858439,0.0826601402795114,
3.5));
#27660=CARTESIAN_POINT('Ctrl Pts',(0.0693049284490514,0.113544181600847,
3.5025799450779));
#27661=CARTESIAN_POINT('Ctrl Pts',(0.0262885066473286,0.130447374694629,
3.5051598901558));
#27662=CARTESIAN_POINT('Ctrl Pts',(-0.0142676563835003,0.125842979166089,
3.5077398352337));
#27663=CARTESIAN_POINT('Ctrl Pts',(-0.0558709915822301,0.121119696778261,
3.51038639525932));
#27664=CARTESIAN_POINT('Ctrl Pts',(-0.0948853785622285,0.0937638222778825,
3.51303295528495));
#27665=CARTESIAN_POINT('Ctrl Pts',(-0.113475688700545,0.0562620506672719,
3.51567951531057));
#27666=CARTESIAN_POINT('Ctrl Pts',(-0.122051112249405,0.0389630614088429,
3.51690033266103));
#27667=CARTESIAN_POINT('Ctrl Pts',(-0.126280629837482,0.0195051929476654,
3.51812115001148));
#27668=CARTESIAN_POINT('Ctrl Pts',(-0.126245375007135,3.12536796039931E-5,
3.51934196736194));
#27669=CARTESIAN_POINT('Origin',(0.,0.,3.7));
#27670=CARTESIAN_POINT('',(-0.126440375727766,-0.00011573372396179,3.56934196736194));
#27671=CARTESIAN_POINT('',(-0.126657922659285,8.80032312977707E-6,3.55565803263806));
#27672=CARTESIAN_POINT('',(-0.12645,1.54856587752183E-17,3.7));
#27673=CARTESIAN_POINT('Ctrl Pts',(-0.126657922659285,8.80032312977707E-6,
3.55565803263806));
#27674=CARTESIAN_POINT('Ctrl Pts',(-0.126658305335383,0.00043204034557634,
3.55563127527141));
#27675=CARTESIAN_POINT('Ctrl Pts',(-0.126656367352663,0.000855276509828617,
3.55560451790477));
#27676=CARTESIAN_POINT('Ctrl Pts',(-0.126652098121077,0.00127848889899514,
3.55557776053813));
#27677=CARTESIAN_POINT('Ctrl Pts',(-0.126229830197349,0.0431382506048763,
3.5529312005125));
#27678=CARTESIAN_POINT('Ctrl Pts',(-0.103000707566798,0.0847654181274417,
3.55028464048688));
#27679=CARTESIAN_POINT('Ctrl Pts',(-0.0675987137490504,0.107109477361251,
3.54763808046125));
#27680=CARTESIAN_POINT('Ctrl Pts',(-0.0321967199313031,0.12945353659506,
3.54499152043563));
#27681=CARTESIAN_POINT('Ctrl Pts',(0.0153781450736419,0.132514487540114,
3.54234496041));
#27682=CARTESIAN_POINT('Ctrl Pts',(0.0533465621421041,0.114879483210429,
3.53969840038438));
#27683=CARTESIAN_POINT('Ctrl Pts',(0.0913149792105665,0.097244478880744,
3.53705184035875));
#27684=CARTESIAN_POINT('Ctrl Pts',(0.119676948342547,0.0589135192763201,
3.53440528033313));
#27685=CARTESIAN_POINT('Ctrl Pts',(0.125448844532432,0.0174567066922002,
3.5317587203075));
#27686=CARTESIAN_POINT('Ctrl Pts',(0.131220740722318,-0.0240001058919198,
3.52911216028188));
#27687=CARTESIAN_POINT('Ctrl Pts',(0.11440256397011,-0.0685827714557354,
3.52646560025625));
#27688=CARTESIAN_POINT('Ctrl Pts',(0.0826932442631274,-0.0959262477461666,
3.52381904023063));
#27689=CARTESIAN_POINT('Ctrl Pts',(0.0509839245561443,-0.123269724036598,
3.521172480205));
#27690=CARTESIAN_POINT('Ctrl Pts',(0.00438346189438567,-0.133374011053645,
3.51852592017938));
#27691=CARTESIAN_POINT('Ctrl Pts',(-0.0357753168513136,-0.121524408044806,
3.51587936015375));
#27692=CARTESIAN_POINT('Ctrl Pts',(-0.0759340955970119,-0.109674805035968,
3.51323280012813));
#27693=CARTESIAN_POINT('Ctrl Pts',(-0.109651190426652,-0.0758713120012468,
3.5105862401025));
#27694=CARTESIAN_POINT('Ctrl Pts',(-0.121481718337573,-0.0357885021759826,
3.50793968007688));
#27695=CARTESIAN_POINT('Ctrl Pts',(-0.124881489291372,-0.0242697961962776,
3.5071791309306));
#27696=CARTESIAN_POINT('Ctrl Pts',(-0.126473800166976,-0.012232524903913,
3.50641858178433));
#27697=CARTESIAN_POINT('Ctrl Pts',(-0.126365398388193,-0.00016976464794081,
3.50565803263806));
#27698=CARTESIAN_POINT('Ctrl Pts',(-0.126245375007135,3.12536796039931E-5,
3.51934196736194));
#27699=CARTESIAN_POINT('Ctrl Pts',(-0.12620420233203,-0.0227115638743483,
3.52076771003711));
#27700=CARTESIAN_POINT('Ctrl Pts',(-0.120346328214258,-0.0454763003201931,
3.52219345271228));
#27701=CARTESIAN_POINT('Ctrl Pts',(-0.108800985171859,-0.06484981090145,
3.52361919538745));
#27702=CARTESIAN_POINT('Ctrl Pts',(-0.0873697382082225,-0.100812232138721,
3.52626575541307));
#27703=CARTESIAN_POINT('Ctrl Pts',(-0.0463410109843132,-0.125089405892421,
3.5289123154387));
#27704=CARTESIAN_POINT('Ctrl Pts',(-0.0045038827259274,-0.126577024986295,
3.53155887546432));
#27705=CARTESIAN_POINT('Ctrl Pts',(0.0373332455324584,-0.128064644080169,
3.53420543548995));
#27706=CARTESIAN_POINT('Ctrl Pts',(0.0799787748253208,-0.106762708514216,
3.53685199551558));
#27707=CARTESIAN_POINT('Ctrl Pts',(0.103913443798274,-0.0724181339568129,
3.5394985555412));
#27708=CARTESIAN_POINT('Ctrl Pts',(0.127848112771228,-0.0380735593994097,
3.54214511556683));
#27709=CARTESIAN_POINT('Ctrl Pts',(0.133071921424273,0.00931365414944368,
3.54479167559245));
#27710=CARTESIAN_POINT('Ctrl Pts',(0.117191739814205,0.0480476856196858,
3.54743823561807));
#27711=CARTESIAN_POINT('Ctrl Pts',(0.101311558204136,0.086781717089928,
3.5500847956437));
#27712=CARTESIAN_POINT('Ctrl Pts',(0.0643273863309551,0.116862566481559,
3.55273135566933));
#27713=CARTESIAN_POINT('Ctrl Pts',(0.0231710436075753,0.124520839933968,
3.55537791569495));
#27714=CARTESIAN_POINT('Ctrl Pts',(-0.0179852991158045,0.132179113386376,
3.55802447572058));
#27715=CARTESIAN_POINT('Ctrl Pts',(-0.0633138126893829,0.117414810899563,
3.5606710357462));
#27716=CARTESIAN_POINT('Ctrl Pts',(-0.0920640726196609,0.0869862082349088,
3.56331759577183));
#27717=CARTESIAN_POINT('Ctrl Pts',(-0.113878836874053,0.0638979719779231,
3.5653257196352));
#27718=CARTESIAN_POINT('Ctrl Pts',(-0.126149033113671,0.0317913564834069,
3.56733384349857));
#27719=CARTESIAN_POINT('Ctrl Pts',(-0.126440375727766,-0.00011573372396179,
3.56934196736194));
#27720=CARTESIAN_POINT('Origin',(0.,0.,3.7));
#27721=CARTESIAN_POINT('',(-0.126640903602401,4.27927297787234E-5,3.61934196736194));
#27722=CARTESIAN_POINT('',(-0.126360536148104,0.000106176725758032,3.60565803263806));
#27723=CARTESIAN_POINT('',(-0.12645,1.54856587752183E-17,3.7));
#27724=CARTESIAN_POINT('Ctrl Pts',(-0.126360536148104,0.000106176725758032,
3.60565803263806));
#27725=CARTESIAN_POINT('Ctrl Pts',(-0.126463554653562,0.0130615819764901,
3.6048439687585));
#27726=CARTESIAN_POINT('Ctrl Pts',(-0.124630630169346,0.0259885352839278,
3.60402990487894));
#27727=CARTESIAN_POINT('Ctrl Pts',(-0.120740583509641,0.0382635675762761,
3.60321584099939));
#27728=CARTESIAN_POINT('Ctrl Pts',(-0.108093858546251,0.0781702758752103,
3.60056928097376));
#27729=CARTESIAN_POINT('Ctrl Pts',(-0.0737047770896513,0.111186630609157,
3.59792272094814));
#27730=CARTESIAN_POINT('Ctrl Pts',(-0.0333162689132352,0.122198227017938,
3.59527616092251));
#27731=CARTESIAN_POINT('Ctrl Pts',(0.00707223926318085,0.133209823426719,
3.59262960089688));
#27732=CARTESIAN_POINT('Ctrl Pts',(0.0534601741594139,0.122216661510335,
3.58998304087126));
#27733=CARTESIAN_POINT('Ctrl Pts',(0.0846116648984234,0.0942510766887394,
3.58733648084563));
#27734=CARTESIAN_POINT('Ctrl Pts',(0.115763155637433,0.0662854918671437,
3.58468992082001));
#27735=CARTESIAN_POINT('Ctrl Pts',(0.131678202219219,0.0213474841403372,
3.58204336079438));
#27736=CARTESIAN_POINT('Ctrl Pts',(0.125071080316048,-0.0199904290876357,
3.57939680076876));
#27737=CARTESIAN_POINT('Ctrl Pts',(0.118463958412876,-0.0613283423156084,
3.57675024074313));
#27738=CARTESIAN_POINT('Ctrl Pts',(0.0893346680247476,-0.0990661610447472,
3.57410368071751));
#27739=CARTESIAN_POINT('Ctrl Pts',(0.0510182611448099,-0.115928737877881,
3.57145712069188));
#27740=CARTESIAN_POINT('Ctrl Pts',(0.0127018542648722,-0.132791314711016,
3.56881056066626));
#27741=CARTESIAN_POINT('Ctrl Pts',(-0.0348016691068745,-0.128778649648146,
3.56616400064063));
#27742=CARTESIAN_POINT('Ctrl Pts',(-0.069745724184294,-0.105726139172113,
3.56351744061501));
#27743=CARTESIAN_POINT('Ctrl Pts',(-0.104336486351438,-0.0829066951932904,
3.56089763795602));
#27744=CARTESIAN_POINT('Ctrl Pts',(-0.126620455001409,-0.0414304545565597,
3.55827783529704));
#27745=CARTESIAN_POINT('Ctrl Pts',(-0.126657922659285,8.80032312977707E-6,
3.55565803263806));
#27746=CARTESIAN_POINT('Ctrl Pts',(-0.126440375727766,-0.00011573372396179,
3.56934196736194));
#27747=CARTESIAN_POINT('Ctrl Pts',(-0.126533001319164,-0.0102598491305144,
3.5699804035242));
#27748=CARTESIAN_POINT('Ctrl Pts',(-0.125414835808849,-0.020383797044434,
3.57061883968645));
#27749=CARTESIAN_POINT('Ctrl Pts',(-0.123007652953296,-0.0301913583035261,
3.5712572758487));
#27750=CARTESIAN_POINT('Ctrl Pts',(-0.113028967069674,-0.0708474193348126,
3.57390383587433));
#27751=CARTESIAN_POINT('Ctrl Pts',(-0.0808995890154535,-0.10606663855489,
3.57655039589995));
#27752=CARTESIAN_POINT('Ctrl Pts',(-0.0413281018804841,-0.119726229337694,
3.57919695592558));
#27753=CARTESIAN_POINT('Ctrl Pts',(-0.00175661474551533,-0.133385820120498,
3.5818435159512));
#27754=CARTESIAN_POINT('Ctrl Pts',(0.0452569814702019,-0.125485782466029,
3.58449007597683));
#27755=CARTESIAN_POINT('Ctrl Pts',(0.0781904578005954,-0.0996425759257176,
3.58713663600245));
#27756=CARTESIAN_POINT('Ctrl Pts',(0.111123934130988,-0.0737993693854069,
3.58978319602808));
#27757=CARTESIAN_POINT('Ctrl Pts',(0.129977290576058,-0.0300129939592548,
3.5924297560537));
#27758=CARTESIAN_POINT('Ctrl Pts',(0.126119643637387,0.0116716003968688,
3.59507631607933));
#27759=CARTESIAN_POINT('Ctrl Pts',(0.122261996698715,0.0533561947529935,
3.59772287610496));
#27760=CARTESIAN_POINT('Ctrl Pts',(0.0956933463762995,0.0929390080390894,
3.60036943613058));
#27761=CARTESIAN_POINT('Ctrl Pts',(0.0585765347711879,0.112299501333378,
3.60301599615621));
#27762=CARTESIAN_POINT('Ctrl Pts',(0.0214597231660768,0.131659994627667,
3.60566255618183));
#27763=CARTESIAN_POINT('Ctrl Pts',(-0.0262052497217305,0.130798167930148,
3.60830911620746));
#27764=CARTESIAN_POINT('Ctrl Pts',(-0.0625979093128853,0.11010854389779,
3.61095567623308));
#27765=CARTESIAN_POINT('Ctrl Pts',(-0.0989905689040401,0.089418919865431,
3.61360223625871));
#27766=CARTESIAN_POINT('Ctrl Pts',(-0.124110915198542,0.048901498498232,
3.61624879628433));
#27767=CARTESIAN_POINT('Ctrl Pts',(-0.12645913501461,0.00710470077718534,
3.61889535630996));
#27768=CARTESIAN_POINT('Ctrl Pts',(-0.126591223576389,0.00475360959731907,
3.61904422666062));
#27769=CARTESIAN_POINT('Ctrl Pts',(-0.126651258400685,0.00239847031733228,
3.61919309701128));
#27770=CARTESIAN_POINT('Ctrl Pts',(-0.126640903602401,4.27927297787234E-5,
3.61934196736194));
#27771=CARTESIAN_POINT('Origin',(0.,0.,3.7));
#27772=CARTESIAN_POINT('',(-0.126313625852874,8.92012377725487E-5,3.66934196736194));
#27773=CARTESIAN_POINT('',(-0.126280524269743,-6.82698929511343E-5,3.65565803263806));
#27774=CARTESIAN_POINT('',(-0.12645,1.54856587752183E-17,3.7));
#27775=CARTESIAN_POINT('Ctrl Pts',(-0.126280524269743,-6.82698929511343E-5,
3.65565803263806));
#27776=CARTESIAN_POINT('Ctrl Pts',(-0.126155459137289,0.0254573418705088,
3.65405666224558));
#27777=CARTESIAN_POINT('Ctrl Pts',(-0.1186500792639,0.0510505822956786,
3.65245529185311));
#27778=CARTESIAN_POINT('Ctrl Pts',(-0.104270310346229,0.0719033403784211,
3.65085392146064));
#27779=CARTESIAN_POINT('Ctrl Pts',(-0.0805050891493468,0.106366370433962,
3.64820736143502));
#27780=CARTESIAN_POINT('Ctrl Pts',(-0.0379633950684185,0.127881407935326,
3.64556080140939));
#27781=CARTESIAN_POINT('Ctrl Pts',(0.00387966794034225,0.126599115215449,
3.64291424138376));
#27782=CARTESIAN_POINT('Ctrl Pts',(0.0457227309491033,0.125316822495572,
3.64026768135814));
#27783=CARTESIAN_POINT('Ctrl Pts',(0.0868671628856968,0.101237199554454,
3.63762112133251));
#27784=CARTESIAN_POINT('Ctrl Pts',(0.108477510477425,0.0653836202783246,
3.63497456130689));
#27785=CARTESIAN_POINT('Ctrl Pts',(0.130087858069152,0.0295300410021955,
3.63232800128126));
#27786=CARTESIAN_POINT('Ctrl Pts',(0.132164121316015,-0.018097494608945,
3.62968144125564));
#27787=CARTESIAN_POINT('Ctrl Pts',(0.113755810560665,-0.0556956347668708,
3.62703488123001));
#27788=CARTESIAN_POINT('Ctrl Pts',(0.0953474998053144,-0.0932937749247968,
3.62438832120439));
#27789=CARTESIAN_POINT('Ctrl Pts',(0.0564546150477511,-0.120862519629508,
3.62174176117876));
#27790=CARTESIAN_POINT('Ctrl Pts',(0.0148818767183724,-0.125781225334577,
3.61909520115314));
#27791=CARTESIAN_POINT('Ctrl Pts',(-0.0266908616110063,-0.130699931039647,
3.61644864112751));
#27792=CARTESIAN_POINT('Ctrl Pts',(-0.0709434535122003,-0.112968597745074,
3.61380208110189));
#27793=CARTESIAN_POINT('Ctrl Pts',(-0.0976175652277067,-0.0807044001658271,
3.61115552107626));
#27794=CARTESIAN_POINT('Ctrl Pts',(-0.116086901439685,-0.0583644505151555,
3.60932302493019));
#27795=CARTESIAN_POINT('Ctrl Pts',(-0.126128636638782,-0.0290570508647223,
3.60749052878412));
#27796=CARTESIAN_POINT('Ctrl Pts',(-0.126360536148104,0.000106176725758032,
3.60565803263806));
#27797=CARTESIAN_POINT('Ctrl Pts',(-0.126640903602401,4.27927297787234E-5,
3.61934196736194));
#27798=CARTESIAN_POINT('Ctrl Pts',(-0.126467174766239,-0.0394798628014113,
3.62183965703691));
#27799=CARTESIAN_POINT('Ctrl Pts',(-0.106479582237496,-0.0791540456794125,
3.62433734671187));
#27800=CARTESIAN_POINT('Ctrl Pts',(-0.0745372494842149,-0.102404041708738,
3.62683503638683));
#27801=CARTESIAN_POINT('Ctrl Pts',(-0.0406910508001211,-0.12703981239872,
3.62948159641246));
#27802=CARTESIAN_POINT('Ctrl Pts',(0.00657743990569856,-0.133235179703789,
3.63212815643808));
#27803=CARTESIAN_POINT('Ctrl Pts',(0.0456292459986054,-0.118153973308938,
3.63477471646371));
#27804=CARTESIAN_POINT('Ctrl Pts',(0.0846810520915122,-0.103072766914087,
3.63742127648934));
#27805=CARTESIAN_POINT('Ctrl Pts',(0.115516173571506,-0.0667149868193161,
3.64006783651496));
#27806=CARTESIAN_POINT('Ctrl Pts',(0.124018641769873,-0.0257248122789798,
3.64271439654059));
#27807=CARTESIAN_POINT('Ctrl Pts',(0.132521109968241,0.0152653622613568,
3.64536095656621));
#27808=CARTESIAN_POINT('Ctrl Pts',(0.11869092488498,0.0608879312472584,
3.64800751659183));
#27809=CARTESIAN_POINT('Ctrl Pts',(0.0888593883296617,0.0902574016134864,
3.65065407661746));
#27810=CARTESIAN_POINT('Ctrl Pts',(0.0590278517743432,0.119626871979714,
3.65330063664309));
#27811=CARTESIAN_POINT('Ctrl Pts',(0.0131949637469664,0.132743243726269,
3.65594719666871));
#27812=CARTESIAN_POINT('Ctrl Pts',(-0.027657500752443,0.123601990750641,
3.65859375669434));
#27813=CARTESIAN_POINT('Ctrl Pts',(-0.0685099652518527,0.114460737775013,
3.66124031671997));
#27814=CARTESIAN_POINT('Ctrl Pts',(-0.104382006223295,0.0830618600772021,
3.66388687674559));
#27815=CARTESIAN_POINT('Ctrl Pts',(-0.118851810998494,0.043779407059542,
3.66653343677121));
#27816=CARTESIAN_POINT('Ctrl Pts',(-0.123970265263591,0.0298838886116103,
3.66746961363479));
#27817=CARTESIAN_POINT('Ctrl Pts',(-0.126410714036168,0.0150019191305398,
3.66840579049837));
#27818=CARTESIAN_POINT('Ctrl Pts',(-0.126313625852874,8.92012377725487E-5,
3.66934196736194));
#27819=CARTESIAN_POINT('Origin',(0.,0.,3.7));
#27820=CARTESIAN_POINT('',(-0.126318202311182,-9.13759226411071E-5,3.71934196736194));
#27821=CARTESIAN_POINT('',(-0.126609590382811,-7.02044759900073E-5,3.70565803263806));
#27822=CARTESIAN_POINT('',(-0.12645,1.54856587752183E-17,3.7));
#27823=CARTESIAN_POINT('Ctrl Pts',(-0.126609590382811,-7.02044759900073E-5,
3.70565803263806));
#27824=CARTESIAN_POINT('Ctrl Pts',(-0.126357411318116,0.0377522139233435,
3.70326935573267));
#27825=CARTESIAN_POINT('Ctrl Pts',(-0.108290467899376,0.0757836426892297,
3.70088067882728));
#27826=CARTESIAN_POINT('Ctrl Pts',(-0.0786816086433086,0.099255188273642,
3.6984920019219));
#27827=CARTESIAN_POINT('Ctrl Pts',(-0.0458761575859702,0.125260737263231,
3.69584544189627));
#27828=CARTESIAN_POINT('Ctrl Pts',(0.00109788169852634,0.133392911300054,
3.69319888187064));
#27829=CARTESIAN_POINT('Ctrl Pts',(0.0407363279886946,0.119928893584969,
3.69055232184502));
#27830=CARTESIAN_POINT('Ctrl Pts',(0.0803747742788628,0.106464875869883,
3.68790576181939));
#27831=CARTESIAN_POINT('Ctrl Pts',(0.112677627574703,0.071404666402888,
3.68525920179377));
#27832=CARTESIAN_POINT('Ctrl Pts',(0.122857008829439,0.0307984304737455,
3.68261264176814));
#27833=CARTESIAN_POINT('Ctrl Pts',(0.133036390084175,-0.00980780545539708,
3.67996608174252));
#27834=CARTESIAN_POINT('Ctrl Pts',(0.121092299297808,-0.0559600678466875,
3.67731952171689));
#27835=CARTESIAN_POINT('Ctrl Pts',(0.0924926054626293,-0.08653037546552,
3.67467296169127));
#27836=CARTESIAN_POINT('Ctrl Pts',(0.0638929116274508,-0.117100683084353,
3.67202640166564));
#27837=CARTESIAN_POINT('Ctrl Pts',(0.0186376147434612,-0.132089035930727,
3.66937984164002));
#27838=CARTESIAN_POINT('Ctrl Pts',(-0.0225559247032424,-0.124633936707157,
3.66673328161439));
#27839=CARTESIAN_POINT('Ctrl Pts',(-0.063749464149946,-0.117178837483586,
3.66408672158877));
#27840=CARTESIAN_POINT('Ctrl Pts',(-0.100881246159364,-0.0872802861900701,
3.66144016156314));
#27841=CARTESIAN_POINT('Ctrl Pts',(-0.116952763007655,-0.0486254992384533,
3.65879360153752));
#27842=CARTESIAN_POINT('Ctrl Pts',(-0.123299788065177,-0.0333598025596003,
3.65774841190436));
#27843=CARTESIAN_POINT('Ctrl Pts',(-0.126362152343126,-0.016728441031668,
3.65670322227121));
#27844=CARTESIAN_POINT('Ctrl Pts',(-0.126280524269743,-6.82698929511343E-5,
3.65565803263806));
#27845=CARTESIAN_POINT('Ctrl Pts',(-0.126313625852874,8.92012377725487E-5,
3.66934196736194));
#27846=CARTESIAN_POINT('Ctrl Pts',(-0.126136246983132,-0.027156143714207,
3.67105235052399));
#27847=CARTESIAN_POINT('Ctrl Pts',(-0.117488868450918,-0.0545041232450019,
3.67276273368604));
#27848=CARTESIAN_POINT('Ctrl Pts',(-0.101228105076468,-0.0761266063810683,
3.67447311684809));
#27849=CARTESIAN_POINT('Ctrl Pts',(-0.0760670258002872,-0.10958413846651,
3.67711967687372));
#27850=CARTESIAN_POINT('Ctrl Pts',(-0.0326772986689716,-0.129333174299883,
3.67976623689934));
#27851=CARTESIAN_POINT('Ctrl Pts',(0.00907775247578101,-0.126332829739009,
3.68241279692497));
#27852=CARTESIAN_POINT('Ctrl Pts',(0.050832803620533,-0.123332485178135,
3.68505935695059));
#27853=CARTESIAN_POINT('Ctrl Pts',(0.0909531787787221,-0.0975827602230137,
3.68770591697622));
#27854=CARTESIAN_POINT('Ctrl Pts',(0.11107222624856,-0.0608715862708329,
3.69035247700184));
#27855=CARTESIAN_POINT('Ctrl Pts',(0.131191273718398,-0.0241604123186516,
3.69299903702747));
#27856=CARTESIAN_POINT('Ctrl Pts',(0.131308993499885,0.0235122106305895,
3.69564559705309));
#27857=CARTESIAN_POINT('Ctrl Pts',(0.111371494820412,0.0603222977018694,
3.69829215707872));
#27858=CARTESIAN_POINT('Ctrl Pts',(0.0914339961409399,0.097132384773149,
3.70093871710434));
#27859=CARTESIAN_POINT('Ctrl Pts',(0.0514412790005074,0.123079935966467,
3.70358527712997));
#27860=CARTESIAN_POINT('Ctrl Pts',(0.00970155469863815,0.126286457292336,
3.70623183715559));
#27861=CARTESIAN_POINT('Ctrl Pts',(-0.0320381696032317,0.129492978618205,
3.70887839718122));
#27862=CARTESIAN_POINT('Ctrl Pts',(-0.0755249010665388,0.109958470076624,
3.71152495720684));
#27863=CARTESIAN_POINT('Ctrl Pts',(-0.100850908347825,0.0766256076274997,
3.71417151723247));
#27864=CARTESIAN_POINT('Ctrl Pts',(-0.117343620441844,0.0549186998809637,
3.71589500060896));
#27865=CARTESIAN_POINT('Ctrl Pts',(-0.126134681028771,0.0273601470071565,
3.71761848398545));
#27866=CARTESIAN_POINT('Ctrl Pts',(-0.126318202311182,-9.13759226411071E-5,
3.71934196736194));
#27867=CARTESIAN_POINT('Origin',(0.,0.,3.7));
#27868=CARTESIAN_POINT('',(-0.126643738265873,-3.92119282522094E-5,3.76934196736194));
#27869=CARTESIAN_POINT('',(-0.126492921331233,0.000111898061355794,3.75565803263806));
#27870=CARTESIAN_POINT('',(-0.12645,1.54856587752183E-17,3.7));
#27871=CARTESIAN_POINT('Ctrl Pts',(-0.126492921331233,0.000111898061355794,
3.75565803263806));
#27872=CARTESIAN_POINT('Ctrl Pts',(-0.12657025228906,0.00851493641555574,
3.75512860924538));
#27873=CARTESIAN_POINT('Ctrl Pts',(-0.125804504023154,0.0169039539351017,
3.7545991858527));
#27874=CARTESIAN_POINT('Ctrl Pts',(-0.12414416907011,0.0251120135156184,
3.75406976246003));
#27875=CARTESIAN_POINT('Ctrl Pts',(-0.115844240928182,0.06614367678216,
3.7514232024344));
#27876=CARTESIAN_POINT('Ctrl Pts',(-0.0851890554053168,0.102653294996741,
3.74877664240878));
#27877=CARTESIAN_POINT('Ctrl Pts',(-0.0462122079706087,0.117927179951992,
3.74613008238315));
#27878=CARTESIAN_POINT('Ctrl Pts',(-0.00723536053590029,0.133201064907244,
3.74348352235752));
#27879=CARTESIAN_POINT('Ctrl Pts',(0.0400631488106516,0.127239216603166,
3.7408369623319));
#27880=CARTESIAN_POINT('Ctrl Pts',(0.0740306001411793,0.102770901424588,
3.73819040230627));
#27881=CARTESIAN_POINT('Ctrl Pts',(0.107998051471707,0.0783025862460102,
3.73554384228065));
#27882=CARTESIAN_POINT('Ctrl Pts',(0.12863444478621,0.0353278041929325,
3.73289728225502));
#27883=CARTESIAN_POINT('Ctrl Pts',(0.126492673803057,-0.00648007801438488,
3.7302507222294));
#27884=CARTESIAN_POINT('Ctrl Pts',(0.124350902819903,-0.0482879602217022,
3.72760416220377));
#27885=CARTESIAN_POINT('Ctrl Pts',(0.0994309675390923,-0.0889289425832592,
3.72495760217815));
#27886=CARTESIAN_POINT('Ctrl Pts',(0.063140931062625,-0.109798045345167,
3.72231104215252));
#27887=CARTESIAN_POINT('Ctrl Pts',(0.0268508945861577,-0.130667148107075,
3.7196644821269));
#27888=CARTESIAN_POINT('Ctrl Pts',(-0.020809243085966,-0.131764371269333,
3.71701792210127));
#27889=CARTESIAN_POINT('Ctrl Pts',(-0.0580212126891809,-0.112587418545307,
3.71437136207565));
#27890=CARTESIAN_POINT('Ctrl Pts',(-0.0952331822923957,-0.0934104658212808,
3.71172480205002));
#27891=CARTESIAN_POINT('Ctrl Pts',(-0.121996983826702,-0.0539593372109697,
3.7090782420244));
#27892=CARTESIAN_POINT('Ctrl Pts',(-0.126060453178764,-0.0122943109346363,
3.70643168199877));
#27893=CARTESIAN_POINT('Ctrl Pts',(-0.126456401181211,-0.00823443438662399,
3.70617379887853));
#27894=CARTESIAN_POINT('Ctrl Pts',(-0.126636815799491,-0.0041535374917583,
3.70591591575829));
#27895=CARTESIAN_POINT('Ctrl Pts',(-0.126609590382811,-7.02044759900073E-5,
3.70565803263806));
#27896=CARTESIAN_POINT('Ctrl Pts',(-0.126318202311182,-9.13759226411071E-5,
3.71934196736194));
#27897=CARTESIAN_POINT('Ctrl Pts',(-0.126416494068865,-0.0147940763636936,
3.72026504401107));
#27898=CARTESIAN_POINT('Ctrl Pts',(-0.12404567634908,-0.0294660748073717,
3.72118812066021));
#27899=CARTESIAN_POINT('Ctrl Pts',(-0.119066572492589,-0.0431919063448052,
3.72211119730934));
#27900=CARTESIAN_POINT('Ctrl Pts',(-0.104790946256804,-0.0825453415113195,
3.72475775733497));
#27901=CARTESIAN_POINT('Ctrl Pts',(-0.0690744106859675,-0.11412099548768,
3.7274043173606));
#27902=CARTESIAN_POINT('Ctrl Pts',(-0.0282675897675097,-0.123463892809314,
3.73005087738622));
#27903=CARTESIAN_POINT('Ctrl Pts',(0.0125392311509478,-0.132806790130948,
3.73269743741185));
#27904=CARTESIAN_POINT('Ctrl Pts',(0.0584363374170267,-0.119916930797855,
3.73534399743747));
#27905=CARTESIAN_POINT('Ctrl Pts',(0.0884125555029259,-0.0906951458916328,
3.7379905574631));
#27906=CARTESIAN_POINT('Ctrl Pts',(0.118388773588825,-0.0614733609854108,
3.74063711748872));
#27907=CARTESIAN_POINT('Ctrl Pts',(0.132444103494545,-0.0159196505060593,
3.74328367751435));
#27908=CARTESIAN_POINT('Ctrl Pts',(0.124144174958903,0.0251120147068241,
3.74593023753997));
#27909=CARTESIAN_POINT('Ctrl Pts',(0.115844246423262,0.0661436799197074,
3.7485767975656));
#27910=CARTESIAN_POINT('Ctrl Pts',(0.0851890594462595,0.102653299866123,
3.75122335759122));
#27911=CARTESIAN_POINT('Ctrl Pts',(0.0462122101626772,0.117927185545889,
3.75386991761685));
#27912=CARTESIAN_POINT('Ctrl Pts',(0.00723536087909469,0.133201071225655,
3.75651647764247));
#27913=CARTESIAN_POINT('Ctrl Pts',(-0.0400631507110678,0.127239222638772,
3.7591630376681));
#27914=CARTESIAN_POINT('Ctrl Pts',(-0.0740306036528435,0.102770906299531,
3.76180959769372));
#27915=CARTESIAN_POINT('Ctrl Pts',(-0.106255505634774,0.0795578294448588,
3.76432038758313));
#27916=CARTESIAN_POINT('Ctrl Pts',(-0.12648204772981,0.0396883664632768,
3.76683117747254));
#27917=CARTESIAN_POINT('Ctrl Pts',(-0.126643738265873,-3.92119282522094E-5,
3.76934196736194));
#27918=CARTESIAN_POINT('Origin',(0.,0.,3.7));
#27919=CARTESIAN_POINT('',(-0.12643411897368,0.000115681837355761,3.81934196736194));
#27920=CARTESIAN_POINT('',(-0.126243465328102,1.71616150689059E-6,3.80565803263806));
#27921=CARTESIAN_POINT('',(-0.12645,1.54856587752183E-17,3.7));
#27922=CARTESIAN_POINT('Ctrl Pts',(-0.126243465328102,1.71616150689059E-6,
3.80565803263806));
#27923=CARTESIAN_POINT('Ctrl Pts',(-0.126246007062352,0.0210055997219054,
3.80434130273247));
#27924=CARTESIAN_POINT('Ctrl Pts',(-0.121290894068088,0.0420083553470164,
3.80302457282688));
#27925=CARTESIAN_POINT('Ctrl Pts',(-0.111371489537494,0.0603222948404575,
3.80170784292128));
#27926=CARTESIAN_POINT('Ctrl Pts',(-0.0914339918037617,0.0971323801656441,
3.79906128289566));
#27927=CARTESIAN_POINT('Ctrl Pts',(-0.0514412765603963,0.123079930128149,
3.79641472287003));
#27928=CARTESIAN_POINT('Ctrl Pts',(-0.00970155423845781,0.126286451301922,
3.79376816284441));
#27929=CARTESIAN_POINT('Ctrl Pts',(0.0320381680834807,0.129492972475696,
3.79112160281878));
#27930=CARTESIAN_POINT('Ctrl Pts',(0.0755248974839926,0.109958464860738,
3.78847504279316));
#27931=CARTESIAN_POINT('Ctrl Pts',(0.10085090356394,0.0766256039927644,
3.78582848276753));
#27932=CARTESIAN_POINT('Ctrl Pts',(0.126176909643887,0.0432927431247909,
3.78318192274191));
#27933=CARTESIAN_POINT('Ctrl Pts',(0.13334219240327,-0.00383847099619805,
3.78053536271628));
#27934=CARTESIAN_POINT('Ctrl Pts',(0.119066566844655,-0.0431919042959778,
3.77788880269065));
#27935=CARTESIAN_POINT('Ctrl Pts',(0.10479094128604,-0.0825453375957573,
3.77524224266503));
#27936=CARTESIAN_POINT('Ctrl Pts',(0.0690744074094266,-0.114120990074327,
3.7725956826394));
#27937=CARTESIAN_POINT('Ctrl Pts',(0.0282675884266474,-0.123463886952785,
3.76994912261378));
#27938=CARTESIAN_POINT('Ctrl Pts',(-0.0125392305561318,-0.132806783831242,
3.76730256258815));
#27939=CARTESIAN_POINT('Ctrl Pts',(-0.0584363346450773,-0.119916925109586,
3.76465600256253));
#27940=CARTESIAN_POINT('Ctrl Pts',(-0.088412551309054,-0.0906951415895065,
3.7620094425369));
#27941=CARTESIAN_POINT('Ctrl Pts',(-0.112392263011044,-0.0673189446502994,
3.75989230590395));
#27942=CARTESIAN_POINT('Ctrl Pts',(-0.126183678849807,-0.0334914156074963,
3.75777516927101));
#27943=CARTESIAN_POINT('Ctrl Pts',(-0.126492921331233,0.000111898061355794,
3.75565803263806));
#27944=CARTESIAN_POINT('Ctrl Pts',(-0.126643738265873,-3.92119282522094E-5,
3.76934196736194));
#27945=CARTESIAN_POINT('Ctrl Pts',(-0.12665248162835,-0.00218746764357669,
3.76947773749816));
#27946=CARTESIAN_POINT('Ctrl Pts',(-0.126602553960315,-0.00433530847842783,
3.76961350763438));
#27947=CARTESIAN_POINT('Ctrl Pts',(-0.126492679803253,-0.0064800783217853,
3.7697492777706));
#27948=CARTESIAN_POINT('Ctrl Pts',(-0.124350908718499,-0.0482879625122638,
3.77239583779623));
#27949=CARTESIAN_POINT('Ctrl Pts',(-0.0994309722556023,-0.0889289468016232,
3.77504239782185));
#27950=CARTESIAN_POINT('Ctrl Pts',(-0.0631409340577098,-0.109798050553457,
3.77768895784748));
#27951=CARTESIAN_POINT('Ctrl Pts',(-0.0268508958598173,-0.130667154305292,
3.7803355178731));
#27952=CARTESIAN_POINT('Ctrl Pts',(0.0208092440730706,-0.131764377519601,
3.78298207789873));
#27953=CARTESIAN_POINT('Ctrl Pts',(0.0580212154414384,-0.112587423885904,
3.78562863792435));
#27954=CARTESIAN_POINT('Ctrl Pts',(0.0952331868098064,-0.0934104702522078,
3.78827519794998));
#27955=CARTESIAN_POINT('Ctrl Pts',(0.121996989613654,-0.0539593397705055,
3.7909217579756));
#27956=CARTESIAN_POINT('Ctrl Pts',(0.126060459158462,-0.0122943115177929,
3.79356831800123));
#27957=CARTESIAN_POINT('Ctrl Pts',(0.130123928703269,0.0293707167349194,
3.79621487802685));
#27958=CARTESIAN_POINT('Ctrl Pts',(0.111487064989038,0.073249642758642,
3.79886143805248));
#27959=CARTESIAN_POINT('Ctrl Pts',(0.0786816123755665,0.0992551929818185,
3.8015079980781));
#27960=CARTESIAN_POINT('Ctrl Pts',(0.0458761597620954,0.125260743204995,
3.80415455810373));
#27961=CARTESIAN_POINT('Ctrl Pts',(-0.00109788175061491,0.133392917627625,
3.80680111812935));
#27962=CARTESIAN_POINT('Ctrl Pts',(-0.0407363299210399,0.119928899273839,
3.80944767815498));
#27963=CARTESIAN_POINT('Ctrl Pts',(-0.0803747780914649,0.106464880920053,
3.81209423818061));
#27964=CARTESIAN_POINT('Ctrl Pts',(-0.112677632919605,0.071404669789851,
3.81474079820623));
#27965=CARTESIAN_POINT('Ctrl Pts',(-0.122857014657189,0.030798431934596,
3.81738735823185));
#27966=CARTESIAN_POINT('Ctrl Pts',(-0.125362998814015,0.0208018927186779,
3.81803889460855));
#27967=CARTESIAN_POINT('Ctrl Pts',(-0.126528173261855,0.0104692323861157,
3.81869043098525));
#27968=CARTESIAN_POINT('Ctrl Pts',(-0.12643411897368,0.000115681837355761,
3.81934196736194));
#27969=CARTESIAN_POINT('Origin',(0.,0.,3.7));
#27970=CARTESIAN_POINT('',(-0.126249985800877,-2.99474503126992E-5,3.86934196736194));
#27971=CARTESIAN_POINT('',(-0.126486618721746,-0.000112766438119152,3.85565803263806));
#27972=CARTESIAN_POINT('',(-0.12645,1.54856587752183E-17,3.7));
#27973=CARTESIAN_POINT('Ctrl Pts',(-0.126486618721746,-0.000112766438119152,
3.85565803263806));
#27974=CARTESIAN_POINT('Ctrl Pts',(-0.126178545401481,0.0332869000256312,
3.85355399621955));
#27975=CARTESIAN_POINT('Ctrl Pts',(-0.112575693492532,0.0669084342579941,
3.85144995980104));
#27976=CARTESIAN_POINT('Ctrl Pts',(-0.0888593841145145,0.0902573973319142,
3.84934592338254));
#27977=CARTESIAN_POINT('Ctrl Pts',(-0.0590278489741825,0.119626866304839,
3.84669936335691));
#27978=CARTESIAN_POINT('Ctrl Pts',(-0.0131949631210826,0.13274323742959,
3.84405280333129));
#27979=CARTESIAN_POINT('Ctrl Pts',(0.0276574994404428,0.123601984887668,
3.84140624330566));
#27980=CARTESIAN_POINT('Ctrl Pts',(0.0685099620019675,0.114460732345747,
3.83875968328004));
#27981=CARTESIAN_POINT('Ctrl Pts',(0.104382001271918,0.0830618561371527,
3.83611312325441));
#27982=CARTESIAN_POINT('Ctrl Pts',(0.118851805360766,0.0437794049828168,
3.83346656322878));
#27983=CARTESIAN_POINT('Ctrl Pts',(0.133321609449615,0.00449695382848087,
3.83082000320316));
#27984=CARTESIAN_POINT('Ctrl Pts',(0.126389178357361,-0.0426690722715969,
3.82817344317753));
#27985=CARTESIAN_POINT('Ctrl Pts',(0.101228100274691,-0.0761266027699533,
3.82552688315191));
#27986=CARTESIAN_POINT('Ctrl Pts',(0.0760670221920212,-0.10958413326831,
3.82288032312628));
#27987=CARTESIAN_POINT('Ctrl Pts',(0.0326772971189339,-0.129333168164945,
3.82023376310066));
#27988=CARTESIAN_POINT('Ctrl Pts',(-0.0090777520451555,-0.12633282374641,
3.81758720307503));
#27989=CARTESIAN_POINT('Ctrl Pts',(-0.0508328012092449,-0.123332479327876,
3.81494064304941));
#27990=CARTESIAN_POINT('Ctrl Pts',(-0.0909531744643365,-0.097582755594171,
3.81229408302378));
#27991=CARTESIAN_POINT('Ctrl Pts',(-0.111072220979832,-0.0608715833833843,
3.80964752299816));
#27992=CARTESIAN_POINT('Ctrl Pts',(-0.121181537898249,-0.0424251389139816,
3.80831769287812));
#27993=CARTESIAN_POINT('Ctrl Pts',(-0.126240898306005,-0.021211136130883,
3.80698786275809));
#27994=CARTESIAN_POINT('Ctrl Pts',(-0.126243465328102,1.71616150689059E-6,
3.80565803263806));
#27995=CARTESIAN_POINT('Ctrl Pts',(-0.12643411897368,0.000115681837355761,
3.81934196736194));
#27996=CARTESIAN_POINT('Ctrl Pts',(-0.126146121962456,-0.0315871960586303,
3.82133699101087));
#27997=CARTESIAN_POINT('Ctrl Pts',(-0.114051564760291,-0.0634859411452914,
3.8233320146598));
#27998=CARTESIAN_POINT('Ctrl Pts',(-0.0924926098500027,-0.0865303795699984,
3.82532703830873));
#27999=CARTESIAN_POINT('Ctrl Pts',(-0.0638929146582029,-0.117100688639029,
3.82797359833436));
#28000=CARTESIAN_POINT('Ctrl Pts',(-0.018637615627574,-0.132089042196783,
3.83062015835998));
#28001=CARTESIAN_POINT('Ctrl Pts',(0.0225559257731756,-0.124633942619396,
3.83326671838561));
#28002=CARTESIAN_POINT('Ctrl Pts',(0.0637494671739252,-0.117178843042008,
3.83591327841123));
#28003=CARTESIAN_POINT('Ctrl Pts',(0.100881250944795,-0.0872802903294789,
3.83855983843686));
#28004=CARTESIAN_POINT('Ctrl Pts',(0.116952768555385,-0.048625501544595,
3.84120639846248));
#28005=CARTESIAN_POINT('Ctrl Pts',(0.133024286165975,-0.00997071275971127,
3.84385295848811));
#28006=CARTESIAN_POINT('Ctrl Pts',(0.128035537616284,0.0374403120975275,
3.84649951851373));
#28007=CARTESIAN_POINT('Ctrl Pts',(0.10427031529219,0.0719033437884345,
3.84914607853936));
#28008=CARTESIAN_POINT('Ctrl Pts',(0.080505092968096,0.106366375479342,
3.85179263856498));
#28009=CARTESIAN_POINT('Ctrl Pts',(0.037963396869598,0.127881414003918,
3.85443919859061));
#28010=CARTESIAN_POINT('Ctrl Pts',(-0.003879668124188,0.126599121222081,
3.85708575861623));
#28011=CARTESIAN_POINT('Ctrl Pts',(-0.0457227331179738,0.125316828440245,
3.85973231864186));
#28012=CARTESIAN_POINT('Ctrl Pts',(-0.0868671670070475,0.101237204351996,
3.86237887866749));
#28013=CARTESIAN_POINT('Ctrl Pts',(-0.108477515623481,0.0653836233772192,
3.86502543869311));
#28014=CARTESIAN_POINT('Ctrl Pts',(-0.120226312608128,0.0458912749879413,
3.86646428158272));
#28015=CARTESIAN_POINT('Ctrl Pts',(-0.126201381437229,0.0229188749131541,
3.86790312447233));
#28016=CARTESIAN_POINT('Ctrl Pts',(-0.126249985800877,-2.99474503126992E-5,
3.86934196736194));
#28017=CARTESIAN_POINT('Origin',(0.,0.,3.7));
#28018=CARTESIAN_POINT('',(-0.126543984365092,-0.000100563349596846,3.91934196736194));
#28019=CARTESIAN_POINT('',(-0.126614009842867,6.71750503076223E-5,3.90565803263806));
#28020=CARTESIAN_POINT('',(-0.12645,1.54856587752183E-17,3.7));
#28021=CARTESIAN_POINT('Ctrl Pts',(-0.126614009842867,6.71750503076223E-5,
3.90565803263806));
#28022=CARTESIAN_POINT('Ctrl Pts',(-0.126638949568151,0.00394272317787337,
3.90541324973226));
#28023=CARTESIAN_POINT('Ctrl Pts',(-0.126476435154099,0.00781615144459198,
3.90516846682647));
#28024=CARTESIAN_POINT('Ctrl Pts',(-0.126119637661472,0.0116715998582211,
3.90492368392067));
#28025=CARTESIAN_POINT('Ctrl Pts',(-0.122261990910541,0.0533561922490439,
3.90227712389504));
#28026=CARTESIAN_POINT('Ctrl Pts',(-0.0956933418361204,0.0929390036289487,
3.89963056386942));
#28027=CARTESIAN_POINT('Ctrl Pts',(-0.0585765319889427,0.112299495998321,
3.89698400384379));
#28028=CARTESIAN_POINT('Ctrl Pts',(-0.0214597221417651,0.131659988367694,
3.89433744381817));
#28029=CARTESIAN_POINT('Ctrl Pts',(0.0262052484781696,0.130798161726534,
3.89169088379254));
#28030=CARTESIAN_POINT('Ctrl Pts',(0.0625979063415064,0.110108538679153,
3.88904432376692));
#28031=CARTESIAN_POINT('Ctrl Pts',(0.0989905642048431,0.089418915631772,
3.88639776374129));
#28032=CARTESIAN_POINT('Ctrl Pts',(0.124110909311582,0.04890149617817,3.88375120371567));
#28033=CARTESIAN_POINT('Ctrl Pts',(0.12645912901712,0.0071047004378325,
3.88110464369004));
#28034=CARTESIAN_POINT('Ctrl Pts',(0.128807348722658,-0.0346920953025048,
3.87845808366442));
#28035=CARTESIAN_POINT('Ctrl Pts',(0.108383443026996,-0.0777682673295779,
3.87581152363879));
#28036=CARTESIAN_POINT('Ctrl Pts',(0.0745372459479278,-0.102404036849921,
3.87316496361316));
#28037=CARTESIAN_POINT('Ctrl Pts',(0.0406910488688595,-0.127039806370264,
3.87051840358754));
#28038=CARTESIAN_POINT('Ctrl Pts',(-0.00657743959361464,-0.133235173383876,
3.86787184356191));
#28039=CARTESIAN_POINT('Ctrl Pts',(-0.0456292438338329,-0.118153967704968,
3.86522528353629));
#28040=CARTESIAN_POINT('Ctrl Pts',(-0.0846810480740508,-0.10307276202606,
3.86257872351066));
#28041=CARTESIAN_POINT('Ctrl Pts',(-0.115516168092013,-0.0667149836546316,
3.85993216348504));
#28042=CARTESIAN_POINT('Ctrl Pts',(-0.124018635887212,-0.0257248110583692,
3.85728560345941));
#28043=CARTESIAN_POINT('Ctrl Pts',(-0.125761573683066,-0.0173221539948553,
3.85674307985229));
#28044=CARTESIAN_POINT('Ctrl Pts',(-0.126566055107683,-0.00872483577640936,
3.85620055624518));
#28045=CARTESIAN_POINT('Ctrl Pts',(-0.126486618721746,-0.000112766438119152,
3.85565803263806));
#28046=CARTESIAN_POINT('Ctrl Pts',(-0.126249985800877,-2.99474503126992E-5,
3.86934196736194));
#28047=CARTESIAN_POINT('Ctrl Pts',(-0.126290782696275,-0.01929242997697,
3.87054968449796));
#28048=CARTESIAN_POINT('Ctrl Pts',(-0.12215616704665,-0.0385383011374065,
3.87175740163397));
#28049=CARTESIAN_POINT('Ctrl Pts',(-0.113755815955893,-0.0556956374040618,
3.87296511876998));
#28050=CARTESIAN_POINT('Ctrl Pts',(-0.0953475043280787,-0.0932937793492606,
3.87561167879561));
#28051=CARTESIAN_POINT('Ctrl Pts',(-0.0564546177286578,-0.120862525378353,
3.87825823882124));
#28052=CARTESIAN_POINT('Ctrl Pts',(-0.0148818774258165,-0.125781231309797,
3.88090479884686));
#28053=CARTESIAN_POINT('Ctrl Pts',(0.0266908628770249,-0.13069993724124,
3.88355135887249));
#28054=CARTESIAN_POINT('Ctrl Pts',(0.0709434568832867,-0.112968603075036,
3.88619791889811));
#28055=CARTESIAN_POINT('Ctrl Pts',(0.0976175698612337,-0.0807044039779288,
3.88884447892374));
#28056=CARTESIAN_POINT('Ctrl Pts',(0.124291682839181,-0.0484402048808214,
3.89149103894936));
#28057=CARTESIAN_POINT('Ctrl Pts',(0.133387314788813,-0.00164314085281106,
3.89413759897499));
#28058=CARTESIAN_POINT('Ctrl Pts',(0.120740589231085,0.0382635693618544,
3.89678415900061));
#28059=CARTESIAN_POINT('Ctrl Pts',(0.108093863673357,0.0781702795765198,
3.89943071902624));
#28060=CARTESIAN_POINT('Ctrl Pts',(0.0737047806082696,0.11118663597784,
3.90207727905187));
#28061=CARTESIAN_POINT('Ctrl Pts',(0.0333162705051194,0.122198232868137,
3.90472383907749));
#28062=CARTESIAN_POINT('Ctrl Pts',(-0.00707223959803082,0.133209829758434,
3.90737039910312));
#28063=CARTESIAN_POINT('Ctrl Pts',(-0.0534601767392434,0.122216667137707,
3.91001695912874));
#28064=CARTESIAN_POINT('Ctrl Pts',(-0.0846116689345932,0.0942510810621984,
3.91266351915437));
#28065=CARTESIAN_POINT('Ctrl Pts',(-0.110814692885301,0.0707278765512593,
3.91488966855689));
#28066=CARTESIAN_POINT('Ctrl Pts',(-0.126237468513852,0.0351961661111841,
3.91711581795942));
#28067=CARTESIAN_POINT('Ctrl Pts',(-0.126543984365092,-0.000100563349596846,
3.91934196736194));
#28068=CARTESIAN_POINT('Origin',(0.,0.,3.7));
#28069=CARTESIAN_POINT('',(-0.126567406925801,8.9117089303592E-5,3.96934196736194));
#28070=CARTESIAN_POINT('',(-0.126283770505697,7.06948412972308E-5,3.95565803263806));
#28071=CARTESIAN_POINT('',(-0.12645,1.54856587752183E-17,3.7));
#28072=CARTESIAN_POINT('',(0.0958116152722338,0.0825211298936549,4.));
#28073=CARTESIAN_POINT('Ctrl Pts',(-0.126567406925801,8.9117089303592E-5,
3.96934196736194));
#28074=CARTESIAN_POINT('Ctrl Pts',(-0.126271512495954,-0.03602989561222,
3.97162163149775));
#28075=CARTESIAN_POINT('Ctrl Pts',(-0.11000667585855,-0.0723734458913716,
3.97390129563356));
#28076=CARTESIAN_POINT('Ctrl Pts',(-0.0826932529987204,-0.0959262598695684,
3.97618095976937));
#28077=CARTESIAN_POINT('Ctrl Pts',(-0.0509839270641226,-0.123269733404333,
3.978827519795));
#28078=CARTESIAN_POINT('Ctrl Pts',(-0.0043834430999392,-0.133373998977298,
3.98147407982063));
#28079=CARTESIAN_POINT('Ctrl Pts',(0.0357753280219188,-0.121524403040669,
3.98412063984625));
#28080=CARTESIAN_POINT('Ctrl Pts',(0.0759340991437768,-0.109674807104039,
3.98676719987188));
#28081=CARTESIAN_POINT('Ctrl Pts',(0.109651157423309,-0.0758713496578151,
3.9894137598975));
#28082=CARTESIAN_POINT('Ctrl Pts',(0.121481684447537,-0.0357885393155276,
3.99206031992312));
#28083=CARTESIAN_POINT('Ctrl Pts',(0.133312211471764,0.00429427102675994,
3.99470687994875));
#28084=CARTESIAN_POINT('Ctrl Pts',(0.123256207240687,0.0506564342651108,
3.99735343997437));
#28085=CARTESIAN_POINT('Ctrl Pts',(0.095811615272233,0.0825211298936557,
4.));
#28086=CARTESIAN_POINT('',(-0.0959939867336434,0.082660026050108,4.));
#28087=CARTESIAN_POINT('Origin',(0.,0.,4.));
#28088=CARTESIAN_POINT('Ctrl Pts',(-0.095994151316856,0.0826601513985344,
4.));
#28089=CARTESIAN_POINT('Ctrl Pts',(-0.0693049200029063,0.113544200686508,
3.9974200549221));
#28090=CARTESIAN_POINT('Ctrl Pts',(-0.0262885035315151,0.130447365396717,
3.9948401098442));
#28091=CARTESIAN_POINT('Ctrl Pts',(0.0142676559974625,0.125842964228272,
3.9922601647663));
#28092=CARTESIAN_POINT('Ctrl Pts',(0.0558709876039151,0.121119676054917,
3.98961360474068));
#28093=CARTESIAN_POINT('Ctrl Pts',(0.0948853729157606,0.0937638197023474,
3.98696704471505));
#28094=CARTESIAN_POINT('Ctrl Pts',(0.113475682659087,0.0562620533584955,
3.98432048468943));
#28095=CARTESIAN_POINT('Ctrl Pts',(0.132065992402412,0.0187602870146438,
3.9816739246638));
#28096=CARTESIAN_POINT('Ctrl Pts',(0.130232226577219,-0.0288873893204904,
3.97902736463818));
#28097=CARTESIAN_POINT('Ctrl Pts',(0.108800980591427,-0.0648498109281795,
3.97638080461255));
#28098=CARTESIAN_POINT('Ctrl Pts',(0.0873697346056348,-0.100812232535869,
3.97373424458693));
#28099=CARTESIAN_POINT('Ctrl Pts',(0.046341008459244,-0.125089399416112,
3.9710876845613));
#28100=CARTESIAN_POINT('Ctrl Pts',(0.00450388209284308,-0.126577017215687,
3.96844112453568));
#28101=CARTESIAN_POINT('Ctrl Pts',(-0.0373332442735578,-0.128064635015261,
3.96579456451005));
#28102=CARTESIAN_POINT('Ctrl Pts',(-0.0799787708599689,-0.106762703734165,
3.96314800448442));
#28103=CARTESIAN_POINT('Ctrl Pts',(-0.103913438592044,-0.0724181315163075,
3.9605014444588));
#28104=CARTESIAN_POINT('Ctrl Pts',(-0.118514209844363,-0.0514670471592998,
3.95888697385188));
#28105=CARTESIAN_POINT('Ctrl Pts',(-0.126152075437054,-0.0256623813017284,
3.95727250324497));
#28106=CARTESIAN_POINT('Ctrl Pts',(-0.126283770505697,7.06948412972308E-5,
3.95565803263806));
#28107=CARTESIAN_POINT('Origin',(0.,0.,4.11042117235887));
#28108=CARTESIAN_POINT('',(-0.154553716617854,1.07385516829317E-5,3.53957882764113));
#28109=CARTESIAN_POINT('',(-0.154050307343621,3.81371511608408E-5,3.53542117235887));
#28110=CARTESIAN_POINT('',(-0.1543,7.47606542906876E-15,4.11042117235887));
#28111=CARTESIAN_POINT('',(0.0398513841857357,-0.149064942821848,3.5));
#28112=CARTESIAN_POINT('Ctrl Pts',(-0.154050307343621,3.81371511608431E-5,
3.53542117235887));
#28113=CARTESIAN_POINT('Ctrl Pts',(-0.154093326879583,0.0238011172149125,
3.53420035500841));
#28114=CARTESIAN_POINT('Ctrl Pts',(-0.137743852801688,0.0990167675561842,
3.53033297763233));
#28115=CARTESIAN_POINT('Ctrl Pts',(-0.0205691901156568,0.181176596665036,
3.52381904023063));
#28116=CARTESIAN_POINT('Ctrl Pts',(0.141207069227503,0.115615351338242,
3.51587936015375));
#28117=CARTESIAN_POINT('Ctrl Pts',(0.173454096992073,-0.0561631599472297,
3.50793968007688));
#28118=CARTESIAN_POINT('Ctrl Pts',(0.089426887306191,-0.135811307301286,
3.50264656002563));
#28119=CARTESIAN_POINT('Ctrl Pts',(0.0398513841857336,-0.149064942821849,
3.5));
#28120=CARTESIAN_POINT('',(-0.0398513841857265,-0.149064942821851,3.5));
#28121=CARTESIAN_POINT('Origin',(0.,0.,3.5));
#28122=CARTESIAN_POINT('Ctrl Pts',(-0.154553716617854,1.07385516829459E-5,
3.53957882764113));
#28123=CARTESIAN_POINT('Ctrl Pts',(-0.154554183576509,0.000527195138975443,
3.53955207027449));
#28124=CARTESIAN_POINT('Ctrl Pts',(-0.154317915988944,0.0521256879879336,
3.53687875288222));
#28125=CARTESIAN_POINT('Ctrl Pts',(-0.0973408901199132,0.154229940417525,
3.53155887546432));
#28126=CARTESIAN_POINT('Ctrl Pts',(0.0768181056158631,0.16543527210962,
3.52361919538745));
#28127=CARTESIAN_POINT('Ctrl Pts',(0.180643771975638,0.0251157687415861,
3.51567951531057));
#28128=CARTESIAN_POINT('Ctrl Pts',(0.119593430082514,-0.13672026231454,
3.50780645018142));
#28129=CARTESIAN_POINT('Ctrl Pts',(0.00819996357198913,-0.162114976519676,
3.5025799450779));
#28130=CARTESIAN_POINT('Ctrl Pts',(-0.0399398165374138,-0.14933059314829,
3.5));
#28131=CARTESIAN_POINT('Origin',(0.,0.,4.11042117235887));
#28132=CARTESIAN_POINT('',(-0.15419083216807,0.000129561635314926,3.58957882764113));
#28133=CARTESIAN_POINT('',(-0.154288256028425,-0.000141223516069758,3.58542117235887));
#28134=CARTESIAN_POINT('',(-0.1543,7.47606542906876E-15,4.11042117235887));
#28135=CARTESIAN_POINT('Ctrl Pts',(-0.154288256028425,-0.000141223516069763,
3.58542117235887));
#28136=CARTESIAN_POINT('Ctrl Pts',(-0.153932746614783,0.0387932487575316,
3.5834130484955));
#28137=CARTESIAN_POINT('Ctrl Pts',(-0.119227247372343,0.129604846059009,
3.57875836460651));
#28138=CARTESIAN_POINT('Ctrl Pts',(0.0333654249967142,0.179306991453011,
3.57145712069188));
#28139=CARTESIAN_POINT('Ctrl Pts',(0.16875469474836,0.0691889591605158,
3.56351744061501));
#28140=CARTESIAN_POINT('Ctrl Pts',(0.149631713131164,-0.104283094234219,
3.55557776053813));
#28141=CARTESIAN_POINT('Ctrl Pts',(-0.00648228852693025,-0.182263845309582,
3.54763808046125));
#28142=CARTESIAN_POINT('Ctrl Pts',(-0.133583343879226,-0.107056676726779,
3.54091921773484));
#28143=CARTESIAN_POINT('Ctrl Pts',(-0.154000066586259,-0.0277136758071254,
3.53684691503404));
#28144=CARTESIAN_POINT('Ctrl Pts',(-0.154050307343621,3.81371511608431E-5,
3.53542117235887));
#28145=CARTESIAN_POINT('Ctrl Pts',(-0.15419083216807,0.000129561635314916,
3.58957882764113));
#28146=CARTESIAN_POINT('Ctrl Pts',(-0.154316540000352,0.0159383321389732,
3.58876476376157));
#28147=CARTESIAN_POINT('Ctrl Pts',(-0.144808574808872,0.0829945710278969,
3.58530413985639));
#28148=CARTESIAN_POINT('Ctrl Pts',(-0.0479747871584019,0.175962994372803,
3.57919695592558));
#28149=CARTESIAN_POINT('Ctrl Pts',(0.121839171429706,0.13571993663382,3.5712572758487));
#28150=CARTESIAN_POINT('Ctrl Pts',(0.180099946935509,-0.0287862221383337,
3.56331759577183));
#28151=CARTESIAN_POINT('Ctrl Pts',(0.0734653204375665,-0.166934393666355,
3.55537791569495));
#28152=CARTESIAN_POINT('Ctrl Pts',(-0.0998464626320651,-0.152294592499083,
3.54746499298472));
#28153=CARTESIAN_POINT('Ctrl Pts',(-0.154507996889821,-0.0505553114913108,
3.54219863030011));
#28154=CARTESIAN_POINT('Ctrl Pts',(-0.154553716617854,1.07385516829459E-5,
3.53957882764113));
#28155=CARTESIAN_POINT('Origin',(0.,0.,4.11042117235887));
#28156=CARTESIAN_POINT('',(-0.154093198061062,-8.33060061860361E-5,3.63957882764113));
#28157=CARTESIAN_POINT('',(-0.154532949196129,5.22176212347235E-5,3.63542117235887));
#28158=CARTESIAN_POINT('',(-0.1543,7.47606542906876E-15,4.11042117235887));
#28159=CARTESIAN_POINT('Ctrl Pts',(-0.154532949196129,5.22176212347084E-5,
3.63542117235887));
#28160=CARTESIAN_POINT('Ctrl Pts',(-0.154545584588578,0.00292672178698735,
3.63527230200821));
#28161=CARTESIAN_POINT('Ctrl Pts',(-0.153169988902963,0.0568907246896308,
3.63247687163192));
#28162=CARTESIAN_POINT('Ctrl Pts',(-0.0901397813258339,0.158554191001936,
3.62703488123002));
#28163=CARTESIAN_POINT('Ctrl Pts',(0.0843490755327352,0.161709110561297,
3.61909520115314));
#28164=CARTESIAN_POINT('Ctrl Pts',(0.181609876119891,0.0168069020193158,
3.61115552107626));
#28165=CARTESIAN_POINT('Ctrl Pts',(0.11259272547993,-0.14348343554309,3.60321584099938));
#28166=CARTESIAN_POINT('Ctrl Pts',(-0.0595116136917225,-0.1724033835878,
3.59527616092251));
#28167=CARTESIAN_POINT('Ctrl Pts',(-0.147380741016298,-0.0760839947500021,
3.58934460470901));
#28168=CARTESIAN_POINT('Ctrl Pts',(-0.154401281957667,-0.0125195312047306,
3.58605960852113));
#28169=CARTESIAN_POINT('Ctrl Pts',(-0.154288256028425,-0.000141223516069763,
3.58542117235887));
#28170=CARTESIAN_POINT('Ctrl Pts',(-0.154093198061063,-8.33060061860274E-5,
3.63957882764113));
#28171=CARTESIAN_POINT('Ctrl Pts',(-0.153940587938977,0.0310641981069166,
3.63797745724865));
#28172=CARTESIAN_POINT('Ctrl Pts',(-0.129646233104354,0.113907608400038,
3.63372952683056));
#28173=CARTESIAN_POINT('Ctrl Pts',(0.00558664719359638,0.182300288895857,
3.62683503638684));
#28174=CARTESIAN_POINT('Ctrl Pts',(0.156205528517827,0.094151159125646,
3.61889535630996));
#28175=CARTESIAN_POINT('Ctrl Pts',(0.163806179027695,-0.0802006497663837,
3.61095567623308));
#28176=CARTESIAN_POINT('Ctrl Pts',(0.0214296163208854,-0.181122531330724,
3.60301599615621));
#28177=CARTESIAN_POINT('Ctrl Pts',(-0.123957687612568,-0.122868073634794,
3.59589037995889));
#28178=CARTESIAN_POINT('Ctrl Pts',(-0.1539078579151,-0.0354567255707862,
3.5914113237872));
#28179=CARTESIAN_POINT('Ctrl Pts',(-0.15419083216807,0.000129561635314916,
3.58957882764113));
#28180=CARTESIAN_POINT('Origin',(0.,0.,4.11042117235887));
#28181=CARTESIAN_POINT('',(-0.154494739391599,-8.56666717596894E-5,3.68957882764113));
#28182=CARTESIAN_POINT('',(-0.15413359010754,0.000108847378321225,3.68542117235887));
#28183=CARTESIAN_POINT('',(-0.1543,7.47606542906876E-15,4.11042117235887));
#28184=CARTESIAN_POINT('Ctrl Pts',(-0.15413359010754,0.00010884737832121,
3.68542117235887));
#28185=CARTESIAN_POINT('Ctrl Pts',(-0.154252061492927,0.0183060191525707,
3.6844849954953));
#28186=CARTESIAN_POINT('Ctrl Pts',(-0.142855501009428,0.0878027720491901,
3.6809022586061));
#28187=CARTESIAN_POINT('Ctrl Pts',(-0.039826269011209,0.177984489264188,
3.67467296169127));
#28188=CARTESIAN_POINT('Ctrl Pts',(0.127955809817362,0.129968921992697,
3.66673328161439));
#28189=CARTESIAN_POINT('Ctrl Pts',(0.178584458888466,-0.0370432344610292,
3.65879360153752));
#28190=CARTESIAN_POINT('Ctrl Pts',(0.0657052360091523,-0.170139449612234,
3.65085392146064));
#28191=CARTESIAN_POINT('Ctrl Pts',(-0.104087723049408,-0.147885095147454,
3.64306311173443));
#28192=CARTESIAN_POINT('Ctrl Pts',(-0.154320957425313,-0.0481751113503961,
3.63791886203384));
#28193=CARTESIAN_POINT('Ctrl Pts',(-0.154532949196129,5.22176212347084E-5,
3.63542117235887));
#28194=CARTESIAN_POINT('Ctrl Pts',(-0.154494739391599,-8.56666717596998E-5,
3.68957882764113));
#28195=CARTESIAN_POINT('Ctrl Pts',(-0.15418701910941,0.0460669561753479,
3.68719015073574));
#28196=CARTESIAN_POINT('Ctrl Pts',(-0.107714707332757,0.143892491682726,
3.68215491380472));
#28197=CARTESIAN_POINT('Ctrl Pts',(0.0586595287281965,0.172695299861449,
3.67447311684809));
#28198=CARTESIAN_POINT('Ctrl Pts',(0.176911729524118,0.0443491475303153,
3.66653343677121));
#28199=CARTESIAN_POINT('Ctrl Pts',(0.133187572742707,-0.124602076359984,
3.65859375669434));
#28200=CARTESIAN_POINT('Ctrl Pts',(-0.0324800977009374,-0.179470471240069,
3.65065407661746));
#28201=CARTESIAN_POINT('Ctrl Pts',(-0.140993802389242,-0.0920951181032393,
3.64431576693306));
#28202=CARTESIAN_POINT('Ctrl Pts',(-0.154192804322217,-0.0204127991394723,
3.64062401727428));
#28203=CARTESIAN_POINT('Ctrl Pts',(-0.154093198061063,-8.33060061860274E-5,
3.63957882764113));
#28204=CARTESIAN_POINT('Origin',(0.,0.,4.11042117235887));
#28205=CARTESIAN_POINT('',(-0.154352374546534,0.000136543067356262,3.73957882764113));
#28206=CARTESIAN_POINT('',(-0.154139174508622,-0.000111501026995055,3.73542117235887));
#28207=CARTESIAN_POINT('',(-0.1543,7.47606542906876E-15,4.11042117235887));
#28208=CARTESIAN_POINT('Ctrl Pts',(-0.154139174508622,-0.000111501026995059,
3.73542117235887));
#28209=CARTESIAN_POINT('Ctrl Pts',(-0.153915233552703,0.0333860868580806,
3.73369768898238));
#28210=CARTESIAN_POINT('Ctrl Pts',(-0.1267153517394,0.118653316414882,3.72932764558026));
#28211=CARTESIAN_POINT('Ctrl Pts',(0.0139700521550768,0.18185006934563,
3.72231104215253));
#28212=CARTESIAN_POINT('Ctrl Pts',(0.160372810275332,0.0868629483698537,
3.71437136207565));
#28213=CARTESIAN_POINT('Ctrl Pts',(0.15994186929589,-0.087653913339944,
3.70643168199877));
#28214=CARTESIAN_POINT('Ctrl Pts',(0.013071788942189,-0.181916844788939,
3.6984920019219));
#28215=CARTESIAN_POINT('Ctrl Pts',(-0.127037714877433,-0.11814535336758,
3.6914884987086));
#28216=CARTESIAN_POINT('Ctrl Pts',(-0.153917144400928,-0.0331371528280101,
3.68713155552092));
#28217=CARTESIAN_POINT('Ctrl Pts',(-0.15413359010754,0.00010884737832121,
3.68542117235887));
#28218=CARTESIAN_POINT('Ctrl Pts',(-0.154352374546534,0.000136543067356257,
3.73957882764113));
#28219=CARTESIAN_POINT('Ctrl Pts',(-0.154446737273245,0.0103903099163322,
3.73904940424845));
#28220=CARTESIAN_POINT('Ctrl Pts',(-0.148841316561083,0.0717994892151511,
3.73587342083015));
#28221=CARTESIAN_POINT('Ctrl Pts',(-0.0665446905722607,0.169812870767156,
3.73005087738622));
#28222=CARTESIAN_POINT('Ctrl Pts',(0.106602640202898,0.147988121222216,
3.72211119730934));
#28223=CARTESIAN_POINT('Ctrl Pts',(0.182147017152552,-0.0093311876933208,
3.71417151723247));
#28224=CARTESIAN_POINT('Ctrl Pts',(0.0909217261957518,-0.158107073301583,
3.70623183715559));
#28225=CARTESIAN_POINT('Ctrl Pts',(-0.0835494302172658,-0.162123717048593,
3.69829215707872));
#28226=CARTESIAN_POINT('Ctrl Pts',(-0.152048491522357,-0.0611528114853893,
3.69274115390723));
#28227=CARTESIAN_POINT('Ctrl Pts',(-0.154527961074428,-0.00506833400535766,
3.68983671076137));
#28228=CARTESIAN_POINT('Ctrl Pts',(-0.154494739391599,-8.56666717596998E-5,
3.68957882764113));
#28229=CARTESIAN_POINT('Origin',(0.,0.,4.11042117235887));
#28230=CARTESIAN_POINT('',(-0.154047977067031,2.09413777367551E-6,3.78957882764113));
#28231=CARTESIAN_POINT('',(-0.154536408180499,-4.7848165513455E-5,3.78542117235887));
#28232=CARTESIAN_POINT('',(-0.1543,7.47606542906876E-15,4.11042117235887));
#28233=CARTESIAN_POINT('Ctrl Pts',(-0.154536408180499,-4.78481655134459E-5,
3.78542117235887));
#28234=CARTESIAN_POINT('Ctrl Pts',(-0.154339106087067,0.0484295369338371,
3.78291038246947));
#28235=CARTESIAN_POINT('Ctrl Pts',(-0.103641790719782,0.148361335894058,
3.77775303255443));
#28236=CARTESIAN_POINT('Ctrl Pts',(0.0665446937287967,0.169812878822259,
3.76994912261378));
#28237=CARTESIAN_POINT('Ctrl Pts',(0.178765223990991,0.0361608181406009,
3.7620094425369));
#28238=CARTESIAN_POINT('Ctrl Pts',(0.127312379282745,-0.130599265535886,
3.75406976246003));
#28239=CARTESIAN_POINT('Ctrl Pts',(-0.0407047855299705,-0.177785630781348,
3.74613008238315));
#28240=CARTESIAN_POINT('Ctrl Pts',(-0.143071654254016,-0.0872869087240706,
3.73991388568277));
#28241=CARTESIAN_POINT('Ctrl Pts',(-0.154259114549828,-0.0180524000230757,
3.73634424900801));
#28242=CARTESIAN_POINT('Ctrl Pts',(-0.154139174508622,-0.000111501026995059,
3.73542117235887));
#28243=CARTESIAN_POINT('Ctrl Pts',(-0.154047977067031,2.09413777367898E-6,
3.78957882764113));
#28244=CARTESIAN_POINT('Ctrl Pts',(-0.154051078605937,0.0256319813134887,
3.78826209773554));
#28245=CARTESIAN_POINT('Ctrl Pts',(-0.135851564244815,0.102772493157479,
3.78429880780432));
#28246=CARTESIAN_POINT('Ctrl Pts',(-0.013970051492431,0.181850060719556,
3.77768895784748));
#28247=CARTESIAN_POINT('Ctrl Pts',(0.145223361235896,0.110339395832533,
3.7697492777706));
#28248=CARTESIAN_POINT('Ctrl Pts',(0.171453565975463,-0.0621955113766863,
3.76180959769372));
#28249=CARTESIAN_POINT('Ctrl Pts',(0.0407047835991549,-0.177785622348059,
3.75386991761685));
#28250=CARTESIAN_POINT('Ctrl Pts',(-0.11610887230377,-0.133745678862782,
3.74645966093265));
#28251=CARTESIAN_POINT('Ctrl Pts',(-0.153975022906486,-0.0408677376689339,
3.74169596427408));
#28252=CARTESIAN_POINT('Ctrl Pts',(-0.154352374546534,0.000136543067356257,
3.73957882764113));
#28253=CARTESIAN_POINT('Origin',(0.,0.,4.11042117235887));
#28254=CARTESIAN_POINT('',(-0.154344683817836,-0.000137602699895489,3.83957882764113));
#28255=CARTESIAN_POINT('',(-0.154280621254558,0.000141160201694546,3.83542117235887));
#28256=CARTESIAN_POINT('',(-0.1543,7.47606542906876E-15,4.11042117235887));
#28257=CARTESIAN_POINT('Ctrl Pts',(-0.154280621254558,0.000141160201694572,
3.83542117235887));
#28258=CARTESIAN_POINT('Ctrl Pts',(-0.154395390544122,0.0127750301081681,
3.83476963598218));
#28259=CARTESIAN_POINT('Ctrl Pts',(-0.147198204620896,0.0765990159781269,
3.83147153957986));
#28260=CARTESIAN_POINT('Ctrl Pts',(-0.0586595315107243,0.172695308053416,
3.82552688315191));
#28261=CARTESIAN_POINT('Ctrl Pts',(0.113300008356683,0.142925568707939,
3.81758720307504));
#28262=CARTESIAN_POINT('Ctrl Pts',(0.181524636378177,-0.0177035721096275,
3.80964752299816));
#28263=CARTESIAN_POINT('Ctrl Pts',(0.0835494341804624,-0.162123724738966,
3.80170784292129));
#28264=CARTESIAN_POINT('Ctrl Pts',(-0.0909217305086156,-0.158107080801413,
3.7937681628444));
#28265=CARTESIAN_POINT('Ctrl Pts',(-0.15329856504372,-0.056379054482583,
3.78833927265694));
#28266=CARTESIAN_POINT('Ctrl Pts',(-0.154547077226211,-0.00266924679639216,
3.78555694249509));
#28267=CARTESIAN_POINT('Ctrl Pts',(-0.154536408180499,-4.78481655134459E-5,
3.78542117235887));
#28268=CARTESIAN_POINT('Ctrl Pts',(-0.154344683817836,-0.000137602699895493,
3.83957882764113));
#28269=CARTESIAN_POINT('Ctrl Pts',(-0.153968758841032,0.0406181785207979,
3.83747479122262));
#28270=CARTESIAN_POINT('Ctrl Pts',(-0.11649114353226,0.133249851238064,
3.83272419477849));
#28271=CARTESIAN_POINT('Ctrl Pts',(0.039826267121788,0.177984480821945,
3.82532703830873));
#28272=CARTESIAN_POINT('Ctrl Pts',(0.171144313607041,0.063041501012073,
3.81738735823185));
#28273=CARTESIAN_POINT('Ctrl Pts',(0.145766517224248,-0.109620843643728,
3.80944767815498));
#28274=CARTESIAN_POINT('Ctrl Pts',(-0.0130717883220708,-0.181916836159762,
3.8015079980781));
#28275=CARTESIAN_POINT('Ctrl Pts',(-0.135584681571728,-0.103286631626578,
3.79488504790682));
#28276=CARTESIAN_POINT('Ctrl Pts',(-0.154044844670753,-0.0258827861209538,
3.79090865776116));
#28277=CARTESIAN_POINT('Ctrl Pts',(-0.154047977067031,2.09413777367898E-6,
3.78957882764113));
#28278=CARTESIAN_POINT('Origin',(0.,0.,4.11042117235887));
#28279=CARTESIAN_POINT('',(-0.154500132216325,8.19700297638587E-5,3.88957882764113));
#28280=CARTESIAN_POINT('',(-0.154055933642351,-3.65432311820964E-5,3.88542117235887));
#28281=CARTESIAN_POINT('',(-0.1543,7.47606542906876E-15,4.11042117235887));
#28282=CARTESIAN_POINT('Ctrl Pts',(-0.154055933642351,-3.6543231182122E-5,
3.88542117235887));
#28283=CARTESIAN_POINT('Ctrl Pts',(-0.15399662440304,0.0279666460980613,
3.88398232946926));
#28284=CARTESIAN_POINT('Ctrl Pts',(-0.133294661580101,0.10755966601202,
3.87989692655402));
#28285=CARTESIAN_POINT('Ctrl Pts',(-0.005586647457645,0.182300297549597,
3.87316496361317));
#28286=CARTESIAN_POINT('Ctrl Pts',(0.150147248343024,0.103539432915148,
3.86522528353629));
#28287=CARTESIAN_POINT('Ctrl Pts',(0.168409737102627,-0.0700197873807462,
3.85728560345941));
#28288=CARTESIAN_POINT('Ctrl Pts',(0.0324800992415292,-0.179470479754251,
3.84934592338254));
#28289=CARTESIAN_POINT('Ctrl Pts',(-0.1195927593937,-0.129104626018084,
3.84205777968236));
#28290=CARTESIAN_POINT('Ctrl Pts',(-0.153929194296616,-0.0385441229881096,
3.8374161960078));
#28291=CARTESIAN_POINT('Ctrl Pts',(-0.154280621254558,0.000141160201694572,
3.83542117235887));
#28292=CARTESIAN_POINT('Ctrl Pts',(-0.154500132216325,8.19700297638379E-5,
3.88957882764113));
#28293=CARTESIAN_POINT('Ctrl Pts',(-0.1545305647953,0.00481108885999716,
3.88933404473533));
#28294=CARTESIAN_POINT('Ctrl Pts',(-0.152188184006249,0.0606402533846132,
3.88644270180391));
#28295=CARTESIAN_POINT('Ctrl Pts',(-0.0843490715154628,0.161709102853824,
3.88090479884686));
#28296=CARTESIAN_POINT('Ctrl Pts',(0.0901397770410241,0.158554183500776,
3.87296511876998));
#28297=CARTESIAN_POINT('Ctrl Pts',(0.182098715355847,0.0102306290122647,
3.86502543869311));
#28298=CARTESIAN_POINT('Ctrl Pts',(0.107332199369115,-0.147459841777235,
3.85708575861623));
#28299=CARTESIAN_POINT('Ctrl Pts',(-0.0657052328909015,-0.17013944154474,
3.84914607853936));
#28300=CARTESIAN_POINT('Ctrl Pts',(-0.148671156397415,-0.0723140833987834,
3.84331043488099));
#28301=CARTESIAN_POINT('Ctrl Pts',(-0.154441615683002,-0.0106464385947012,
3.84012135124824));
#28302=CARTESIAN_POINT('Ctrl Pts',(-0.154344683817836,-0.000137602699895493,
3.83957882764113));
#28303=CARTESIAN_POINT('Origin',(0.,0.,4.11042117235887));
#28304=CARTESIAN_POINT('',(-0.154097159264761,8.62650376686758E-5,3.93957882764113));
#28305=CARTESIAN_POINT('',(-0.154414683966261,-0.000122711940234539,3.93542117235887));
#28306=CARTESIAN_POINT('',(-0.1543,7.47606542906876E-15,4.11042117235887));
#28307=CARTESIAN_POINT('Ctrl Pts',(-0.154414683966261,-0.00012271194023455,
3.93542117235887));
#28308=CARTESIAN_POINT('Ctrl Pts',(-0.15404065948349,0.0429479512135688,
3.93319502295635));
#28309=CARTESIAN_POINT('Ctrl Pts',(-0.11284743018063,0.1378508358131,3.9283223135282));
#28310=CARTESIAN_POINT('Ctrl Pts',(0.0479747894892283,0.175963002958517,
3.92080304407442));
#28311=CARTESIAN_POINT('Ctrl Pts',(0.173864125597012,0.0550988560374321,
3.91286336399754));
#28312=CARTESIAN_POINT('Ctrl Pts',(0.140567423109983,-0.116212816074597,
3.90492368392067));
#28313=CARTESIAN_POINT('Ctrl Pts',(-0.0214296173447312,-0.181122539961793,
3.89698400384379));
#28314=CARTESIAN_POINT('Ctrl Pts',(-0.138004452641611,-0.0984898965999405,
3.89048316665653));
#28315=CARTESIAN_POINT('Ctrl Pts',(-0.154105715856349,-0.0235414942304966,
3.88662888949489));
#28316=CARTESIAN_POINT('Ctrl Pts',(-0.154055933642351,-3.6543231182122E-5,
3.88542117235887));
#28317=CARTESIAN_POINT('Ctrl Pts',(-0.154097159264761,8.62650376686723E-5,
3.93957882764113));
#28318=CARTESIAN_POINT('Ctrl Pts',(-0.154199890802351,0.0201598980625174,
3.93854673822241));
#28319=CARTESIAN_POINT('Ctrl Pts',(-0.141224360537215,0.0915805799143205,
3.93486808877808));
#28320=CARTESIAN_POINT('Ctrl Pts',(-0.0333654229848094,0.179306981584077,
3.92854287930812));
#28321=CARTESIAN_POINT('Ctrl Pts',(0.132570265831228,0.125258780485074,
3.92060319923124));
#28322=CARTESIAN_POINT('Ctrl Pts',(0.17712875926901,-0.0434751369680033,
3.91266351915436));
#28323=CARTESIAN_POINT('Ctrl Pts',(0.059511610779771,-0.172403375181386,
3.90472383907749));
#28324=CARTESIAN_POINT('Ctrl Pts',(-0.107286687880009,-0.144375040164272,
3.89702894190641));
#28325=CARTESIAN_POINT('Ctrl Pts',(-0.154201531823291,-0.0463195111784584,
3.89198060476095));
#28326=CARTESIAN_POINT('Ctrl Pts',(-0.154500132216325,8.19700297638379E-5,
3.88957882764113));
#28327=CARTESIAN_POINT('Origin',(0.,0.,4.11042117235887));
#28328=CARTESIAN_POINT('',(-0.154145398954164,-0.00018319008806407,3.98957882764113));
#28329=CARTESIAN_POINT('',(-0.154443265232512,0.000108744696557919,3.98542117235887));
#28330=CARTESIAN_POINT('',(-0.1543,7.47606542906876E-15,4.11042117235887));
#28331=CARTESIAN_POINT('',(-0.0398513841857263,-0.149064942821851,4.));
#28332=CARTESIAN_POINT('Ctrl Pts',(-0.0398513841857263,-0.149064942821851,
4.));
#28333=CARTESIAN_POINT('Ctrl Pts',(-0.0894268873061843,-0.13581130730129,
3.99735343997437));
#28334=CARTESIAN_POINT('Ctrl Pts',(-0.144571567721208,-0.0835405737349159,
3.99387971585475));
#28335=CARTESIAN_POINT('Ctrl Pts',(-0.154267320225706,-0.0162511224334367,
3.99040599173513));
#28336=CARTESIAN_POINT('Ctrl Pts',(-0.154145398954164,-0.000183190088064077,
3.98957882764113));
#28337=CARTESIAN_POINT('',(0.0399397509085001,-0.149330346493117,4.));
#28338=CARTESIAN_POINT('Origin',(0.,0.,4.));
#28339=CARTESIAN_POINT('Ctrl Pts',(0.0399398308045223,-0.149330586455588,
4.));
#28340=CARTESIAN_POINT('Ctrl Pts',(-0.00819994193508078,-0.162114963086391,
3.9974200549221));
#28341=CARTESIAN_POINT('Ctrl Pts',(-0.111773735607764,-0.138502981643238,
3.99256044570839));
#28342=CARTESIAN_POINT('Ctrl Pts',(-0.154082201487749,-0.0439653055987776,
3.98770083649468));
#28343=CARTESIAN_POINT('Ctrl Pts',(-0.154443265232512,0.000108744696557906,
3.98542117235887));
#28344=CARTESIAN_POINT('Origin',(-1.70916393953233E-17,-6.81365885416763E-18,
3.5));
#28345=CARTESIAN_POINT('Ctrl Pts',(-0.0958116152722498,0.0825211298936362,
3.5));
#28346=CARTESIAN_POINT('Ctrl Pts',(-0.100695982673166,0.0779597798732974,
3.5));
#28347=CARTESIAN_POINT('Ctrl Pts',(-0.105169094336774,0.073000191113619,
3.5));
#28348=CARTESIAN_POINT('Ctrl Pts',(-0.109227190160158,0.0677117533966587,
3.5));
#28349=CARTESIAN_POINT('Ctrl Pts',(-0.111694873825402,0.0644959122887171,
3.5));
#28350=CARTESIAN_POINT('Ctrl Pts',(-0.114010184214277,0.0611562073506752,
3.5));
#28351=CARTESIAN_POINT('Ctrl Pts',(-0.116166807098829,0.0577125335531249,
3.5));
#28352=CARTESIAN_POINT('Ctrl Pts',(-0.121431726365849,0.0493055632589991,
3.5));
#28353=CARTESIAN_POINT('Ctrl Pts',(-0.12573464769667,0.0403151423737322,
3.5));
#28354=CARTESIAN_POINT('Ctrl Pts',(-0.129045466546674,0.0309386517006337,
3.5));
#28355=CARTESIAN_POINT('Ctrl Pts',(-0.130207164312345,0.0276486353154881,
3.5));
#28356=CARTESIAN_POINT('Ctrl Pts',(-0.131243087485824,0.0243197585947972,
3.5));
#28357=CARTESIAN_POINT('Ctrl Pts',(-0.132152263806834,0.0209620064696601,
3.5));
#28358=CARTESIAN_POINT('Ctrl Pts',(-0.134828933182204,0.0110765837240964,
3.5));
#28359=CARTESIAN_POINT('Ctrl Pts',(-0.136412178238084,0.000939292992310017,
3.5));
#28360=CARTESIAN_POINT('Ctrl Pts',(-0.136856372906323,-0.00925247465139327,
3.5));
#28361=CARTESIAN_POINT('Ctrl Pts',(-0.137021913483504,-0.0130506992112034,
3.5));
#28362=CARTESIAN_POINT('Ctrl Pts',(-0.137028726314264,-0.0168567537781713,
3.5));
#28363=CARTESIAN_POINT('Ctrl Pts',(-0.136872398016052,-0.0206609891299379,
3.5));
#28364=CARTESIAN_POINT('Ctrl Pts',(-0.136740582821431,-0.0238687002674301,
3.5));
#28365=CARTESIAN_POINT('Ctrl Pts',(-0.136493094718847,-0.0270653690856263,
3.5));
#28366=CARTESIAN_POINT('Ctrl Pts',(-0.13612917734588,-0.0302430275614766,
3.5));
#28367=CARTESIAN_POINT('Ctrl Pts',(-0.13576659429471,-0.0334090349888054,
3.5));
#28368=CARTESIAN_POINT('Ctrl Pts',(-0.135288410857674,-0.0365568188154616,
3.5));
#28369=CARTESIAN_POINT('Ctrl Pts',(-0.134693327673148,-0.0396806409761667,
3.5));
#28370=CARTESIAN_POINT('Ctrl Pts',(-0.133341599676801,-0.0467763848654778,
3.5));
#28371=CARTESIAN_POINT('Ctrl Pts',(-0.131387825400402,-0.0537485551880799,
3.5));
#28372=CARTESIAN_POINT('Ctrl Pts',(-0.128888271219693,-0.0605519919600177,
3.5));
#28373=CARTESIAN_POINT('Ctrl Pts',(-0.127520602506107,-0.0642745948504241,
3.5));
#28374=CARTESIAN_POINT('Ctrl Pts',(-0.125989250183059,-0.0679466858359917,
3.5));
#28375=CARTESIAN_POINT('Ctrl Pts',(-0.124301567034569,-0.0715605953668731,
3.5));
#28376=CARTESIAN_POINT('Ctrl Pts',(-0.123083413065749,-0.0741690815877246,
3.5));
#28377=CARTESIAN_POINT('Ctrl Pts',(-0.121784536276434,-0.0767452222753887,
3.5));
#28378=CARTESIAN_POINT('Ctrl Pts',(-0.120412533496435,-0.0792783080753084,
3.5));
#28379=CARTESIAN_POINT('Ctrl Pts',(-0.116240621079353,-0.0869807794232376,
3.5));
#28380=CARTESIAN_POINT('Ctrl Pts',(-0.111384900653015,-0.0943068033536031,
3.5));
#28381=CARTESIAN_POINT('Ctrl Pts',(-0.105936294580107,-0.101180758720708,
3.5));
#28382=CARTESIAN_POINT('Ctrl Pts',(-0.102498213514854,-0.105518237972245,
3.5));
#28383=CARTESIAN_POINT('Ctrl Pts',(-0.0988234872002696,-0.109675688132788,
3.5));
#28384=CARTESIAN_POINT('Ctrl Pts',(-0.0949300211352312,-0.113632240993693,
3.5));
#28385=CARTESIAN_POINT('Ctrl Pts',(-0.0916236146803262,-0.116992221972066,
3.5));
#28386=CARTESIAN_POINT('Ctrl Pts',(-0.0881545091528211,-0.120210812929281,
3.5));
#28387=CARTESIAN_POINT('Ctrl Pts',(-0.0845585132916744,-0.123253141705618,
3.5));
#28388=CARTESIAN_POINT('Ctrl Pts',(-0.0763242263006133,-0.13021961475866,
3.5));
#28389=CARTESIAN_POINT('Ctrl Pts',(-0.0674109291876633,-0.136284624413674,
3.5));
#28390=CARTESIAN_POINT('Ctrl Pts',(-0.0579550193346048,-0.141304740223277,
3.5));
#28391=CARTESIAN_POINT('Ctrl Pts',(-0.0532842084112166,-0.143784460538354,
3.5));
#28392=CARTESIAN_POINT('Ctrl Pts',(-0.0484803425336181,-0.146008805046434,
3.5));
#28393=CARTESIAN_POINT('Ctrl Pts',(-0.0435567265409999,-0.147956912059339,
3.5));
#28394=CARTESIAN_POINT('Ctrl Pts',(-0.042358096554505,-0.148431169086302,
3.5));
#28395=CARTESIAN_POINT('Ctrl Pts',(-0.0411523620931259,-0.148889040418797,
3.5));
#28396=CARTESIAN_POINT('Ctrl Pts',(-0.0399398165374117,-0.14933059314829,
3.5));
#28397=CARTESIAN_POINT('Ctrl Pts',(0.0398513841857336,-0.149064942821849,
3.5));
#28398=CARTESIAN_POINT('Ctrl Pts',(0.0462529496128914,-0.146725837162888,
3.5));
#28399=CARTESIAN_POINT('Ctrl Pts',(0.0524692076951892,-0.14393427563735,
3.5));
#28400=CARTESIAN_POINT('Ctrl Pts',(0.0584702623153416,-0.140728485236784,
3.5));
#28401=CARTESIAN_POINT('Ctrl Pts',(0.0631250229031883,-0.138241891170577,
3.5));
#28402=CARTESIAN_POINT('Ctrl Pts',(0.0676502468975603,-0.1355058910355,
3.5));
#28403=CARTESIAN_POINT('Ctrl Pts',(0.0720296458894365,-0.132535875720451,
3.5));
#28404=CARTESIAN_POINT('Ctrl Pts',(0.0754784967726087,-0.130196938354537,
3.5));
#28405=CARTESIAN_POINT('Ctrl Pts',(0.0788293975632557,-0.127717841671465,
3.5));
#28406=CARTESIAN_POINT('Ctrl Pts',(0.0820734025861846,-0.125108353169529,
3.5));
#28407=CARTESIAN_POINT('Ctrl Pts',(0.0878699486728443,-0.120445592089575,
3.5));
#28408=CARTESIAN_POINT('Ctrl Pts',(0.0933277488655726,-0.115365506062939,
3.5));
#28409=CARTESIAN_POINT('Ctrl Pts',(0.0983983261001443,-0.109911369421357,
3.5));
#28410=CARTESIAN_POINT('Ctrl Pts',(0.100785232866561,-0.107343907167555,
3.5));
#28411=CARTESIAN_POINT('Ctrl Pts',(0.103082837759472,-0.104696811464977,
3.5));
#28412=CARTESIAN_POINT('Ctrl Pts',(0.105281553373082,-0.101981102913922,
3.5));
#28413=CARTESIAN_POINT('Ctrl Pts',(0.111767020079616,-0.0939706820648148,
3.5));
#28414=CARTESIAN_POINT('Ctrl Pts',(0.117410242387804,-0.0853491014404185,
3.5));
#28415=CARTESIAN_POINT('Ctrl Pts',(0.122076804303227,-0.0762334533122014,
3.5));
#28416=CARTESIAN_POINT('Ctrl Pts',(0.124156859535273,-0.0721702796253988,
3.5));
#28417=CARTESIAN_POINT('Ctrl Pts',(0.126042226032514,-0.0680087185900064,
3.5));
#28418=CARTESIAN_POINT('Ctrl Pts',(0.127717516401833,-0.0637585923271345,
3.5));
#28419=CARTESIAN_POINT('Ctrl Pts',(0.128878955464437,-0.0608120806339354,
3.5));
#28420=CARTESIAN_POINT('Ctrl Pts',(0.129938690733468,-0.0578239271836136,
3.5));
#28421=CARTESIAN_POINT('Ctrl Pts',(0.130888204891735,-0.0548097446101512,
3.5));
#28422=CARTESIAN_POINT('Ctrl Pts',(0.132091470075251,-0.0509900428017762,
3.5));
#28423=CARTESIAN_POINT('Ctrl Pts',(0.133119907502104,-0.0471234083998808,
3.5));
#28424=CARTESIAN_POINT('Ctrl Pts',(0.13396498302397,-0.0432168875268929,
3.5));
#28425=CARTESIAN_POINT('Ctrl Pts',(0.135449870731708,-0.03635271423797,
3.5));
#28426=CARTESIAN_POINT('Ctrl Pts',(0.136369320260194,-0.0293652097985063,
3.5));
#28427=CARTESIAN_POINT('Ctrl Pts',(0.136739868479968,-0.022319296125407,
3.5));
#28428=CARTESIAN_POINT('Ctrl Pts',(0.136938614931574,-0.0185401649189451,
3.5));
#28429=CARTESIAN_POINT('Ctrl Pts',(0.13697923643291,-0.0147442545690828,
3.5));
#28430=CARTESIAN_POINT('Ctrl Pts',(0.136862895918197,-0.0109420689853019,
3.5));
#28431=CARTESIAN_POINT('Ctrl Pts',(0.136768618157157,-0.00786092786453014,
3.5));
#28432=CARTESIAN_POINT('Ctrl Pts',(0.136571008887471,-0.00477673741219634,
3.5));
#28433=CARTESIAN_POINT('Ctrl Pts',(0.136272480032331,-0.00170755776859209,
3.5));
#28434=CARTESIAN_POINT('Ctrl Pts',(0.135524862167375,0.00597871273026037,
3.5));
#28435=CARTESIAN_POINT('Ctrl Pts',(0.134145273604047,0.0135925891081728,
3.5));
#28436=CARTESIAN_POINT('Ctrl Pts',(0.132154756111308,0.0210469694652312,
3.5));
#28437=CARTESIAN_POINT('Ctrl Pts',(0.130956639638983,0.0255338508563019,
3.5));
#28438=CARTESIAN_POINT('Ctrl Pts',(0.129536820205507,0.0299628465144204,
3.5));
#28439=CARTESIAN_POINT('Ctrl Pts',(0.127896985354882,0.0343130630344241,
3.5));
#28440=CARTESIAN_POINT('Ctrl Pts',(0.126764260724531,0.0373179981946284,
3.5));
#28441=CARTESIAN_POINT('Ctrl Pts',(0.125525608395292,0.0402872565072415,
3.5));
#28442=CARTESIAN_POINT('Ctrl Pts',(0.124183958141022,0.0432071171955597,
3.5));
#28443=CARTESIAN_POINT('Ctrl Pts',(0.120305951421964,0.0516469019546402,
3.5));
#28444=CARTESIAN_POINT('Ctrl Pts',(0.115595095267004,0.0596252551381628,
3.5));
#28445=CARTESIAN_POINT('Ctrl Pts',(0.110076005567125,0.0669787038662309,
3.5));
#28446=CARTESIAN_POINT('Ctrl Pts',(0.106491490638639,0.0717545905024268,
3.5));
#28447=CARTESIAN_POINT('Ctrl Pts',(0.102565240148127,0.0762663779558996,
3.5));
#28448=CARTESIAN_POINT('Ctrl Pts',(0.0982968917172504,0.0804596491219306,
3.5));
#28449=CARTESIAN_POINT('Ctrl Pts',(0.0975400014439711,0.081203226224454,
3.5));
#28450=CARTESIAN_POINT('Ctrl Pts',(0.0967723418961243,0.0819367632413509,
3.5));
#28451=CARTESIAN_POINT('Ctrl Pts',(0.0959941578858439,0.0826601402795114,
3.5));
#28452=CARTESIAN_POINT('Origin',(0.,0.,4.11042117235887));
#28453=CARTESIAN_POINT('Ctrl Pts',(-0.154443265232512,0.000108744696557909,
3.98542117235887));
#28454=CARTESIAN_POINT('Ctrl Pts',(-0.154501375899708,0.00720215273278324,
3.98505427646906));
#28455=CARTESIAN_POINT('Ctrl Pts',(-0.150833043785448,0.0654047280234095,
3.98204082055362));
#28456=CARTESIAN_POINT('Ctrl Pts',(-0.0768181153328184,0.165435267997838,
3.97638080461255));
#28457=CARTESIAN_POINT('Ctrl Pts',(0.0973408978391562,0.154229954870798,
3.96844112453568));
#28458=CARTESIAN_POINT('Ctrl Pts',(0.182376570303567,0.00184388772387479,
3.9605014444588));
#28459=CARTESIAN_POINT('Ctrl Pts',(0.100432518024861,-0.152245093163996,
3.95256176438192));
#28460=CARTESIAN_POINT('Ctrl Pts',(-0.0734653243360244,-0.166934402953208,
3.94462208430505));
#28461=CARTESIAN_POINT('Ctrl Pts',(-0.150201443282177,-0.0675205906017345,
3.9389085536307));
#28462=CARTESIAN_POINT('Ctrl Pts',(-0.154485318877682,-0.00825665133948968,
3.93584158298197));
#28463=CARTESIAN_POINT('Ctrl Pts',(-0.154414683966261,-0.00012271194023455,
3.93542117235887));
#28464=CARTESIAN_POINT('Ctrl Pts',(-0.154145398954164,-0.000183190088064077,
3.98957882764113));
#28465=CARTESIAN_POINT('Ctrl Pts',(-0.153877225967651,0.0351591693674689,
3.9877594317095));
#28466=CARTESIAN_POINT('Ctrl Pts',(-0.124353035696744,0.122445639808398,
3.98329347575225));
#28467=CARTESIAN_POINT('Ctrl Pts',(0.0205691872966891,0.181176549232701,
3.97618095976937));
#28468=CARTESIAN_POINT('Ctrl Pts',(0.16339053139201,0.0810339956098913,
3.9682412796925));
#28469=CARTESIAN_POINT('Ctrl Pts',(0.156677599794682,-0.0933915431448235,
3.96030159961562));
#28470=CARTESIAN_POINT('Ctrl Pts',(0.00648228676056323,-0.182263829019595,
3.95236191953875));
#28471=CARTESIAN_POINT('Ctrl Pts',(-0.129338242603737,-0.114419911622588,
3.94545432888058));
#28472=CARTESIAN_POINT('Ctrl Pts',(-0.153936458995158,-0.0313143964796836,
3.94119329824804));
#28473=CARTESIAN_POINT('Ctrl Pts',(-0.154097159264761,8.62650376686723E-5,
3.93957882764113));
#28474=CARTESIAN_POINT('Ctrl Pts',(0.095811615272233,0.0825211298936557,
4.));
#28475=CARTESIAN_POINT('Ctrl Pts',(0.123256207240687,0.0506564342651108,
3.99735343997437));
#28476=CARTESIAN_POINT('Ctrl Pts',(0.143368215702842,-0.042067892211591,
3.99206031992312));
#28477=CARTESIAN_POINT('Ctrl Pts',(0.0422170408642446,-0.143478264550263,
3.98412063984626));
#28478=CARTESIAN_POINT('Ctrl Pts',(-0.0975844110283061,-0.113165467831369,
3.97618095976937));
#28479=CARTESIAN_POINT('Ctrl Pts',(-0.148038914743343,0.0205825766583269,
3.9682412796925));
#28480=CARTESIAN_POINT('Ctrl Pts',(-0.0629530180417037,0.135575435115532,
3.96030159961561));
#28481=CARTESIAN_POINT('Ctrl Pts',(0.0797715912622248,0.126392597494572,
3.95236191953875));
#28482=CARTESIAN_POINT('Ctrl Pts',(0.149458958618833,0.00151107973223563,
3.94442223946186));
#28483=CARTESIAN_POINT('Ctrl Pts',(0.0823051970462972,-0.124765988532646,
3.936482559385));
#28484=CARTESIAN_POINT('Ctrl Pts',(-0.0602053808314341,-0.136803987384531,
3.92854287930812));
#28485=CARTESIAN_POINT('Ctrl Pts',(-0.147593255628917,-0.0235905240738923,
3.92060319923124));
#28486=CARTESIAN_POINT('Ctrl Pts',(-0.0998481138804565,0.11122350451698,
3.91266351915437));
#28487=CARTESIAN_POINT('Ctrl Pts',(0.0393156975431816,0.144202992379161,
3.90472383907749));
#28488=CARTESIAN_POINT('Ctrl Pts',(0.142482946738445,0.0451539231751995,
3.89678415900061));
#28489=CARTESIAN_POINT('Ctrl Pts',(0.115196050889548,-0.0952372689088321,
3.88884447892374));
#28490=CARTESIAN_POINT('Ctrl Pts',(-0.0175617311292369,-0.148431271407445,
3.88090479884687));
#28491=CARTESIAN_POINT('Ctrl Pts',(-0.134240390927499,-0.0657250333201687,
3.87296511876998));
#28492=CARTESIAN_POINT('Ctrl Pts',(-0.128011600896121,0.0771575802637476,
3.86502543869311));
#28493=CARTESIAN_POINT('Ctrl Pts',(-0.00457829922889965,0.149396452528493,
3.85708575861623));
#28494=CARTESIAN_POINT('Ctrl Pts',(0.123046789066594,0.0848513369547663,
3.84914607853936));
#28495=CARTESIAN_POINT('Ctrl Pts',(0.138013034715666,-0.0573817376169498,
3.84120639846248));
#28496=CARTESIAN_POINT('Ctrl Pts',(0.0266176834030549,-0.147077395754537,
3.83326671838561));
#28497=CARTESIAN_POINT('Ctrl Pts',(-0.109148213688832,-0.102112335081275,
3.82532703830873));
#28498=CARTESIAN_POINT('Ctrl Pts',(-0.144980487747744,0.0363444586596486,
3.81738735823185));
#28499=CARTESIAN_POINT('Ctrl Pts',(-0.0480719232633252,0.141525092050256,
3.80944767815498));
#28500=CARTESIAN_POINT('Ctrl Pts',(0.0928502012748058,0.117128568782365,
3.8015079980781));
#28501=CARTESIAN_POINT('Ctrl Pts',(0.148760792417501,-0.0145082092888036,
3.79356831800123));
#28502=CARTESIAN_POINT('Ctrl Pts',(0.0684693840059589,-0.13286160073391,
3.78562863792435));
#28503=CARTESIAN_POINT('Ctrl Pts',(-0.0745110357927053,-0.129569931090983,
3.77768895784747));
#28504=CARTESIAN_POINT('Ctrl Pts',(-0.149270845181396,-0.00764697822290441,
3.7697492777706));
#28505=CARTESIAN_POINT('Ctrl Pts',(-0.0873616623012301,0.121277374051889,
3.76180959769372));
#28506=CARTESIAN_POINT('Ctrl Pts',(0.0545338724692569,0.139162919812538,
3.75386991761685));
#28507=CARTESIAN_POINT('Ctrl Pts',(0.146499433400264,0.0296340599732921,
3.74593023753997));
#28508=CARTESIAN_POINT('Ctrl Pts',(0.104333443683106,-0.107027071464762,
3.7379905574631));
#28509=CARTESIAN_POINT('Ctrl Pts',(-0.0333578751151315,-0.14569664946404,
3.73005087738622));
#28510=CARTESIAN_POINT('Ctrl Pts',(-0.14050748182764,-0.0509696875349592,
3.72211119730934));
#28511=CARTESIAN_POINT('Ctrl Pts',(-0.119011632529845,0.0904239615350441,
3.71417151723247));
#28512=CARTESIAN_POINT('Ctrl Pts',(0.0114485618600744,0.149027487159785,
3.70623183715559));
#28513=CARTESIAN_POINT('Ctrl Pts',(0.131426713281372,0.0711848335798314,
3.69829215707872));
#28514=CARTESIAN_POINT('Ctrl Pts',(0.131073553936911,-0.0718330352678932,
3.69035247700184));
#28515=CARTESIAN_POINT('Ctrl Pts',(0.0107124284623447,-0.149082210133256,
3.68241279692496));
#28516=CARTESIAN_POINT('Ctrl Pts',(-0.119456752931603,-0.0898351026331364,
3.67447311684809));
#28517=CARTESIAN_POINT('Ctrl Pts',(-0.140254047194737,0.0516629823793918,
3.66653343677121));
#28518=CARTESIAN_POINT('Ctrl Pts',(-0.0326379242804108,0.145859615472823,
3.65859375669434));
#28519=CARTESIAN_POINT('Ctrl Pts',(0.10486073980172,0.10651050023316,3.65065407661746));
#28520=CARTESIAN_POINT('Ctrl Pts',(0.146351295051501,-0.0303572067245441,
3.64271439654059));
#28521=CARTESIAN_POINT('Ctrl Pts',(0.0538459306115186,-0.139430547008859,
3.63477471646371));
#28522=CARTESIAN_POINT('Ctrl Pts',(-0.0879595415059408,-0.12084444509365,
3.62683503638684));
#28523=CARTESIAN_POINT('Ctrl Pts',(-0.149231261493045,0.00838407713103302,
3.61889535630996));
#28524=CARTESIAN_POINT('Ctrl Pts',(-0.0738702226095378,0.12993634123263,
3.61095567623308));
#28525=CARTESIAN_POINT('Ctrl Pts',(0.0691246960538845,0.132521821325185,
3.60301599615621));
#28526=CARTESIAN_POINT('Ctrl Pts',(0.148830647021129,0.0137733814668988,
3.59507631607933));
#28527=CARTESIAN_POINT('Ctrl Pts',(0.0922705776859184,-0.11758574481156,
3.58713663600245));
#28528=CARTESIAN_POINT('Ctrl Pts',(-0.0487702109612334,-0.141285857774966,
3.57919695592558));
#28529=CARTESIAN_POINT('Ctrl Pts',(-0.145158345123895,-0.0356282001147357,
3.5712572758487));
#28530=CARTESIAN_POINT('Ctrl Pts',(-0.108642326262961,0.10265050841275,
3.56331759577183));
#28531=CARTESIAN_POINT('Ctrl Pts',(0.0273432144577738,0.14694341587319,
3.55537791569495));
#28532=CARTESIAN_POINT('Ctrl Pts',(0.138295730077318,0.0567008676982971,
3.54743823561807));
#28533=CARTESIAN_POINT('Ctrl Pts',(0.122624304118183,-0.0854607729482632,
3.5394985555412));
#28534=CARTESIAN_POINT('Ctrl Pts',(-0.00531228376040394,-0.149366579646122,
3.53155887546432));
#28535=CARTESIAN_POINT('Ctrl Pts',(-0.128398465432132,-0.0765350583850204,
3.52361919538745));
#28536=CARTESIAN_POINT('Ctrl Pts',(-0.133899765542225,0.0664079477775043,
3.51567951531057));
#28537=CARTESIAN_POINT('Ctrl Pts',(-0.0168566046022346,0.148475571278638,
3.5077398352337));
#28538=CARTESIAN_POINT('Ctrl Pts',(0.115720245650148,0.0947476421044766,
3.49980015515682));
#28539=CARTESIAN_POINT('Ctrl Pts',(0.142146925240749,-0.0460261281615502,
3.49186047507995));
#28540=CARTESIAN_POINT('Ctrl Pts',(0.0732860006472317,-0.111298378536925,
3.48656735502869));
#28541=CARTESIAN_POINT('Ctrl Pts',(0.0326585063531174,-0.122159831625553,
3.48392079500307));
#28542=CARTESIAN_POINT('Ctrl Pts',(0.102845629995659,0.0885794229410745,
4.00535973499898));
#28543=CARTESIAN_POINT('Ctrl Pts',(0.132305068112318,0.0543753790239966,
4.00271317497335));
#28544=CARTESIAN_POINT('Ctrl Pts',(0.153893600722808,-0.0451563087084747,
3.9974200549221));
#28545=CARTESIAN_POINT('Ctrl Pts',(0.0453164071172279,-0.154011728812092,
3.98948037484522));
#28546=CARTESIAN_POINT('Ctrl Pts',(-0.104748575644461,-0.121473516543913,
3.98154069476835));
#28547=CARTESIAN_POINT('Ctrl Pts',(-0.158907199376537,0.0220936475952833,
3.97360101469147));
#28548=CARTESIAN_POINT('Ctrl Pts',(-0.067574717138742,0.145528712742967,
3.9656613346146));
#28549=CARTESIAN_POINT('Ctrl Pts',(0.0856280267878686,0.135671716619981,
3.95772165453772));
#28550=CARTESIAN_POINT('Ctrl Pts',(0.160431495847078,0.00162201572944855,
3.94978197446085));
#28551=CARTESIAN_POINT('Ctrl Pts',(0.0883476373724852,-0.133925690076429,
3.94184229438397));
#28552=CARTESIAN_POINT('Ctrl Pts',(-0.0646253619996309,-0.146847459240757,
3.93390261430709));
#28553=CARTESIAN_POINT('Ctrl Pts',(-0.158428822175023,-0.0253224236269645,
3.92596293423022));
#28554=CARTESIAN_POINT('Ctrl Pts',(-0.107178468359357,0.119388983891694,
3.91802325415334));
#28555=CARTESIAN_POINT('Ctrl Pts',(0.0422020615251973,0.15478966257228,
3.91008357407647));
#28556=CARTESIAN_POINT('Ctrl Pts',(0.152943339691301,0.0484689007959436,
3.90214389399959));
#28557=CARTESIAN_POINT('Ctrl Pts',(0.123653174963026,-0.102229117964087,
3.89420421392272));
#28558=CARTESIAN_POINT('Ctrl Pts',(-0.0188510265344017,-0.159328360925561,
3.88626453384584));
#28559=CARTESIAN_POINT('Ctrl Pts',(-0.144095656216364,-0.0705502400631941,
3.87832485376896));
#28560=CARTESIAN_POINT('Ctrl Pts',(-0.137409579240545,0.0828221080358456,
3.87038517369209));
#28561=CARTESIAN_POINT('Ctrl Pts',(-0.00491441530514796,0.160364400868861,
3.86244549361521));
#28562=CARTESIAN_POINT('Ctrl Pts',(0.13208027549207,0.0910807022748934,
3.85450581353834));
#28563=CARTESIAN_POINT('Ctrl Pts',(0.148145268844653,-0.0615944208715485,
3.84656613346146));
#28564=CARTESIAN_POINT('Ctrl Pts',(0.0285718220158795,-0.157875090421108,
3.83862645338458));
#28565=CARTESIAN_POINT('Ctrl Pts',(-0.117161335479353,-0.109608917477515,
3.83068677330771));
#28566=CARTESIAN_POINT('Ctrl Pts',(-0.155624237803826,0.0390126889843388,
3.82274709323083));
#28567=CARTESIAN_POINT('Ctrl Pts',(-0.0516011260124583,0.151915164051309,
3.81480741315396));
#28568=CARTESIAN_POINT('Ctrl Pts',(0.0996668036354316,0.125727568757556,
3.80686773307708));
#28569=CARTESIAN_POINT('Ctrl Pts',(0.159682073737726,-0.0155733302290782,
3.7989280530002));
#28570=CARTESIAN_POINT('Ctrl Pts',(0.0734960673974602,-0.142615642068929,
3.79098837292333));
#28571=CARTESIAN_POINT('Ctrl Pts',(-0.0799812673646754,-0.139082314327793,
3.78304869284645));
#28572=CARTESIAN_POINT('Ctrl Pts',(-0.160229572051837,-0.00820838152726148,
3.77510901276958));
#28573=CARTESIAN_POINT('Ctrl Pts',(-0.0937753232873622,0.13018095878194,
3.7671693326927));
#28574=CARTESIAN_POINT('Ctrl Pts',(0.0585374795557702,0.149379572815778,
3.75922965261583));
#28575=CARTESIAN_POINT('Ctrl Pts',(0.157254696930506,0.0318096460290618,
3.75128997253895));
#28576=CARTESIAN_POINT('Ctrl Pts',(0.111993088882986,-0.11488446948847,
3.74335029246207));
#28577=CARTESIAN_POINT('Ctrl Pts',(-0.0358068452534112,-0.156392976569809,
3.7354106123852));
#28578=CARTESIAN_POINT('Ctrl Pts',(-0.15082284592122,-0.0547116297989597,
3.72747093230832));
#28579=CARTESIAN_POINT('Ctrl Pts',(-0.127748877728095,0.0970624413788584,
3.71953125223145));
#28580=CARTESIAN_POINT('Ctrl Pts',(0.0122890586250752,0.1599683478884,3.71159157215457));
#28581=CARTESIAN_POINT('Ctrl Pts',(0.141075412279359,0.0764108718431722,
3.7036518920777));
#28582=CARTESIAN_POINT('Ctrl Pts',(0.140696325723237,-0.0771066612919101,
3.69571221200082));
#28583=CARTESIAN_POINT('Ctrl Pts',(0.0114988819556263,-0.160027088351817,
3.68777253192394));
#28584=CARTESIAN_POINT('Ctrl Pts',(-0.128226676667323,-0.0964303513700096,
3.67983285184707));
#28585=CARTESIAN_POINT('Ctrl Pts',(-0.150550805371548,0.0554558229204912,
3.67189317177019));
#28586=CARTESIAN_POINT('Ctrl Pts',(-0.035034039190677,0.156567906736611,
3.66395349169332));
#28587=CARTESIAN_POINT('Ctrl Pts',(0.112559096473601,0.114329974153006,
3.65601381161644));
#28588=CARTESIAN_POINT('Ctrl Pts',(0.157095682997156,-0.0325858826367059,
3.64807413153956));
#28589=CARTESIAN_POINT('Ctrl Pts',(0.0577990324107298,-0.14966684787665,
3.64013445146269));
#28590=CARTESIAN_POINT('Ctrl Pts',(-0.0944170958250141,-0.129716246321693,
3.63219477138581));
#28591=CARTESIAN_POINT('Ctrl Pts',(-0.160187082324945,0.00899959459010582,
3.62425509130894));
#28592=CARTESIAN_POINT('Ctrl Pts',(-0.0792934088483033,0.139475624489065,
3.61631541123206));
#28593=CARTESIAN_POINT('Ctrl Pts',(0.0741994892135014,0.142250917737222,
3.60837573115519));
#28594=CARTESIAN_POINT('Ctrl Pts',(0.159757056720716,0.0147845549843712,
3.60043605107831));
#28595=CARTESIAN_POINT('Ctrl Pts',(0.099044626950589,-0.126218308388737,
3.59249637100143));
#28596=CARTESIAN_POINT('Ctrl Pts',(-0.0523506785380631,-0.151658366379244,
3.58455669092456));
#28597=CARTESIAN_POINT('Ctrl Pts',(-0.155815152588506,-0.0382438462810607,
3.57661701084768));
#28598=CARTESIAN_POINT('Ctrl Pts',(-0.116618308301774,0.110186600832138,
3.5686773307708));
#28599=CARTESIAN_POINT('Ctrl Pts',(0.0293506179707539,0.157731274399797,
3.56073765069393));
#28600=CARTESIAN_POINT('Ctrl Pts',(0.148448718300998,0.06086356485237,3.55279797061705));
#28601=CARTESIAN_POINT('Ctrl Pts',(0.131626773789177,-0.0917348800435817,
3.54485829054018));
#28602=CARTESIAN_POINT('Ctrl Pts',(-0.00570228534924597,-0.160332334867275,
3.5369186104633));
#28603=CARTESIAN_POINT('Ctrl Pts',(-0.137824845456608,-0.0821538836809814,
3.52897893038643));
#28604=CARTESIAN_POINT('Ctrl Pts',(-0.143730023800696,0.0712832907209694,
3.52103925030955));
#28605=CARTESIAN_POINT('Ctrl Pts',(-0.0180941331067087,0.159375913074104,
3.51309957023267));
#28606=CARTESIAN_POINT('Ctrl Pts',(0.124215853509266,0.101703545182399,
3.5051598901558));
#28607=CARTESIAN_POINT('Ctrl Pts',(0.152582649157857,-0.0494051387567767,
3.49722021007893));
#28608=CARTESIAN_POINT('Ctrl Pts',(0.0786662962002181,-0.119469354791712,
3.49192709002767));
#28609=CARTESIAN_POINT('Ctrl Pts',(0.0350561322973228,-0.131128202024318,
3.48928053000205));
#28610=CARTESIAN_POINT('Ctrl Pts',(0.109879644719085,0.0946377159884933,
4.01071946999795));
#28611=CARTESIAN_POINT('Ctrl Pts',(0.141353928983949,0.0580943237828825,
4.00807290997233));
#28612=CARTESIAN_POINT('Ctrl Pts',(0.164418985742774,-0.0482447252053583,
4.00277978992107));
#28613=CARTESIAN_POINT('Ctrl Pts',(0.0484157733702112,-0.164545193073921,
3.99484010984421));
#28614=CARTESIAN_POINT('Ctrl Pts',(-0.111912740260616,-0.129781565256457,
3.98690042976732));
#28615=CARTESIAN_POINT('Ctrl Pts',(-0.16977548400973,0.0236047185322397,
3.97896074969046));
#28616=CARTESIAN_POINT('Ctrl Pts',(-0.0721964162357802,0.155481990370402,
3.97102106961357));
#28617=CARTESIAN_POINT('Ctrl Pts',(0.0914844623135124,0.14495083574539,
3.9630813895367));
#28618=CARTESIAN_POINT('Ctrl Pts',(0.171404033075322,0.0017329517266617,
3.95514170945982));
#28619=CARTESIAN_POINT('Ctrl Pts',(0.0943900776986731,-0.143085391620212,
3.94720202938295));
#28620=CARTESIAN_POINT('Ctrl Pts',(-0.0690453431678277,-0.156890931096983,
3.93926234930607));
#28621=CARTESIAN_POINT('Ctrl Pts',(-0.169264388721129,-0.0270543231800365,
3.9313226692292));
#28622=CARTESIAN_POINT('Ctrl Pts',(-0.114508822838256,0.127554463266409,
3.92338298915232));
#28623=CARTESIAN_POINT('Ctrl Pts',(0.0450884255072127,0.165376332765398,
3.91544330907545));
#28624=CARTESIAN_POINT('Ctrl Pts',(0.163403732644156,0.0517838784166879,
3.90750362899857));
#28625=CARTESIAN_POINT('Ctrl Pts',(0.132110299036504,-0.109220967019342,
3.89956394892169));
#28626=CARTESIAN_POINT('Ctrl Pts',(-0.0201403219395664,-0.170225450443677,
3.89162426884482));
#28627=CARTESIAN_POINT('Ctrl Pts',(-0.153950921505229,-0.0753754468062197,
3.88368458876794));
#28628=CARTESIAN_POINT('Ctrl Pts',(-0.146807557584968,0.0884866358079437,
3.87574490869107));
#28629=CARTESIAN_POINT('Ctrl Pts',(-0.00525053138139654,0.171332349209229,
3.86780522861419));
#28630=CARTESIAN_POINT('Ctrl Pts',(0.141113761917547,0.0973100675950205,
3.85986554853731));
#28631=CARTESIAN_POINT('Ctrl Pts',(0.15827750297364,-0.0658071041261473,
3.85192586846044));
#28632=CARTESIAN_POINT('Ctrl Pts',(0.0305259606287044,-0.16867278508768,
3.84398618838356));
#28633=CARTESIAN_POINT('Ctrl Pts',(-0.125174457269873,-0.117105499873754,
3.83604650830669));
#28634=CARTESIAN_POINT('Ctrl Pts',(-0.166267987859908,0.0416809193090289,
3.82810682822981));
#28635=CARTESIAN_POINT('Ctrl Pts',(-0.0551303287615912,0.162305236052362,
3.82016714815293));
#28636=CARTESIAN_POINT('Ctrl Pts',(0.106483405996057,0.134326568732747,
3.81222746807606));
#28637=CARTESIAN_POINT('Ctrl Pts',(0.170603355057952,-0.0166384511693528,
3.80428778799918));
#28638=CARTESIAN_POINT('Ctrl Pts',(0.0785227507889612,-0.152369683403947,
3.79634810792231));
#28639=CARTESIAN_POINT('Ctrl Pts',(-0.0854514989366454,-0.148594697564603,
3.78840842784543));
#28640=CARTESIAN_POINT('Ctrl Pts',(-0.171188298922279,-0.00876978483161878,
3.78046874776855));
#28641=CARTESIAN_POINT('Ctrl Pts',(-0.100188984273494,0.139084543511992,
3.77252906769168));
#28642=CARTESIAN_POINT('Ctrl Pts',(0.0625410866422834,0.159596225819019,
3.7645893876148));
#28643=CARTESIAN_POINT('Ctrl Pts',(0.168009960460748,0.0339852320848313,
3.75664970753793));
#28644=CARTESIAN_POINT('Ctrl Pts',(0.119652734082865,-0.122741867512178,
3.74871002746105));
#28645=CARTESIAN_POINT('Ctrl Pts',(-0.0382558153916907,-0.167089303675579,
3.74077034738417));
#28646=CARTESIAN_POINT('Ctrl Pts',(-0.161138210014801,-0.0584535720629604,
3.7328306673073));
#28647=CARTESIAN_POINT('Ctrl Pts',(-0.136486122926345,0.103700921222673,
3.72489098723042));
#28648=CARTESIAN_POINT('Ctrl Pts',(0.0131295553900761,0.170909208617015,
3.71695130715355));
#28649=CARTESIAN_POINT('Ctrl Pts',(0.150724111277345,0.081636910106513,
3.70901162707667));
#28650=CARTESIAN_POINT('Ctrl Pts',(0.150319097509564,-0.0823802873159272,
3.7010719469998));
#28651=CARTESIAN_POINT('Ctrl Pts',(0.0122853354489075,-0.170971966570378,
3.69313226692292));
#28652=CARTESIAN_POINT('Ctrl Pts',(-0.136996600403042,-0.103025600106883,
3.68519258684605));
#28653=CARTESIAN_POINT('Ctrl Pts',(-0.16084756354836,0.0592486634615907,
3.67725290676916));
#28654=CARTESIAN_POINT('Ctrl Pts',(-0.037430154100943,0.1672761980004,3.66931322669229));
#28655=CARTESIAN_POINT('Ctrl Pts',(0.120257453145481,0.122149448072851,
3.66137354661541));
#28656=CARTESIAN_POINT('Ctrl Pts',(0.167840070942811,-0.0348145585488677,
3.65343386653854));
#28657=CARTESIAN_POINT('Ctrl Pts',(0.0617521342099411,-0.159903148744442,
3.64549418646166));
#28658=CARTESIAN_POINT('Ctrl Pts',(-0.100874650144087,-0.138588047549736,
3.63755450638479));
#28659=CARTESIAN_POINT('Ctrl Pts',(-0.171142903156845,0.00961511204917869,
3.62961482630791));
#28660=CARTESIAN_POINT('Ctrl Pts',(-0.0847165950870686,0.149014907745501,
3.62167514623104));
#28661=CARTESIAN_POINT('Ctrl Pts',(0.0792742823731183,0.15198001414926,
3.61373546615416));
#28662=CARTESIAN_POINT('Ctrl Pts',(0.170683466420304,0.0157957285018435,
3.60579578607728));
#28663=CARTESIAN_POINT('Ctrl Pts',(0.10581867621526,-0.134850871965913,
3.59785610600041));
#28664=CARTESIAN_POINT('Ctrl Pts',(-0.0559311461148929,-0.162030874983522,
3.58991642592353));
#28665=CARTESIAN_POINT('Ctrl Pts',(-0.166471960053118,-0.0408594924473857,
3.58197674584666));
#28666=CARTESIAN_POINT('Ctrl Pts',(-0.124594290340586,0.117722693251527,
3.57403706576978));
#28667=CARTESIAN_POINT('Ctrl Pts',(0.0313580214837342,0.168519132926404,
3.56609738569291));
#28668=CARTESIAN_POINT('Ctrl Pts',(0.158601706524679,0.065026262006443,
3.55815770561603));
#28669=CARTESIAN_POINT('Ctrl Pts',(0.14062924346017,-0.0980089871389004,
3.55021802553916));
#28670=CARTESIAN_POINT('Ctrl Pts',(-0.00609228693808808,-0.171298090088428,
3.54227834546228));
#28671=CARTESIAN_POINT('Ctrl Pts',(-0.147251225481083,-0.0877727089769424,
3.5343386653854));
#28672=CARTESIAN_POINT('Ctrl Pts',(-0.153560282059167,0.0761586336644345,
3.52639898530853));
#28673=CARTESIAN_POINT('Ctrl Pts',(-0.0193316616111828,0.17027625486957,
3.51845930523165));
#28674=CARTESIAN_POINT('Ctrl Pts',(0.132711461368385,0.10865944826032,3.51051962515478));
#28675=CARTESIAN_POINT('Ctrl Pts',(0.163018373074965,-0.0527841493520032,
3.5025799450779));
#28676=CARTESIAN_POINT('Ctrl Pts',(0.0840465917532045,-0.127640331046499,
3.49728682502665));
#28677=CARTESIAN_POINT('Ctrl Pts',(0.0374537582415282,-0.140096572423083,
3.49464026500102));
#28678=CARTESIAN_POINT('Ctrl Pts',(0.116913659442511,0.100696009035912,
4.01607920499693));
#28679=CARTESIAN_POINT('Ctrl Pts',(0.15040278985558,0.0618132685417683,
4.01343264497131));
#28680=CARTESIAN_POINT('Ctrl Pts',(0.17494437076274,-0.0513331417022419,
4.00813952492005));
#28681=CARTESIAN_POINT('Ctrl Pts',(0.0515151396231945,-0.17507865733575,
4.00019984484318));
#28682=CARTESIAN_POINT('Ctrl Pts',(-0.119076904876771,-0.138089613969001,
3.9922601647663));
#28683=CARTESIAN_POINT('Ctrl Pts',(-0.180643768642924,0.0251157894691961,
3.98432048468943));
#28684=CARTESIAN_POINT('Ctrl Pts',(-0.0768181153328184,0.165435267997838,
3.97638080461255));
#28685=CARTESIAN_POINT('Ctrl Pts',(0.0973408978391562,0.154229954870798,
3.96844112453568));
#28686=CARTESIAN_POINT('Ctrl Pts',(0.182376570303567,0.00184388772387479,
3.9605014444588));
#28687=CARTESIAN_POINT('Ctrl Pts',(0.100432518024861,-0.152245093163996,
3.95256176438192));
#28688=CARTESIAN_POINT('Ctrl Pts',(-0.0734653243360244,-0.166934402953208,
3.94462208430505));
#28689=CARTESIAN_POINT('Ctrl Pts',(-0.180099955267235,-0.0287862227331087,
3.93668240422817));
#28690=CARTESIAN_POINT('Ctrl Pts',(-0.121839177317157,0.135719942641123,
3.9287427241513));
#28691=CARTESIAN_POINT('Ctrl Pts',(0.0479747894892283,0.175963002958517,
3.92080304407442));
#28692=CARTESIAN_POINT('Ctrl Pts',(0.173864125597012,0.0550988560374321,
3.91286336399754));
#28693=CARTESIAN_POINT('Ctrl Pts',(0.140567423109983,-0.116212816074597,
3.90492368392067));
#28694=CARTESIAN_POINT('Ctrl Pts',(-0.0214296173447312,-0.181122539961793,
3.89698400384379));
#28695=CARTESIAN_POINT('Ctrl Pts',(-0.163806186794094,-0.0802006535492451,
3.88904432376692));
#28696=CARTESIAN_POINT('Ctrl Pts',(-0.156205535929391,0.0941511635800416,
3.88110464369004));
#28697=CARTESIAN_POINT('Ctrl Pts',(-0.005586647457645,0.182300297549597,
3.87316496361317));
#28698=CARTESIAN_POINT('Ctrl Pts',(0.150147248343024,0.103539432915148,
3.86522528353629));
#28699=CARTESIAN_POINT('Ctrl Pts',(0.168409737102627,-0.0700197873807462,
3.85728560345941));
#28700=CARTESIAN_POINT('Ctrl Pts',(0.0324800992415292,-0.179470479754251,
3.84934592338254));
#28701=CARTESIAN_POINT('Ctrl Pts',(-0.133187579060394,-0.124602082269994,
3.84140624330566));
#28702=CARTESIAN_POINT('Ctrl Pts',(-0.17691173791599,0.0443491496337192,
3.83346656322879));
#28703=CARTESIAN_POINT('Ctrl Pts',(-0.0586595315107243,0.172695308053416,
3.82552688315191));
#28704=CARTESIAN_POINT('Ctrl Pts',(0.113300008356683,0.142925568707939,
3.81758720307504));
#28705=CARTESIAN_POINT('Ctrl Pts',(0.181524636378177,-0.0177035721096275,
3.80964752299816));
#28706=CARTESIAN_POINT('Ctrl Pts',(0.0835494341804624,-0.162123724738966,
3.80170784292129));
#28707=CARTESIAN_POINT('Ctrl Pts',(-0.0909217305086156,-0.158107080801413,
3.7937681628444));
#28708=CARTESIAN_POINT('Ctrl Pts',(-0.18214702579272,-0.00933118813597588,
3.78582848276753));
#28709=CARTESIAN_POINT('Ctrl Pts',(-0.106602645259627,0.147988128242044,
3.77788880269065));
#28710=CARTESIAN_POINT('Ctrl Pts',(0.0665446937287967,0.169812878822259,
3.76994912261378));
#28711=CARTESIAN_POINT('Ctrl Pts',(0.178765223990991,0.0361608181406009,
3.7620094425369));
#28712=CARTESIAN_POINT('Ctrl Pts',(0.127312379282745,-0.130599265535886,
3.75406976246003));
#28713=CARTESIAN_POINT('Ctrl Pts',(-0.0407047855299705,-0.177785630781348,
3.74613008238315));
#28714=CARTESIAN_POINT('Ctrl Pts',(-0.171453574108382,-0.0621955143269609,
3.73819040230628));
#28715=CARTESIAN_POINT('Ctrl Pts',(-0.145223368124595,0.110339401066487,
3.7302507222294));
#28716=CARTESIAN_POINT('Ctrl Pts',(0.0139700521550768,0.18185006934563,
3.72231104215253));
#28717=CARTESIAN_POINT('Ctrl Pts',(0.160372810275332,0.0868629483698537,
3.71437136207565));
#28718=CARTESIAN_POINT('Ctrl Pts',(0.15994186929589,-0.087653913339944,
3.70643168199877));
#28719=CARTESIAN_POINT('Ctrl Pts',(0.013071788942189,-0.181916844788939,
3.6984920019219));
#28720=CARTESIAN_POINT('Ctrl Pts',(-0.145766524138762,-0.109620848843756,
3.69055232184502));
#28721=CARTESIAN_POINT('Ctrl Pts',(-0.171144321725171,0.06304150400269,
3.68261264176815));
#28722=CARTESIAN_POINT('Ctrl Pts',(-0.039826269011209,0.177984489264188,
3.67467296169127));
#28723=CARTESIAN_POINT('Ctrl Pts',(0.127955809817362,0.129968921992697,
3.66673328161439));
#28724=CARTESIAN_POINT('Ctrl Pts',(0.178584458888466,-0.0370432344610292,
3.65879360153752));
#28725=CARTESIAN_POINT('Ctrl Pts',(0.0657052360091523,-0.170139449612234,
3.65085392146064));
#28726=CARTESIAN_POINT('Ctrl Pts',(-0.107332204463161,-0.147459848777779,
3.64291424138377));
#28727=CARTESIAN_POINT('Ctrl Pts',(-0.182098723988745,0.0102306295082514,
3.63497456130689));
#28728=CARTESIAN_POINT('Ctrl Pts',(-0.0901397813258339,0.158554191001936,
3.62703488123002));
#28729=CARTESIAN_POINT('Ctrl Pts',(0.0843490755327352,0.161709110561297,
3.61909520115314));
#28730=CARTESIAN_POINT('Ctrl Pts',(0.181609876119891,0.0168069020193158,
3.61115552107626));
#28731=CARTESIAN_POINT('Ctrl Pts',(0.11259272547993,-0.14348343554309,3.60321584099938));
#28732=CARTESIAN_POINT('Ctrl Pts',(-0.0595116136917225,-0.1724033835878,
3.59527616092251));
#28733=CARTESIAN_POINT('Ctrl Pts',(-0.17712876751773,-0.0434751386137106,
3.58733648084563));
#28734=CARTESIAN_POINT('Ctrl Pts',(-0.132570272379398,0.125258785670915,
3.57939680076876));
#28735=CARTESIAN_POINT('Ctrl Pts',(0.0333654249967142,0.179306991453011,
3.57145712069188));
#28736=CARTESIAN_POINT('Ctrl Pts',(0.16875469474836,0.0691889591605158,
3.56351744061501));
#28737=CARTESIAN_POINT('Ctrl Pts',(0.149631713131164,-0.104283094234219,
3.55557776053813));
#28738=CARTESIAN_POINT('Ctrl Pts',(-0.00648228852693025,-0.182263845309582,
3.54763808046125));
#28739=CARTESIAN_POINT('Ctrl Pts',(-0.156677605505559,-0.0933915342729034,
3.53969840038438));
#28740=CARTESIAN_POINT('Ctrl Pts',(-0.163390540317638,0.0810339766078996,
3.5317587203075));
#28741=CARTESIAN_POINT('Ctrl Pts',(-0.0205691901156568,0.181176596665036,
3.52381904023063));
#28742=CARTESIAN_POINT('Ctrl Pts',(0.141207069227503,0.115615351338242,
3.51587936015375));
#28743=CARTESIAN_POINT('Ctrl Pts',(0.173454096992073,-0.0561631599472297,
3.50793968007688));
#28744=CARTESIAN_POINT('Ctrl Pts',(0.089426887306191,-0.135811307301286,
3.50264656002563));
#28745=CARTESIAN_POINT('Ctrl Pts',(0.0398513841857336,-0.149064942821849,
3.5));
#28746=CARTESIAN_POINT('Ctrl Pts',(0.095811615272233,0.0825211298936557,
4.));
#28747=CARTESIAN_POINT('Ctrl Pts',(0.102493030557671,0.0762815759767258,
4.));
#28748=CARTESIAN_POINT('Ctrl Pts',(0.10839405706188,0.0693097484661253,
4.));
#28749=CARTESIAN_POINT('Ctrl Pts',(0.11350885289652,0.0617853075148104,
4.));
#28750=CARTESIAN_POINT('Ctrl Pts',(0.117424080053794,0.0560255672420171,
4.));
#28751=CARTESIAN_POINT('Ctrl Pts',(0.120878299816185,0.0499406938168944,
4.));
#28752=CARTESIAN_POINT('Ctrl Pts',(0.123857056765335,0.0435961076613069,
4.));
#28753=CARTESIAN_POINT('Ctrl Pts',(0.125170781948423,0.0407979462969676,
4.));
#28754=CARTESIAN_POINT('Ctrl Pts',(0.126390002992329,0.0379525898756446,
4.));
#28755=CARTESIAN_POINT('Ctrl Pts',(0.12751038950843,0.0350750832122783,
4.));
#28756=CARTESIAN_POINT('Ctrl Pts',(0.131085166597008,0.0258939258664803,
4.));
#28757=CARTESIAN_POINT('Ctrl Pts',(0.133669431833427,0.0163619242015854,
4.));
#28758=CARTESIAN_POINT('Ctrl Pts',(0.135230958047781,0.0066616777752228,
4.));
#28759=CARTESIAN_POINT('Ctrl Pts',(0.135923073683569,0.00236223524203686,
4.));
#28760=CARTESIAN_POINT('Ctrl Pts',(0.136413711726375,-0.0019706858607116,
4.));
#28761=CARTESIAN_POINT('Ctrl Pts',(0.136697089502038,-0.00632254181082518,
4.));
#28762=CARTESIAN_POINT('Ctrl Pts',(0.136879678085431,-0.00912656979504798,
4.));
#28763=CARTESIAN_POINT('Ctrl Pts',(0.136975856810266,-0.011936494905405,
4.));
#28764=CARTESIAN_POINT('Ctrl Pts',(0.136984537674321,-0.0147391030393356,
4.));
#28765=CARTESIAN_POINT('Ctrl Pts',(0.137010531466213,-0.0231311723225325,
4.));
#28766=CARTESIAN_POINT('Ctrl Pts',(0.136255503035819,-0.0314800211532621,
4.));
#28767=CARTESIAN_POINT('Ctrl Pts',(0.134693290097439,-0.0396806821547801,
4.));
#28768=CARTESIAN_POINT('Ctrl Pts',(0.133704762250079,-0.0448698478361003,
4.));
#28769=CARTESIAN_POINT('Ctrl Pts',(0.132392592878428,-0.0499999054788172,
4.));
#28770=CARTESIAN_POINT('Ctrl Pts',(0.130776991260223,-0.0550529928649125,
4.));
#28771=CARTESIAN_POINT('Ctrl Pts',(0.129445892801333,-0.0592162449664668,
4.));
#28772=CARTESIAN_POINT('Ctrl Pts',(0.127906314848104,-0.0633316423760335,
4.));
#28773=CARTESIAN_POINT('Ctrl Pts',(0.126180878863323,-0.0673610722009708,
4.));
#28774=CARTESIAN_POINT('Ctrl Pts',(0.122312843187174,-0.0763941388895448,
4.));
#28775=CARTESIAN_POINT('Ctrl Pts',(0.117508253438465,-0.0850205194401279,
4.));
#28776=CARTESIAN_POINT('Ctrl Pts',(0.111900166266883,-0.0931314900308112,
4.));
#28777=CARTESIAN_POINT('Ctrl Pts',(0.108605841530307,-0.097896068439994,
4.));
#28778=CARTESIAN_POINT('Ctrl Pts',(0.105033346987346,-0.102482765945667,
4.));
#28779=CARTESIAN_POINT('Ctrl Pts',(0.101203104491781,-0.106867390005116,
4.));
#28780=CARTESIAN_POINT('Ctrl Pts',(0.0988795404734533,-0.109527261987172,
4.));
#28781=CARTESIAN_POINT('Ctrl Pts',(0.0964620699804362,-0.112111128650417,
4.));
#28782=CARTESIAN_POINT('Ctrl Pts',(0.0939639375491823,-0.114605366763082,
4.));
#28783=CARTESIAN_POINT('Ctrl Pts',(0.0874788757256353,-0.121080319075824,
4.));
#28784=CARTESIAN_POINT('Ctrl Pts',(0.0804377540716352,-0.126968968726175,
4.));
#28785=CARTESIAN_POINT('Ctrl Pts',(0.0729230547225638,-0.132178932127324,
4.));
#28786=CARTESIAN_POINT('Ctrl Pts',(0.0694491809116136,-0.134587379168854,
4.));
#28787=CARTESIAN_POINT('Ctrl Pts',(0.0658808132415588,-0.136845565695848,
4.));
#28788=CARTESIAN_POINT('Ctrl Pts',(0.0622290543017492,-0.138943290379685,
4.));
#28789=CARTESIAN_POINT('Ctrl Pts',(0.0562216582547972,-0.142394192583524,
4.));
#28790=CARTESIAN_POINT('Ctrl Pts',(0.0499865922958981,-0.145412833318798,
4.));
#28791=CARTESIAN_POINT('Ctrl Pts',(0.0435567401413007,-0.147956905966761,
4.));
#28792=CARTESIAN_POINT('Ctrl Pts',(0.0423577886630555,-0.148431290072134,
4.));
#28793=CARTESIAN_POINT('Ctrl Pts',(0.0411520494229064,-0.148889152887265,
4.));
#28794=CARTESIAN_POINT('Ctrl Pts',(0.0399398308045252,-0.149330586455588,
4.));
#28795=CARTESIAN_POINT('Ctrl Pts',(-0.126543984365092,-0.000100563349596846,
3.91934196736194));
#28796=CARTESIAN_POINT('Ctrl Pts',(-0.126601870201444,-0.00676638730964717,
3.91976237798504));
#28797=CARTESIAN_POINT('Ctrl Pts',(-0.126120638953643,-0.0134238307402375,
3.92018278860814));
#28798=CARTESIAN_POINT('Ctrl Pts',(-0.125071086204593,-0.0199904298605203,
3.92060319923124));
#28799=CARTESIAN_POINT('Ctrl Pts',(-0.118463964029756,-0.0613283451774388,
3.92324975925687));
#28800=CARTESIAN_POINT('Ctrl Pts',(-0.089334672430595,-0.0990661662809851,
3.92589631928249));
#28801=CARTESIAN_POINT('Ctrl Pts',(-0.0510182636513927,-0.115928743690777,
3.92854287930812));
#28802=CARTESIAN_POINT('Ctrl Pts',(-0.0127018548721904,-0.132791321100569,
3.93118943933374));
#28803=CARTESIAN_POINT('Ctrl Pts',(0.0348016710870533,-0.128778654816608,
3.93383599935937));
#28804=CARTESIAN_POINT('Ctrl Pts',(0.0697457276620979,-0.10572614363048,
3.93648255938499));
#28805=CARTESIAN_POINT('Ctrl Pts',(0.104689784237142,-0.0826736324443521,
3.93912911941062));
#28806=CARTESIAN_POINT('Ctrl Pts',(0.127074371427988,-0.0405812763560585,
3.94177567943624));
#28807=CARTESIAN_POINT('Ctrl Pts',(0.126652103797309,0.00127848798181101,
3.94442223946187));
#28808=CARTESIAN_POINT('Ctrl Pts',(0.126229836166631,0.0431382523196808,
3.94706879948749));
#28809=CARTESIAN_POINT('Ctrl Pts',(0.103000713714428,0.0847654249071265,
3.94971535951312));
#28810=CARTESIAN_POINT('Ctrl Pts',(0.067598717604338,0.107109484137676,
3.95236191953875));
#28811=CARTESIAN_POINT('Ctrl Pts',(0.0321967214942486,0.129453543368225,
3.95500847956437));
#28812=CARTESIAN_POINT('Ctrl Pts',(-0.0153781482737276,0.132514489241879,
3.95765503958999));
#28813=CARTESIAN_POINT('Ctrl Pts',(-0.0533465659413221,0.114879485769171,
3.96030159961562));
#28814=CARTESIAN_POINT('Ctrl Pts',(-0.0913149836089167,0.0972444822964635,
3.96294815964124));
#28815=CARTESIAN_POINT('Ctrl Pts',(-0.11967694917613,0.0589135294773952,
3.96559471966687));
#28816=CARTESIAN_POINT('Ctrl Pts',(-0.12544884800723,0.0174567123195785,
3.9682412796925));
#28817=CARTESIAN_POINT('Ctrl Pts',(-0.1262490134813,0.0117095024801126,
3.96860817558231));
#28818=CARTESIAN_POINT('Ctrl Pts',(-0.126615029050668,0.00590221784225734,
3.96897507147213));
#28819=CARTESIAN_POINT('Ctrl Pts',(-0.126567406925801,8.9117089303592E-5,
3.96934196736194));
#28820=CARTESIAN_POINT('Ctrl Pts',(-0.0398513841857263,-0.149064942821851,
4.));
#28821=CARTESIAN_POINT('Ctrl Pts',(-0.0894268873061843,-0.13581130730129,
3.99735343997437));
#28822=CARTESIAN_POINT('Ctrl Pts',(-0.173454116750112,-0.0561632816072737,
3.99206031992313));
#28823=CARTESIAN_POINT('Ctrl Pts',(-0.141207051852386,0.115615412698802,
3.98412063984625));
#28824=CARTESIAN_POINT('Ctrl Pts',(0.0205691872966891,0.181176549232701,
3.97618095976937));
#28825=CARTESIAN_POINT('Ctrl Pts',(0.16339053139201,0.0810339956098913,
3.9682412796925));
#28826=CARTESIAN_POINT('Ctrl Pts',(0.156677599794682,-0.0933915431448235,
3.96030159961562));
#28827=CARTESIAN_POINT('Ctrl Pts',(0.00648228676056323,-0.182263829019595,
3.95236191953875));
#28828=CARTESIAN_POINT('Ctrl Pts',(-0.149631704989928,-0.104283093629962,
3.94442223946187));
#28829=CARTESIAN_POINT('Ctrl Pts',(-0.168754687429674,0.0691889583215889,
3.93648255938499));
#28830=CARTESIAN_POINT('Ctrl Pts',(-0.0333654229848094,0.179306981584077,
3.92854287930812));
#28831=CARTESIAN_POINT('Ctrl Pts',(0.132570265831228,0.125258780485074,
3.92060319923124));
#28832=CARTESIAN_POINT('Ctrl Pts',(0.17712875926901,-0.0434751369680033,
3.91266351915436));
#28833=CARTESIAN_POINT('Ctrl Pts',(0.059511610779771,-0.172403375181386,
3.90472383907749));
#28834=CARTESIAN_POINT('Ctrl Pts',(-0.112592720088119,-0.143483428861666,
3.89678415900062));
#28835=CARTESIAN_POINT('Ctrl Pts',(-0.181609867534042,0.0168069012899025,
3.88884447892373));
#28836=CARTESIAN_POINT('Ctrl Pts',(-0.0843490715154628,0.161709102853824,
3.88090479884686));
#28837=CARTESIAN_POINT('Ctrl Pts',(0.0901397770410241,0.158554183500776,
3.87296511876998));
#28838=CARTESIAN_POINT('Ctrl Pts',(0.182098715355847,0.0102306290122647,
3.86502543869311));
#28839=CARTESIAN_POINT('Ctrl Pts',(0.107332199369115,-0.147459841777235,
3.85708575861623));
#28840=CARTESIAN_POINT('Ctrl Pts',(-0.0657052328909015,-0.17013944154474,
3.84914607853936));
#28841=CARTESIAN_POINT('Ctrl Pts',(-0.178584450418103,-0.0370432327022405,
3.84120639846248));
#28842=CARTESIAN_POINT('Ctrl Pts',(-0.127955803747328,0.129968915826709,
3.83326671838561));
#28843=CARTESIAN_POINT('Ctrl Pts',(0.039826267121788,0.177984480821945,
3.82532703830873));
#28844=CARTESIAN_POINT('Ctrl Pts',(0.171144313607041,0.063041501012073,
3.81738735823185));
#28845=CARTESIAN_POINT('Ctrl Pts',(0.145766517224248,-0.109620843643728,
3.80944767815498));
#28846=CARTESIAN_POINT('Ctrl Pts',(-0.0130717883220708,-0.181916836159762,
3.8015079980781));
#28847=CARTESIAN_POINT('Ctrl Pts',(-0.159941861709037,-0.0876539091820477,
3.79356831800123));
#28848=CARTESIAN_POINT('Ctrl Pts',(-0.160372802668024,0.0868629442494614,
3.78562863792435));
#28849=CARTESIAN_POINT('Ctrl Pts',(-0.013970051492431,0.181850060719556,
3.77768895784748));
#28850=CARTESIAN_POINT('Ctrl Pts',(0.145223361235896,0.110339395832533,
3.7697492777706));
#28851=CARTESIAN_POINT('Ctrl Pts',(0.171453565975463,-0.0621955113766863,
3.76180959769372));
#28852=CARTESIAN_POINT('Ctrl Pts',(0.0407047835991549,-0.177785622348059,
3.75386991761685));
#28853=CARTESIAN_POINT('Ctrl Pts',(-0.127312373243651,-0.130599259340906,
3.74593023753997));
#28854=CARTESIAN_POINT('Ctrl Pts',(-0.178765215511242,0.0361608164252855,
3.7379905574631));
#28855=CARTESIAN_POINT('Ctrl Pts',(-0.0665446905722607,0.169812870767156,
3.73005087738622));
#28856=CARTESIAN_POINT('Ctrl Pts',(0.106602640202898,0.147988121222216,
3.72211119730934));
#28857=CARTESIAN_POINT('Ctrl Pts',(0.182147017152552,-0.0093311876933208,
3.71417151723247));
#28858=CARTESIAN_POINT('Ctrl Pts',(0.0909217261957518,-0.158107073301583,
3.70623183715559));
#28859=CARTESIAN_POINT('Ctrl Pts',(-0.0835494302172658,-0.162123717048593,
3.69829215707872));
#28860=CARTESIAN_POINT('Ctrl Pts',(-0.181524627767524,-0.0177035712699219,
3.69035247700185));
#28861=CARTESIAN_POINT('Ctrl Pts',(-0.113300002982309,0.14292556192831,
3.68241279692496));
#28862=CARTESIAN_POINT('Ctrl Pts',(0.0586595287281965,0.172695299861449,
3.67447311684809));
#28863=CARTESIAN_POINT('Ctrl Pts',(0.176911729524118,0.0443491475303153,
3.66653343677121));
#28864=CARTESIAN_POINT('Ctrl Pts',(0.133187572742707,-0.124602076359984,
3.65859375669434));
#28865=CARTESIAN_POINT('Ctrl Pts',(-0.0324800977009374,-0.179470471240069,
3.65065407661746));
#28866=CARTESIAN_POINT('Ctrl Pts',(-0.168409729113823,-0.0700197840611982,
3.64271439654059));
#28867=CARTESIAN_POINT('Ctrl Pts',(-0.150147241221285,0.103539428007117,
3.63477471646371));
#28868=CARTESIAN_POINT('Ctrl Pts',(0.00558664719359638,0.182300288895857,
3.62683503638684));
#28869=CARTESIAN_POINT('Ctrl Pts',(0.156205528517827,0.094151159125646,
3.61889535630996));
#28870=CARTESIAN_POINT('Ctrl Pts',(0.163806179027695,-0.0802006497663837,
3.61095567623308));
#28871=CARTESIAN_POINT('Ctrl Pts',(0.0214296163208854,-0.181122531330724,
3.60301599615621));
#28872=CARTESIAN_POINT('Ctrl Pts',(-0.140567416427732,-0.116212810634341,
3.59507631607934));
#28873=CARTESIAN_POINT('Ctrl Pts',(-0.173864117377934,0.0550988535555318,
3.58713663600245));
#28874=CARTESIAN_POINT('Ctrl Pts',(-0.0479747871584019,0.175962994372803,
3.57919695592558));
#28875=CARTESIAN_POINT('Ctrl Pts',(0.121839171429706,0.13571993663382,3.5712572758487));
#28876=CARTESIAN_POINT('Ctrl Pts',(0.180099946935509,-0.0287862221383337,
3.56331759577183));
#28877=CARTESIAN_POINT('Ctrl Pts',(0.0734653204375665,-0.166934393666355,
3.55537791569495));
#28878=CARTESIAN_POINT('Ctrl Pts',(-0.100432512451176,-0.152245088347237,
3.54743823561807));
#28879=CARTESIAN_POINT('Ctrl Pts',(-0.182376563237206,0.00184389181179004,
3.5394985555412));
#28880=CARTESIAN_POINT('Ctrl Pts',(-0.0973408901199132,0.154229940417525,
3.53155887546432));
#28881=CARTESIAN_POINT('Ctrl Pts',(0.0768181056158631,0.16543527210962,
3.52361919538745));
#28882=CARTESIAN_POINT('Ctrl Pts',(0.180643771975638,0.0251157687415861,
3.51567951531057));
#28883=CARTESIAN_POINT('Ctrl Pts',(0.11907687582224,-0.13808957637103,3.50773983523369));
#28884=CARTESIAN_POINT('Ctrl Pts',(-0.0515150906951779,-0.17507869823889,
3.49980015515682));
#28885=CARTESIAN_POINT('Ctrl Pts',(-0.174944455635001,-0.0513330523253054,
3.49186047507995));
#28886=CARTESIAN_POINT('Ctrl Pts',(-0.15040278985559,0.061813268541742,
3.4865673550287));
#28887=CARTESIAN_POINT('Ctrl Pts',(-0.116913659442529,0.100696009035892,
3.48392079500307));
#28888=CARTESIAN_POINT('Ctrl Pts',(-0.0374537582415214,-0.140096572423085,
4.00535973499898));
#28889=CARTESIAN_POINT('Ctrl Pts',(-0.0840465917531983,-0.127640331046503,
4.00271317497335));
#28890=CARTESIAN_POINT('Ctrl Pts',(-0.163018391644278,-0.0527842636924701,
3.9974200549221));
#28891=CARTESIAN_POINT('Ctrl Pts',(-0.132711445038627,0.108659505929172,
3.98948037484522));
#28892=CARTESIAN_POINT('Ctrl Pts',(0.0193316589618159,0.170276210290963,
3.98154069476835));
#28893=CARTESIAN_POINT('Ctrl Pts',(0.153560273670542,0.0761586515231869,
3.97360101469147));
#28894=CARTESIAN_POINT('Ctrl Pts',(0.147251220113796,-0.0877727173150906,
3.9656613346146));
#28895=CARTESIAN_POINT('Ctrl Pts',(0.00609228527799324,-0.171298074778515,
3.95772165453772));
#28896=CARTESIAN_POINT('Ctrl Pts',(-0.140629235808745,-0.0980089865709976,
3.94978197446085));
#28897=CARTESIAN_POINT('Ctrl Pts',(-0.158601699646316,0.0650262612179893,
3.94184229438397));
#28898=CARTESIAN_POINT('Ctrl Pts',(-0.0313580195928739,0.168519123651227,
3.93390261430709));
#28899=CARTESIAN_POINT('Ctrl Pts',(0.124594284186381,0.117722688377688,
3.92596293423022));
#28900=CARTESIAN_POINT('Ctrl Pts',(0.166471952300676,-0.0408594909006909,
3.91802325415334));
#28901=CARTESIAN_POINT('Ctrl Pts',(0.0559311433781364,-0.162030867082874,
3.91008357407647));
#28902=CARTESIAN_POINT('Ctrl Pts',(-0.105818671147842,-0.134850865686472,
3.90214389399959));
#28903=CARTESIAN_POINT('Ctrl Pts',(-0.170683458351015,0.0157957278163147,
3.89420421392272));
#28904=CARTESIAN_POINT('Ctrl Pts',(-0.0792742785975418,0.151980006905501,
3.88626453384583));
#28905=CARTESIAN_POINT('Ctrl Pts',(0.0847165910600508,0.149014900695642,
3.87832485376897));
#28906=CARTESIAN_POINT('Ctrl Pts',(0.171142895043338,0.00961511158303258,
3.87038517369209));
#28907=CARTESIAN_POINT('Ctrl Pts',(0.100874645356521,-0.138588040970374,
3.86244549361521));
#28908=CARTESIAN_POINT('Ctrl Pts',(-0.0617521312792973,-0.159903141162322,
3.85450581353833));
#28909=CARTESIAN_POINT('Ctrl Pts',(-0.16784006298206,-0.0348145568958948,
3.84656613346146));
#28910=CARTESIAN_POINT('Ctrl Pts',(-0.120257447440646,0.122149442277835,
3.83862645338458));
#28911=CARTESIAN_POINT('Ctrl Pts',(0.0374301523251976,0.167276190066077,
3.83068677330771));
#28912=CARTESIAN_POINT('Ctrl Pts',(0.16084755591865,0.0592486606509017,
3.82274709323083));
#28913=CARTESIAN_POINT('Ctrl Pts',(0.136996593904535,-0.103025595219711,
3.81480741315396));
#28914=CARTESIAN_POINT('Ctrl Pts',(-0.0122853348660984,-0.170971958460368,
3.80686773307708));
#28915=CARTESIAN_POINT('Ctrl Pts',(-0.150319090379167,-0.0823802834081873,
3.7989280530002));
#28916=CARTESIAN_POINT('Ctrl Pts',(-0.150724104127725,0.0816369062340208,
3.79098837292333));
#28917=CARTESIAN_POINT('Ctrl Pts',(-0.0131295547672976,0.170909200509922,
3.78304869284645));
#28918=CARTESIAN_POINT('Ctrl Pts',(0.136486116452099,0.103700916303616,
3.77510901276958));
#28919=CARTESIAN_POINT('Ctrl Pts',(0.161138202371193,-0.0584535692901865,
3.7671693326927));
#28920=CARTESIAN_POINT('Ctrl Pts',(0.0382558135770412,-0.167089295749672,
3.75922965261583));
#28921=CARTESIAN_POINT('Ctrl Pts',(-0.119652728407108,-0.122741861689914,
3.75128997253895));
#28922=CARTESIAN_POINT('Ctrl Pts',(-0.168009952491177,0.0339852304727166,
3.74335029246208));
#28923=CARTESIAN_POINT('Ctrl Pts',(-0.0625410836756577,0.159596218248545,
3.73541061238519));
#28924=CARTESIAN_POINT('Ctrl Pts',(0.100188979521,0.139084536914507,3.72747093230832));
#28925=CARTESIAN_POINT('Ctrl Pts',(0.171188290801939,-0.00876978441559563,
3.71953125223144));
#28926=CARTESIAN_POINT('Ctrl Pts',(0.0854514948832616,-0.148594690515994,
3.71159157215457));
#28927=CARTESIAN_POINT('Ctrl Pts',(-0.078522747064207,-0.15236967617626,
3.7036518920777));
#28928=CARTESIAN_POINT('Ctrl Pts',(-0.170603346965352,-0.0166384503801673,
3.69571221200081));
#28929=CARTESIAN_POINT('Ctrl Pts',(-0.106483400945028,0.134326562361009,
3.68777253192394));
#28930=CARTESIAN_POINT('Ctrl Pts',(0.0551303261464719,0.162305228353258,
3.67983285184707));
#28931=CARTESIAN_POINT('Ctrl Pts',(0.166267979972926,0.0416809173321745,
3.67189317177019));
#28932=CARTESIAN_POINT('Ctrl Pts',(0.125174451332285,-0.117105494319316,
3.66395349169331));
#28933=CARTESIAN_POINT('Ctrl Pts',(-0.030525959180801,-0.168672777085747,
3.65601381161644));
#28934=CARTESIAN_POINT('Ctrl Pts',(-0.158277495465476,-0.0658071010063173,
3.64807413153956));
#28935=CARTESIAN_POINT('Ctrl Pts',(-0.141113755224281,0.0973100629822772,
3.64013445146269));
#28936=CARTESIAN_POINT('Ctrl Pts',(0.0052505311332342,0.171332341076135,
3.63219477138581));
#28937=CARTESIAN_POINT('Ctrl Pts',(0.146807550619315,0.0884866316215429,
3.62425509130893));
#28938=CARTESIAN_POINT('Ctrl Pts',(0.153950914206089,-0.0753754432509509,
3.61631541123206));
#28939=CARTESIAN_POINT('Ctrl Pts',(0.0201403209773194,-0.170225442331889,
3.60837573115518));
#28940=CARTESIAN_POINT('Ctrl Pts',(-0.132110292756286,-0.109220961906395,
3.60043605107832));
#28941=CARTESIAN_POINT('Ctrl Pts',(-0.163403724919573,0.0517838760841091,
3.59249637100142));
#28942=CARTESIAN_POINT('Ctrl Pts',(-0.0450884233166185,0.165376324696236,
3.58455669092456));
#28943=CARTESIAN_POINT('Ctrl Pts',(0.114508817305019,0.12755445762053,3.57661701084768));
#28944=CARTESIAN_POINT('Ctrl Pts',(0.169264380890674,-0.0270543226210457,
3.56867733077081));
#28945=CARTESIAN_POINT('Ctrl Pts',(0.0690453395039173,-0.156890922368865,
3.56073765069393));
#28946=CARTESIAN_POINT('Ctrl Pts',(-0.0943900724603247,-0.14308538709325,
3.55279797061705));
#28947=CARTESIAN_POINT('Ctrl Pts',(-0.171404026434103,0.00173295556863096,
3.54485829054018));
#28948=CARTESIAN_POINT('Ctrl Pts',(-0.0914844550586914,0.144950822161685,
3.5369186104633));
#28949=CARTESIAN_POINT('Ctrl Pts',(0.0721964071034376,0.155481994234803,
3.52897893038643));
#28950=CARTESIAN_POINT('Ctrl Pts',(0.169775487141934,0.0236046990516893,
3.52103925030955));
#28951=CARTESIAN_POINT('Ctrl Pts',(0.111912712954128,-0.129781529920537,
3.51309957023267));
#28952=CARTESIAN_POINT('Ctrl Pts',(-0.0484157273859087,-0.164545231516157,
3.5051598901558));
#28953=CARTESIAN_POINT('Ctrl Pts',(-0.164419065508765,-0.0482446412057121,
3.49722021007893));
#28954=CARTESIAN_POINT('Ctrl Pts',(-0.141353928983959,0.0580943237828579,
3.49192709002767));
#28955=CARTESIAN_POINT('Ctrl Pts',(-0.109879644719102,0.094637715988474,
3.48928053000205));
#28956=CARTESIAN_POINT('Ctrl Pts',(-0.0350561322973164,-0.13112820202432,
4.01071946999795));
#28957=CARTESIAN_POINT('Ctrl Pts',(-0.0786662962002123,-0.119469354791716,
4.00807290997233));
#28958=CARTESIAN_POINT('Ctrl Pts',(-0.152582666538444,-0.0494052457776665,
4.00277978992108));
#28959=CARTESIAN_POINT('Ctrl Pts',(-0.124215838224868,0.101703599159542,
3.9948401098442));
#28960=CARTESIAN_POINT('Ctrl Pts',(0.0180941306269427,0.159375871349225,
3.98690042976732));
#28961=CARTESIAN_POINT('Ctrl Pts',(0.143730015949074,0.0712833074364824,
3.97896074969045));
#28962=CARTESIAN_POINT('Ctrl Pts',(0.137824840432911,-0.0821538914853577,
3.97102106961357));
#28963=CARTESIAN_POINT('Ctrl Pts',(0.0057022837954231,-0.160332320537436,
3.9630813895367));
#28964=CARTESIAN_POINT('Ctrl Pts',(-0.131626766627563,-0.0917348795120337,
3.95514170945982));
#28965=CARTESIAN_POINT('Ctrl Pts',(-0.148448711862958,0.0608635641143897,
3.94720202938295));
#28966=CARTESIAN_POINT('Ctrl Pts',(-0.0293506162009384,0.157731265718376,
3.93926234930607));
#28967=CARTESIAN_POINT('Ctrl Pts',(0.116618302541534,0.110186596270301,
3.93132266922919));
#28968=CARTESIAN_POINT('Ctrl Pts',(0.155815145332341,-0.0382438448333786,
3.92338298915232));
#28969=CARTESIAN_POINT('Ctrl Pts',(0.0523506759765019,-0.151658358984361,
3.91544330907544));
#28970=CARTESIAN_POINT('Ctrl Pts',(-0.0990446222075651,-0.126218302511277,
3.90750362899857));
#28971=CARTESIAN_POINT('Ctrl Pts',(-0.159757049167988,0.0147845543427269,
3.89956394892169));
#28972=CARTESIAN_POINT('Ctrl Pts',(-0.0741994856796208,0.142250910957177,
3.89162426884482));
#28973=CARTESIAN_POINT('Ctrl Pts',(0.0792934050790776,0.139475617890508,
3.88368458876794));
#28974=CARTESIAN_POINT('Ctrl Pts',(0.160187074730829,0.0089995941538004,
3.87574490869107));
#28975=CARTESIAN_POINT('Ctrl Pts',(0.0944170913439271,-0.129716240163513,
3.86780522861419));
#28976=CARTESIAN_POINT('Ctrl Pts',(-0.0577990296676931,-0.149666840779905,
3.85986554853731));
#28977=CARTESIAN_POINT('Ctrl Pts',(-0.157095675546018,-0.0325858810895492,
3.85192586846044));
#28978=CARTESIAN_POINT('Ctrl Pts',(-0.112559091133964,0.114329968728961,
3.84398618838356));
#28979=CARTESIAN_POINT('Ctrl Pts',(0.0350340375286068,0.156567899310209,
3.83604650830669));
#28980=CARTESIAN_POINT('Ctrl Pts',(0.150550798230259,0.0554558202897304,
3.8281068282298));
#28981=CARTESIAN_POINT('Ctrl Pts',(0.128226670584821,-0.0964303467956928,
3.82016714815294));
#28982=CARTESIAN_POINT('Ctrl Pts',(-0.0114988814101258,-0.160027080760974,
3.81222746807605));
#28983=CARTESIAN_POINT('Ctrl Pts',(-0.140696319049298,-0.0771066576343268,
3.80428778799918));
#28984=CARTESIAN_POINT('Ctrl Pts',(-0.141075405587426,0.0764108682185801,
3.79634810792231));
#28985=CARTESIAN_POINT('Ctrl Pts',(-0.0122890580421644,0.159968340300288,
3.78840842784543));
#28986=CARTESIAN_POINT('Ctrl Pts',(0.127748871668302,0.0970624367746977,
3.78046874776856));
#28987=CARTESIAN_POINT('Ctrl Pts',(0.150822838766923,-0.0547116272036868,
3.77252906769167));
#28988=CARTESIAN_POINT('Ctrl Pts',(0.0358068435549273,-0.156392969151285,
3.7645893876148));
#28989=CARTESIAN_POINT('Ctrl Pts',(-0.111993083570565,-0.114884464038922,
3.75664970753792));
#28990=CARTESIAN_POINT('Ctrl Pts',(-0.157254689471112,0.0318096445201475,
3.74871002746105));
#28991=CARTESIAN_POINT('Ctrl Pts',(-0.0585374767790549,0.149379565729933,
3.74077034738417));
#28992=CARTESIAN_POINT('Ctrl Pts',(0.0937753188391016,0.130180952606797,
3.7328306673073));
#28993=CARTESIAN_POINT('Ctrl Pts',(0.160229564451327,-0.00820838113787044,
3.72489098723042));
#28994=CARTESIAN_POINT('Ctrl Pts',(0.0799812635707716,-0.139082307730405,
3.71695130715355));
#28995=CARTESIAN_POINT('Ctrl Pts',(-0.0734960639111485,-0.142615635303926,
3.70901162707667));
#28996=CARTESIAN_POINT('Ctrl Pts',(-0.15968206616318,-0.015573329490413,
3.7010719469998));
#28997=CARTESIAN_POINT('Ctrl Pts',(-0.0996667989077476,0.125727562793709,
3.69313226692292));
#28998=CARTESIAN_POINT('Ctrl Pts',(0.0516011235647474,0.151915156845068,
3.68519258684604));
#28999=CARTESIAN_POINT('Ctrl Pts',(0.155624230421734,0.039012687134034,
3.67725290676917));
#29000=CARTESIAN_POINT('Ctrl Pts',(0.117161329921862,-0.109608912278647,
3.66931322669229));
#29001=CARTESIAN_POINT('Ctrl Pts',(-0.0285718206606646,-0.157875082931424,
3.66137354661541));
#29002=CARTESIAN_POINT('Ctrl Pts',(-0.148145261817129,-0.0615944179514364,
3.65343386653854));
#29003=CARTESIAN_POINT('Ctrl Pts',(-0.132080269227278,0.0910806979574378,
3.64549418646166));
#29004=CARTESIAN_POINT('Ctrl Pts',(0.00491441507287188,0.160364393256412,
3.63755450638479));
#29005=CARTESIAN_POINT('Ctrl Pts',(0.137409572720802,0.08282210411744,3.62961482630791));
#29006=CARTESIAN_POINT('Ctrl Pts',(0.144095649384483,-0.0705502367355182,
3.62167514623104));
#29007=CARTESIAN_POINT('Ctrl Pts',(0.0188510256337537,-0.159328353333054,
3.61373546615416));
#29008=CARTESIAN_POINT('Ctrl Pts',(-0.12365316908484,-0.102229113178448,
3.60579578607729));
#29009=CARTESIAN_POINT('Ctrl Pts',(-0.152943332461211,0.0484688986126864,
3.5978561060004));
#29010=CARTESIAN_POINT('Ctrl Pts',(-0.0422020594748354,0.15478965501967,
3.58991642592354));
#29011=CARTESIAN_POINT('Ctrl Pts',(0.107178463180333,0.119388978607241,
3.58197674584666));
#29012=CARTESIAN_POINT('Ctrl Pts',(0.15842881484584,-0.0253224231037578,
3.57403706576978));
#29013=CARTESIAN_POINT('Ctrl Pts',(0.0646253585702682,-0.146847451071376,
3.56609738569291));
#29014=CARTESIAN_POINT('Ctrl Pts',(-0.0883476324694729,-0.133925685839263,
3.55815770561603));
#29015=CARTESIAN_POINT('Ctrl Pts',(-0.160431489631001,0.00162201932547174,
3.55021802553915));
#29016=CARTESIAN_POINT('Ctrl Pts',(-0.0856280199974695,0.135671703905846,
3.54227834546228));
#29017=CARTESIAN_POINT('Ctrl Pts',(0.067574708591012,0.145528716359985,
3.5343386653854));
#29018=CARTESIAN_POINT('Ctrl Pts',(0.15890720230823,0.0220936293617927,
3.52639898530853));
#29019=CARTESIAN_POINT('Ctrl Pts',(0.104748550086015,-0.121473483470044,
3.51845930523165));
#29020=CARTESIAN_POINT('Ctrl Pts',(-0.0453163640766394,-0.154011764793424,
3.51051962515478));
#29021=CARTESIAN_POINT('Ctrl Pts',(-0.153893675382528,-0.0451562300861186,
3.5025799450779));
#29022=CARTESIAN_POINT('Ctrl Pts',(-0.132305068112328,0.0543753790239735,
3.49728682502665));
#29023=CARTESIAN_POINT('Ctrl Pts',(-0.102845629995675,0.0885794229410565,
3.49464026500102));
#29024=CARTESIAN_POINT('Ctrl Pts',(-0.0326585063531114,-0.122159831625554,
4.01607920499693));
#29025=CARTESIAN_POINT('Ctrl Pts',(-0.0732860006472263,-0.111298378536929,
4.0134326449713));
#29026=CARTESIAN_POINT('Ctrl Pts',(-0.142146941432609,-0.046026227862863,
4.00813952492006));
#29027=CARTESIAN_POINT('Ctrl Pts',(-0.11572023141111,0.0947476923899126,
4.00019984484318));
#29028=CARTESIAN_POINT('Ctrl Pts',(0.0168566022920696,0.148475532407486,
3.9922601647663));
#29029=CARTESIAN_POINT('Ctrl Pts',(0.133899758227606,0.0664079633497781,
3.98432048468943));
#29030=CARTESIAN_POINT('Ctrl Pts',(0.128398460752025,-0.076535065655625,
3.97638080461255));
#29031=CARTESIAN_POINT('Ctrl Pts',(0.00531228231285306,-0.149366566296356,
3.96844112453568));
#29032=CARTESIAN_POINT('Ctrl Pts',(-0.12262429744638,-0.0854607724530698,
3.9605014444588));
#29033=CARTESIAN_POINT('Ctrl Pts',(-0.1382957240796,0.0567008670107902,
3.95256176438192));
#29034=CARTESIAN_POINT('Ctrl Pts',(-0.0273432128090029,0.146943407785525,
3.94462208430505));
#29035=CARTESIAN_POINT('Ctrl Pts',(0.108642320896687,0.102650504162914,
3.93668240422817));
#29036=CARTESIAN_POINT('Ctrl Pts',(0.145158338364007,-0.0356281987660663,
3.9287427241513));
#29037=CARTESIAN_POINT('Ctrl Pts',(0.0487702085748674,-0.141285850885848,
3.92080304407442));
#29038=CARTESIAN_POINT('Ctrl Pts',(-0.0922705732672884,-0.117585739336083,
3.91286336399754));
#29039=CARTESIAN_POINT('Ctrl Pts',(-0.148830639984962,0.0137733808691391,
3.90492368392067));
#29040=CARTESIAN_POINT('Ctrl Pts',(-0.0691246927616998,0.132521815008853,
3.89698400384379));
#29041=CARTESIAN_POINT('Ctrl Pts',(0.0738702190981043,0.129936335085374,
3.88904432376692));
#29042=CARTESIAN_POINT('Ctrl Pts',(0.149231254418321,0.00838407672456824,
3.88110464369004));
#29043=CARTESIAN_POINT('Ctrl Pts',(0.0879595373313327,-0.120844439356652,
3.87316496361317));
#29044=CARTESIAN_POINT('Ctrl Pts',(-0.0538459280560888,-0.139430540397488,
3.86522528353628));
#29045=CARTESIAN_POINT('Ctrl Pts',(-0.146351288109975,-0.0303572052832036,
3.85728560345941));
#29046=CARTESIAN_POINT('Ctrl Pts',(-0.104860734827282,0.106510495180087,
3.84934592338253));
#29047=CARTESIAN_POINT('Ctrl Pts',(0.0326379227320163,0.145859608554342,
3.84140624330567));
#29048=CARTESIAN_POINT('Ctrl Pts',(0.140254040541868,0.0516629799285589,
3.83346656322878));
#29049=CARTESIAN_POINT('Ctrl Pts',(0.119456747265108,-0.0898350983716749,
3.82552688315191));
#29050=CARTESIAN_POINT('Ctrl Pts',(-0.0107124279541533,-0.14908220306158,
3.81758720307504));
#29051=CARTESIAN_POINT('Ctrl Pts',(-0.131073547719428,-0.0718330318604663,
3.80964752299816));
#29052=CARTESIAN_POINT('Ctrl Pts',(-0.131426707047127,0.0711848302031395,
3.80170784292129));
#29053=CARTESIAN_POINT('Ctrl Pts',(-0.0114485613170311,0.149027480090653,
3.7937681628444));
#29054=CARTESIAN_POINT('Ctrl Pts',(0.119011626884504,0.0904239572457801,
3.78582848276753));
#29055=CARTESIAN_POINT('Ctrl Pts',(0.140507475162653,-0.0509696851171873,
3.77788880269065));
#29056=CARTESIAN_POINT('Ctrl Pts',(0.0333578735328136,-0.145696642552897,
3.76994912261378));
#29057=CARTESIAN_POINT('Ctrl Pts',(-0.104333438734023,-0.10702706638793,
3.7620094425369));
#29058=CARTESIAN_POINT('Ctrl Pts',(-0.146499426451047,0.0296340585675785,
3.75406976246003));
#29059=CARTESIAN_POINT('Ctrl Pts',(-0.0545338698824522,0.139162913211322,
3.74613008238315));
#29060=CARTESIAN_POINT('Ctrl Pts',(0.0873616581572035,0.121277368299088,
3.73819040230628));
#29061=CARTESIAN_POINT('Ctrl Pts',(0.149270838100714,-0.00764697786014525,
3.7302507222294));
#29062=CARTESIAN_POINT('Ctrl Pts',(0.0745110322582815,-0.129569924944816,
3.72231104215252));
#29063=CARTESIAN_POINT('Ctrl Pts',(-0.0684693807580898,-0.132861594431592,
3.71437136207565));
#29064=CARTESIAN_POINT('Ctrl Pts',(-0.148760785361007,-0.0145082086006585,
3.70643168199877));
#29065=CARTESIAN_POINT('Ctrl Pts',(-0.0928501968704667,0.117128563226408,
3.6984920019219));
#29066=CARTESIAN_POINT('Ctrl Pts',(0.0480719209830229,0.141525085336877,
3.69055232184502));
#29067=CARTESIAN_POINT('Ctrl Pts',(0.144980480870543,0.0363444569358934,
3.68261264176815));
#29068=CARTESIAN_POINT('Ctrl Pts',(0.10914820851144,-0.102112330237978,
3.67467296169127));
#29069=CARTESIAN_POINT('Ctrl Pts',(-0.0266176821405283,-0.147077388777102,
3.66673328161439));
#29070=CARTESIAN_POINT('Ctrl Pts',(-0.138013028168781,-0.0573817348965553,
3.65879360153751));
#29071=CARTESIAN_POINT('Ctrl Pts',(-0.123046783230275,0.0848513329325982,
3.65085392146064));
#29072=CARTESIAN_POINT('Ctrl Pts',(0.00457829901250977,0.149396445436689,
3.64291424138376));
#29073=CARTESIAN_POINT('Ctrl Pts',(0.128011594822289,0.0771575766133371,
3.63497456130689));
#29074=CARTESIAN_POINT('Ctrl Pts',(0.134240384562878,-0.0657250302200856,
3.62703488123001));
#29075=CARTESIAN_POINT('Ctrl Pts',(0.0175617302901878,-0.148431264334219,
3.61909520115314));
#29076=CARTESIAN_POINT('Ctrl Pts',(-0.115196045413394,-0.0952372644505018,
3.61115552107626));
#29077=CARTESIAN_POINT('Ctrl Pts',(-0.14248294000285,0.0451539211412638,
3.60321584099938));
#29078=CARTESIAN_POINT('Ctrl Pts',(-0.039315695633052,0.144202985343104,
3.59527616092251));
#29079=CARTESIAN_POINT('Ctrl Pts',(0.0998481090556468,0.111223499593951,
3.58733648084563));
#29080=CARTESIAN_POINT('Ctrl Pts',(0.147593248801005,-0.0235905235864699,
3.57939680076876));
#29081=CARTESIAN_POINT('Ctrl Pts',(0.0602053776366188,-0.136803979773886,
3.57145712069188));
#29082=CARTESIAN_POINT('Ctrl Pts',(-0.0823051924786211,-0.124765984585276,
3.56351744061501));
#29083=CARTESIAN_POINT('Ctrl Pts',(-0.149458952827898,0.00151108308231263,
3.55557776053813));
#29084=CARTESIAN_POINT('Ctrl Pts',(-0.0797715849362477,0.126392585650007,
3.54763808046126));
#29085=CARTESIAN_POINT('Ctrl Pts',(0.0629530100785864,0.135575438485168,
3.53969840038438));
#29086=CARTESIAN_POINT('Ctrl Pts',(0.148038917474527,0.020582559671896,
3.5317587203075));
#29087=CARTESIAN_POINT('Ctrl Pts',(0.097584387217902,-0.113165437019551,
3.52381904023062));
#29088=CARTESIAN_POINT('Ctrl Pts',(-0.0422170007673702,-0.143478298070691,
3.51587936015375));
#29089=CARTESIAN_POINT('Ctrl Pts',(-0.143368285256292,-0.0420678189665254,
3.50793968007687));
#29090=CARTESIAN_POINT('Ctrl Pts',(-0.123256207240696,0.0506564342650893,
3.50264656002563));
#29091=CARTESIAN_POINT('Ctrl Pts',(-0.0958116152722475,0.0825211298936389,
3.5));
#29092=CARTESIAN_POINT('Ctrl Pts',(-0.126283770505697,7.06948412972308E-5,
3.95565803263806));
#29093=CARTESIAN_POINT('Ctrl Pts',(-0.126367959766412,0.0165211867142232,
3.95462594321935));
#29094=CARTESIAN_POINT('Ctrl Pts',(-0.123384590961307,0.0329424219101817,
3.95359385380063));
#29095=CARTESIAN_POINT('Ctrl Pts',(-0.117191734428964,0.0480476838959361,
3.95256176438192));
#29096=CARTESIAN_POINT('Ctrl Pts',(-0.101311553656068,0.086781713935702,
3.9499152043563));
#29097=CARTESIAN_POINT('Ctrl Pts',(-0.0643273832325353,0.116862560860614,
3.94726864433067));
#29098=CARTESIAN_POINT('Ctrl Pts',(-0.0231710424031541,0.124520833719301,
3.94462208430505));
#29099=CARTESIAN_POINT('Ctrl Pts',(0.0179852984262271,0.132179106577988,
3.94197552427942));
#29100=CARTESIAN_POINT('Ctrl Pts',(0.0633138096614572,0.117414805370451,
3.9393289642538));
#29101=CARTESIAN_POINT('Ctrl Pts',(0.0920640681902922,0.0869862042785193,
3.93668240422817));
#29102=CARTESIAN_POINT('Ctrl Pts',(0.120814326719127,0.0565576031865874,
3.93403584420254));
#29103=CARTESIAN_POINT('Ctrl Pts',(0.132986332541567,0.0104647022102606,
3.93138928417692));
#29104=CARTESIAN_POINT('Ctrl Pts',(0.123007647154597,-0.0301913569645331,
3.9287427241513));
#29105=CARTESIAN_POINT('Ctrl Pts',(0.113028961767627,-0.0708474161393267,
3.92609616412567));
#29106=CARTESIAN_POINT('Ctrl Pts',(0.0808995851712473,-0.106066633512587,
3.92344960410005));
#29107=CARTESIAN_POINT('Ctrl Pts',(0.0413280998993647,-0.11972622360759,
3.92080304407442));
#29108=CARTESIAN_POINT('Ctrl Pts',(0.00175661462748208,-0.133385813702593,
3.91815648404879));
#29109=CARTESIAN_POINT('Ctrl Pts',(-0.0452569793199031,-0.125485776519338,
3.91550992402317));
#29110=CARTESIAN_POINT('Ctrl Pts',(-0.0781904540798746,-0.0996425712268402,
3.91286336399754));
#29111=CARTESIAN_POINT('Ctrl Pts',(-0.10807787979064,-0.0761896290779491,
3.91046158687771));
#29112=CARTESIAN_POINT('Ctrl Pts',(-0.126369304595299,-0.037959184630699,
3.90805980975789));
#29113=CARTESIAN_POINT('Ctrl Pts',(-0.126614009842867,6.71750503076223E-5,
3.90565803263806));
#29114=CARTESIAN_POINT('Ctrl Pts',(-0.0398513841857263,-0.149064942821851,
4.));
#29115=CARTESIAN_POINT('Ctrl Pts',(-0.0498814023543805,-0.14540001546545,
4.));
#29116=CARTESIAN_POINT('Ctrl Pts',(-0.0594354697797451,-0.140634945951871,
4.));
#29117=CARTESIAN_POINT('Ctrl Pts',(-0.0684028880593604,-0.13492060142061,
4.));
#29118=CARTESIAN_POINT('Ctrl Pts',(-0.0752795449518356,-0.130538561296954,
4.));
#29119=CARTESIAN_POINT('Ctrl Pts',(-0.0818109545260972,-0.125596962852027,
4.));
#29120=CARTESIAN_POINT('Ctrl Pts',(-0.0879325986341956,-0.120150358192012,
4.));
#29121=CARTESIAN_POINT('Ctrl Pts',(-0.0903223739843738,-0.118024105615282,
4.));
#29122=CARTESIAN_POINT('Ctrl Pts',(-0.0926479810229214,-0.115821878910758,
4.));
#29123=CARTESIAN_POINT('Ctrl Pts',(-0.0948977224364798,-0.11355536832373,
4.));
#29124=CARTESIAN_POINT('Ctrl Pts',(-0.1022475948872,-0.106150711227375,
4.));
#29125=CARTESIAN_POINT('Ctrl Pts',(-0.108817076574654,-0.0980392058992304,
4.));
#29126=CARTESIAN_POINT('Ctrl Pts',(-0.114476228961537,-0.0893439955398699,
4.));
#29127=CARTESIAN_POINT('Ctrl Pts',(-0.117310911144628,-0.0849885450768213,
4.));
#29128=CARTESIAN_POINT('Ctrl Pts',(-0.119916487835761,-0.0804862654238585,
4.));
#29129=CARTESIAN_POINT('Ctrl Pts',(-0.122271719969265,-0.0758513570938915,
4.));
#29130=CARTESIAN_POINT('Ctrl Pts',(-0.123706258421051,-0.073028300238791,
4.));
#29131=CARTESIAN_POINT('Ctrl Pts',(-0.12504717142243,-0.0701567413128179,
4.));
#29132=CARTESIAN_POINT('Ctrl Pts',(-0.126284991686486,-0.067251866211871,
4.));
#29133=CARTESIAN_POINT('Ctrl Pts',(-0.1295973650463,-0.0594784994498528,
4.));
#29134=CARTESIAN_POINT('Ctrl Pts',(-0.132185052379765,-0.051445045564302,
4.));
#29135=CARTESIAN_POINT('Ctrl Pts',(-0.133964990884521,-0.0432169428549209,
4.));
#29136=CARTESIAN_POINT('Ctrl Pts',(-0.135518726559135,-0.0360345055517295,
4.));
#29137=CARTESIAN_POINT('Ctrl Pts',(-0.13645631947854,-0.0287032207927444,
4.));
#29138=CARTESIAN_POINT('Ctrl Pts',(-0.136789702571871,-0.0212983790736885,
4.));
#29139=CARTESIAN_POINT('Ctrl Pts',(-0.13693233353465,-0.0181303728827948,
4.));
#29140=CARTESIAN_POINT('Ctrl Pts',(-0.136963744111631,-0.0149584576035291,
4.));
#29141=CARTESIAN_POINT('Ctrl Pts',(-0.136886254945713,-0.0117904221806244,
4.));
#29142=CARTESIAN_POINT('Ctrl Pts',(-0.136677592311597,-0.00325954423806801,
4.));
#29143=CARTESIAN_POINT('Ctrl Pts',(-0.135681410366555,0.00524856144622462,
4.));
#29144=CARTESIAN_POINT('Ctrl Pts',(-0.133925248777689,0.0136159175851835,
4.));
#29145=CARTESIAN_POINT('Ctrl Pts',(-0.132934632228228,0.018335780221422,
4.));
#29146=CARTESIAN_POINT('Ctrl Pts',(-0.131701699385377,0.0230107212566983,
4.));
#29147=CARTESIAN_POINT('Ctrl Pts',(-0.130227956640556,0.0276173752808998,
4.));
#29148=CARTESIAN_POINT('Ctrl Pts',(-0.129158656751422,0.030959813881302,
4.));
#29149=CARTESIAN_POINT('Ctrl Pts',(-0.12796229886657,0.0342658696738965,
4.));
#29150=CARTESIAN_POINT('Ctrl Pts',(-0.126644858507038,0.0375136883583919,
4.));
#29151=CARTESIAN_POINT('Ctrl Pts',(-0.124572648602295,0.042622201998594,
4.));
#29152=CARTESIAN_POINT('Ctrl Pts',(-0.122198572282107,0.0475953519381505,
4.));
#29153=CARTESIAN_POINT('Ctrl Pts',(-0.119526530046339,0.0523977893098404,
4.));
#29154=CARTESIAN_POINT('Ctrl Pts',(-0.116935312520942,0.0570549611597328,
4.));
#29155=CARTESIAN_POINT('Ctrl Pts',(-0.11406058633243,0.0615550019486321,
4.));
#29156=CARTESIAN_POINT('Ctrl Pts',(-0.11092106856286,0.0658392337664117,
4.));
#29157=CARTESIAN_POINT('Ctrl Pts',(-0.10710607669906,0.071045227402084,
4.));
#29158=CARTESIAN_POINT('Ctrl Pts',(-0.102897192277319,0.075940267594365,
4.));
#29159=CARTESIAN_POINT('Ctrl Pts',(-0.0982968852906839,0.0804596595786888,
4.));
#29160=CARTESIAN_POINT('Ctrl Pts',(-0.0975398380300018,0.0812033911017416,
4.));
#29161=CARTESIAN_POINT('Ctrl Pts',(-0.0967721750025885,0.0819369232370377,
4.));
#29162=CARTESIAN_POINT('Ctrl Pts',(-0.0959941513168557,0.0826601513985347,
4.));
#29163=CARTESIAN_POINT('Origin',(0.,0.,3.7));
#29164=CARTESIAN_POINT('Origin',(0.,0.,3.4));
#29165=CARTESIAN_POINT('Origin',(1.,0.,3.8));
#29166=CARTESIAN_POINT('',(0.8,2.44929359829471E-17,4.));
#29167=CARTESIAN_POINT('Origin',(1.,0.,4.));
#29168=CARTESIAN_POINT('',(0.8,2.44929359829471E-17,3.6));
#29169=CARTESIAN_POINT('',(0.8,2.44929359829471E-17,3.8));
#29170=CARTESIAN_POINT('Origin',(1.,0.,3.6));
#29171=CARTESIAN_POINT('Origin',(1.4,-0.6,3.6));
#29172=CARTESIAN_POINT('',(1.4,-0.6,3.6));
#29173=CARTESIAN_POINT('',(1.4,0.6,3.6));
#29174=CARTESIAN_POINT('',(1.4,-0.6,3.6));
#29175=CARTESIAN_POINT('',(1.4,0.6,4.));
#29176=CARTESIAN_POINT('',(1.4,0.6,3.6));
#29177=CARTESIAN_POINT('',(1.4,-0.6,4.));
#29178=CARTESIAN_POINT('',(1.4,-0.6,4.));
#29179=CARTESIAN_POINT('',(1.4,-0.6,3.6));
#29180=CARTESIAN_POINT('Origin',(0.7,0.,3.6));
#29181=CARTESIAN_POINT('',(0.4,0.6,3.6));
#29182=CARTESIAN_POINT('',(0.4,-0.6,3.6));
#29183=CARTESIAN_POINT('',(0.4,-0.3,3.6));
#29184=CARTESIAN_POINT('',(1.4,0.6,3.6));
#29185=CARTESIAN_POINT('',(0.,-0.6,3.6));
#29186=CARTESIAN_POINT('Origin',(0.4,0.6,2.6));
#29187=CARTESIAN_POINT('',(-0.4,0.6,4.));
#29188=CARTESIAN_POINT('',(0.4,0.6,4.));
#29189=CARTESIAN_POINT('',(0.4,0.6,2.6));
#29190=CARTESIAN_POINT('',(0.4,0.6,2.6));
#29191=CARTESIAN_POINT('',(-0.4,0.6,2.6));
#29192=CARTESIAN_POINT('',(0.4,0.6,2.6));
#29193=CARTESIAN_POINT('',(-0.4,0.6,2.6));
#29194=CARTESIAN_POINT('Origin',(0.4,-0.6,2.6));
#29195=CARTESIAN_POINT('',(0.4,-0.6,2.6));
#29196=CARTESIAN_POINT('',(0.4,-0.6,2.6));
#29197=CARTESIAN_POINT('',(0.4,-0.6,2.6));
#29198=CARTESIAN_POINT('Origin',(-0.4,-0.6,2.6));
#29199=CARTESIAN_POINT('',(-0.4,-0.6,4.));
#29200=CARTESIAN_POINT('',(-0.4,-0.6,4.));
#29201=CARTESIAN_POINT('',(-0.4,-0.6,2.6));
#29202=CARTESIAN_POINT('',(-0.4,-0.6,2.6));
#29203=CARTESIAN_POINT('',(-0.4,-0.6,2.6));
#29204=CARTESIAN_POINT('Origin',(-0.4,0.6,2.6));
#29205=CARTESIAN_POINT('',(-0.4,0.6,2.6));
#29206=CARTESIAN_POINT('',(-0.4,0.6,4.));
#29207=CARTESIAN_POINT('Origin',(0.,0.,4.));
#29208=CARTESIAN_POINT('Origin',(0.,0.,2.6));
#29209=CARTESIAN_POINT('',(0.,0.,0.));
#29210=CARTESIAN_POINT('Origin',(0.,0.,4.1));
#29211=CARTESIAN_POINT('',(-0.2,2.44929359829471E-17,4.2));
#29212=CARTESIAN_POINT('Origin',(0.,0.,4.2));
#29213=CARTESIAN_POINT('',(-0.2,2.44929359829471E-17,4.));
#29214=CARTESIAN_POINT('',(-0.2,2.44929359829471E-17,4.1));
#29215=CARTESIAN_POINT('Origin',(0.,0.,4.));
#29216=CARTESIAN_POINT('Origin',(0.4,0.4,4.));
#29217=CARTESIAN_POINT('',(0.4,0.4,4.));
#29218=CARTESIAN_POINT('',(-0.4,0.4,4.));
#29219=CARTESIAN_POINT('',(0.4,0.4,4.));
#29220=CARTESIAN_POINT('',(-0.4,0.4,4.2));
#29221=CARTESIAN_POINT('',(-0.4,0.4,4.));
#29222=CARTESIAN_POINT('',(0.4,0.4,4.2));
#29223=CARTESIAN_POINT('',(0.4,0.4,4.2));
#29224=CARTESIAN_POINT('',(0.4,0.4,4.));
#29225=CARTESIAN_POINT('Origin',(0.4,-0.4,4.));
#29226=CARTESIAN_POINT('',(0.4,-0.4,4.));
#29227=CARTESIAN_POINT('',(0.4,-0.4,4.));
#29228=CARTESIAN_POINT('',(0.4,-0.4,4.2));
#29229=CARTESIAN_POINT('',(0.4,-0.4,4.2));
#29230=CARTESIAN_POINT('',(0.4,-0.4,4.));
#29231=CARTESIAN_POINT('Origin',(-0.4,-0.4,4.));
#29232=CARTESIAN_POINT('',(-0.4,-0.4,4.));
#29233=CARTESIAN_POINT('',(-0.4,-0.4,4.));
#29234=CARTESIAN_POINT('',(-0.4,-0.4,4.2));
#29235=CARTESIAN_POINT('',(-0.4,-0.4,4.2));
#29236=CARTESIAN_POINT('',(-0.4,-0.4,4.));
#29237=CARTESIAN_POINT('Origin',(-0.4,0.4,4.));
#29238=CARTESIAN_POINT('',(-0.4,0.4,4.));
#29239=CARTESIAN_POINT('',(-0.4,0.4,4.2));
#29240=CARTESIAN_POINT('Origin',(0.,0.,4.2));
#29241=CARTESIAN_POINT('Origin',(0.,0.,4.));
#29242=CARTESIAN_POINT('',(0.,0.,0.));
#29243=CARTESIAN_POINT('Origin',(0.,0.,0.));
#29244=CARTESIAN_POINT('',(-0.2,-2.44929359829471E-17,1.));
#29245=CARTESIAN_POINT('Origin',(0.,0.,1.));
#29246=CARTESIAN_POINT('',(-0.2,-2.44929359829471E-17,0.));
#29247=CARTESIAN_POINT('',(-0.2,-2.44929359829471E-17,0.));
#29248=CARTESIAN_POINT('Origin',(0.,0.,0.));
#29249=CARTESIAN_POINT('Origin',(0.,0.,0.));
#29250=CARTESIAN_POINT('',(-0.3,-3.67394039744206E-17,1.));
#29251=CARTESIAN_POINT('Origin',(0.,0.,1.));
#29252=CARTESIAN_POINT('',(-0.3,-3.67394039744206E-17,0.));
#29253=CARTESIAN_POINT('',(-0.3,-3.67394039744206E-17,0.));
#29254=CARTESIAN_POINT('Origin',(0.,0.,0.));
#29255=CARTESIAN_POINT('Origin',(0.,0.,1.));
#29256=CARTESIAN_POINT('Origin',(0.,0.,0.));
#29257=CARTESIAN_POINT('',(0.,0.,0.));
#29258=CARTESIAN_POINT('Origin',(0.,0.,2.15));
#29259=CARTESIAN_POINT('',(-0.15,-1.83697019872103E-17,2.1));
#29260=CARTESIAN_POINT('Origin',(0.,0.,2.1));
#29261=CARTESIAN_POINT('',(-0.15,-1.83697019872103E-17,2.2));
#29262=CARTESIAN_POINT('',(-0.15,-1.83697019872103E-17,2.15));
#29263=CARTESIAN_POINT('Origin',(0.,0.,2.2));
#29264=CARTESIAN_POINT('Origin',(0.55,0.,2.1));
#29265=CARTESIAN_POINT('',(-0.2,2.44929359829471E-17,2.1));
#29266=CARTESIAN_POINT('Origin',(0.,0.,2.1));
#29267=CARTESIAN_POINT('Origin',(0.15,0.,2.2));
#29268=CARTESIAN_POINT('',(-0.2,-2.44929359829471E-17,2.2));
#29269=CARTESIAN_POINT('Origin',(0.,0.,2.2));
#29270=CARTESIAN_POINT('Origin',(0.,0.,0.));
#29271=CARTESIAN_POINT('',(-0.2,-2.44929359829471E-17,2.3));
#29272=CARTESIAN_POINT('Origin',(0.,0.,2.3));
#29273=CARTESIAN_POINT('',(-0.2,-2.44929359829471E-17,0.));
#29274=CARTESIAN_POINT('Origin',(0.,0.,0.));
#29275=CARTESIAN_POINT('',(-0.4,-4.89858719658941E-17,0.));
#29276=CARTESIAN_POINT('Origin',(0.,0.,0.));
#29277=CARTESIAN_POINT('',(-0.2,-2.44929359829471E-17,0.));
#29278=CARTESIAN_POINT('Origin',(0.,0.,0.));
#29279=CARTESIAN_POINT('Origin',(0.,0.,-0.2));
#29280=CARTESIAN_POINT('',(-0.4,-4.89858719658941E-17,-0.2));
#29281=CARTESIAN_POINT('',(-0.4,-4.89858719658941E-17,-0.2));
#29282=CARTESIAN_POINT('Origin',(0.,0.,-0.2));
#29283=CARTESIAN_POINT('Origin',(0.,0.,-0.2));
#29284=CARTESIAN_POINT('Origin',(0.,0.,0.));
#29285=CARTESIAN_POINT('',(-0.2,-2.44929359829471E-17,0.));
#29286=CARTESIAN_POINT('Origin',(0.,0.,2.3));
#29287=CARTESIAN_POINT('',(0.,0.,0.));
#29288=CARTESIAN_POINT('Origin',(-0.1,0.,0.1));
#29289=CARTESIAN_POINT('',(-0.1,0.111803398874989,0.));
#29290=CARTESIAN_POINT('',(-0.1,0.111803398874989,0.1));
#29291=CARTESIAN_POINT('',(-0.1,0.111803398874989,0.));
#29292=CARTESIAN_POINT('',(-0.1,0.335410196624968,0.));
#29293=CARTESIAN_POINT('',(-0.1,0.,0.));
#29294=CARTESIAN_POINT('',(-0.1,0.335410196624968,0.1));
#29295=CARTESIAN_POINT('',(-0.1,0.335410196624968,0.));
#29296=CARTESIAN_POINT('',(-0.1,0.,0.1));
#29297=CARTESIAN_POINT('Origin',(0.1,0.7,0.1));
#29298=CARTESIAN_POINT('',(0.1,0.111803398874989,0.1));
#29299=CARTESIAN_POINT('',(0.1,0.111803398874989,0.));
#29300=CARTESIAN_POINT('',(0.1,0.111803398874989,0.));
#29301=CARTESIAN_POINT('',(0.1,0.335410196624968,0.1));
#29302=CARTESIAN_POINT('',(0.1,0.35,0.1));
#29303=CARTESIAN_POINT('',(0.1,0.335410196624968,0.));
#29304=CARTESIAN_POINT('',(0.1,0.335410196624968,0.));
#29305=CARTESIAN_POINT('',(0.1,0.35,0.));
#29306=CARTESIAN_POINT('Origin',(0.,0.,0.));
#29307=CARTESIAN_POINT('Origin',(0.,0.,0.));
#29308=CARTESIAN_POINT('Origin',(0.,0.,0.));
#29309=CARTESIAN_POINT('Origin',(0.,0.,0.));
#29310=CARTESIAN_POINT('Origin',(0.,0.,0.1));
#29311=CARTESIAN_POINT('Origin',(0.,0.,0.));
#29312=CARTESIAN_POINT('Origin',(0.,0.,0.1));
#29313=CARTESIAN_POINT('Origin',(0.,0.,0.1));
#29314=CARTESIAN_POINT('',(0.,0.,0.));
#29315=CARTESIAN_POINT('Ctrl Pts',(0.6,-1.22464679914735E-17,0.));
#29316=CARTESIAN_POINT('Ctrl Pts',(0.6,0.0128205128205128,-0.0966643893412244));
#29317=CARTESIAN_POINT('Ctrl Pts',(0.552422075024677,0.0384615384615385,
-0.289907779312461));
#29318=CARTESIAN_POINT('Ctrl Pts',(0.354387423761003,0.0769230769230769,
-0.513439446520879));
#29319=CARTESIAN_POINT('Ctrl Pts',(0.0752027553952744,0.115384615384615,
-0.619312950390957));
#29320=CARTESIAN_POINT('Ctrl Pts',(-0.221227750860346,0.153846153846154,
-0.583326335743102));
#29321=CARTESIAN_POINT('Ctrl Pts',(-0.466969125257516,0.192307692307692,
-0.413698471057249));
#29322=CARTESIAN_POINT('Ctrl Pts',(-0.605737625154647,0.230769230769231,
-0.149301246402526));
#29323=CARTESIAN_POINT('Ctrl Pts',(-0.605736940333524,0.269230769230769,
0.14930101675222));
#29324=CARTESIAN_POINT('Ctrl Pts',(-0.466970187413293,0.307692307692308,
0.413699286558057));
#29325=CARTESIAN_POINT('Ctrl Pts',(-0.221225725123394,0.346153846153846,
0.583324484886018));
#29326=CARTESIAN_POINT('Ctrl Pts',(0.0751986583056162,0.384615384615385,
0.619316856641734));
#29327=CARTESIAN_POINT('Ctrl Pts',(0.354396045955746,0.423076923076923,
0.513431304005641));
#29328=CARTESIAN_POINT('Ctrl Pts',(0.55240551470084,0.461538461538462,0.289924779022985));
#29329=CARTESIAN_POINT('Ctrl Pts',(0.623865568763842,0.5,3.99584594159288E-16));
#29330=CARTESIAN_POINT('Ctrl Pts',(0.552405514700841,0.538461538461539,
-0.289924779022984));
#29331=CARTESIAN_POINT('Ctrl Pts',(0.354396045955747,0.576923076923077,
-0.513431304005641));
#29332=CARTESIAN_POINT('Ctrl Pts',(0.0751986583056171,0.615384615384616,
-0.619316856641735));
#29333=CARTESIAN_POINT('Ctrl Pts',(-0.221225725123393,0.653846153846154,
-0.583324484886017));
#29334=CARTESIAN_POINT('Ctrl Pts',(-0.466970187413293,0.692307692307693,
-0.413699286558058));
#29335=CARTESIAN_POINT('Ctrl Pts',(-0.605736940333523,0.730769230769231,
-0.149301016752221));
#29336=CARTESIAN_POINT('Ctrl Pts',(-0.605737625154647,0.769230769230769,
0.149301246402525));
#29337=CARTESIAN_POINT('Ctrl Pts',(-0.466969125257516,0.807692307692308,
0.41369847105725));
#29338=CARTESIAN_POINT('Ctrl Pts',(-0.221227750860347,0.846153846153846,
0.583326335743102));
#29339=CARTESIAN_POINT('Ctrl Pts',(0.0752027553952735,0.884615384615385,
0.619312950390957));
#29340=CARTESIAN_POINT('Ctrl Pts',(0.354387423761003,0.923076923076923,
0.513439446520879));
#29341=CARTESIAN_POINT('Ctrl Pts',(0.552422075024676,0.961538461538462,
0.289907779312462));
#29342=CARTESIAN_POINT('Ctrl Pts',(0.6,0.987179487179487,0.096664389341225));
#29343=CARTESIAN_POINT('Ctrl Pts',(0.6,1.,2.93915231795365E-16));
#29344=CARTESIAN_POINT('Ctrl Pts',(0.6,-0.0299199300341885,0.));
#29345=CARTESIAN_POINT('Ctrl Pts',(0.6,-0.0170994172136757,-0.09670823080664));
#29346=CARTESIAN_POINT('Ctrl Pts',(0.552433668035603,0.00854160842734991,
-0.289889597147613));
#29347=CARTESIAN_POINT('Ctrl Pts',(0.354391049739123,0.0470031468888885,
-0.513458052176708));
#29348=CARTESIAN_POINT('Ctrl Pts',(0.0752046939357531,0.0854646853504268,
-0.619317061421753));
#29349=CARTESIAN_POINT('Ctrl Pts',(-0.221231470738224,0.123926223811965,
-0.583337632633336));
#29350=CARTESIAN_POINT('Ctrl Pts',(-0.466975962510102,0.162387762273504,
-0.413703477287484));
#29351=CARTESIAN_POINT('Ctrl Pts',(-0.605746831003298,0.200849300735043,
-0.149304082326356));
#29352=CARTESIAN_POINT('Ctrl Pts',(-0.605746010438017,0.239310839196581,
0.149303548319889));
#29353=CARTESIAN_POINT('Ctrl Pts',(-0.466977235204714,0.277772377658119,
0.413705373558643));
#29354=CARTESIAN_POINT('Ctrl Pts',(-0.221229043462903,0.316233916119658,
0.58333332852287));
#29355=CARTESIAN_POINT('Ctrl Pts',(0.0751997847274774,0.354695454581196,
0.619326143478273));
#29356=CARTESIAN_POINT('Ctrl Pts',(0.35440138101164,0.393156993042734,0.513439044221362));
#29357=CARTESIAN_POINT('Ctrl Pts',(0.552413825150628,0.431618531504273,
0.289929135658685));
#29358=CARTESIAN_POINT('Ctrl Pts',(0.623874957033007,0.470080069965812,
3.99584594159288E-16));
#29359=CARTESIAN_POINT('Ctrl Pts',(0.552413825150628,0.50854160842735,-0.289929135658685));
#29360=CARTESIAN_POINT('Ctrl Pts',(0.354401381011641,0.547003146888889,
-0.513439044221361));
#29361=CARTESIAN_POINT('Ctrl Pts',(0.0751997847274784,0.585464685350427,
-0.619326143478273));
#29362=CARTESIAN_POINT('Ctrl Pts',(-0.221229043462903,0.623926223811966,
-0.583333328522871));
#29363=CARTESIAN_POINT('Ctrl Pts',(-0.466977235204713,0.662387762273504,
-0.413705373558643));
#29364=CARTESIAN_POINT('Ctrl Pts',(-0.605746010438017,0.700849300735043,
-0.14930354831989));
#29365=CARTESIAN_POINT('Ctrl Pts',(-0.605746831003298,0.73931083919658,
0.149304082326356));
#29366=CARTESIAN_POINT('Ctrl Pts',(-0.466975962510103,0.77777237765812,
0.413703477287484));
#29367=CARTESIAN_POINT('Ctrl Pts',(-0.221231470738224,0.816233916119658,
0.583337632633336));
#29368=CARTESIAN_POINT('Ctrl Pts',(0.0752046939357522,0.854695454581196,
0.619317061421752));
#29369=CARTESIAN_POINT('Ctrl Pts',(0.354391049739122,0.893156993042734,
0.513458052176709));
#29370=CARTESIAN_POINT('Ctrl Pts',(0.552433668035603,0.931618531504273,
0.289889597147614));
#29371=CARTESIAN_POINT('Ctrl Pts',(0.6,0.957259557145299,0.0967082308066405));
#29372=CARTESIAN_POINT('Ctrl Pts',(0.6,0.970080069965812,2.93915231795365E-16));
#29373=CARTESIAN_POINT('Ctrl Pts',(0.57140278473399,-0.0895099491231781,
0.));
#29374=CARTESIAN_POINT('Ctrl Pts',(0.57140278473399,-0.0766894363026653,
-0.0920388134316465));
#29375=CARTESIAN_POINT('Ctrl Pts',(0.526087666325587,-0.0510484106616395,
-0.27609779977643));
#29376=CARTESIAN_POINT('Ctrl Pts',(0.337495083246531,-0.0125868722001011,
-0.488960092834314));
#29377=CARTESIAN_POINT('Ctrl Pts',(0.071617628135789,0.0258746662614374,
-0.589793519606227));
#29378=CARTESIAN_POINT('Ctrl Pts',(-0.210682030750213,0.064336204722976,
-0.555519091361673));
#29379=CARTESIAN_POINT('Ctrl Pts',(-0.444709568341539,0.102797743184514,
-0.393978668020424));
#29380=CARTESIAN_POINT('Ctrl Pts',(-0.57686308879389,0.141259281646053,
-0.142184059267368));
#29381=CARTESIAN_POINT('Ctrl Pts',(-0.576862493445414,0.179720820107591,
0.142183967988976));
#29382=CARTESIAN_POINT('Ctrl Pts',(-0.444710491725475,0.21818235856913,
0.39397899216129));
#29383=CARTESIAN_POINT('Ctrl Pts',(-0.21068026967806,0.256643897030668,
0.555518355836033));
#29384=CARTESIAN_POINT('Ctrl Pts',(0.0716140663354809,0.295105435492207,
0.589795072696736));
#29385=CARTESIAN_POINT('Ctrl Pts',(0.337502578941879,0.333566973953745,
0.488956887495931));
#29386=CARTESIAN_POINT('Ctrl Pts',(0.526073269626597,0.372028512415283,
0.276104552814102));
#29387=CARTESIAN_POINT('Ctrl Pts',(0.59412694151864,0.410490050876822,3.42501080707961E-16));
#29388=CARTESIAN_POINT('Ctrl Pts',(0.526073269626597,0.448951589338361,
-0.276104552814101));
#29389=CARTESIAN_POINT('Ctrl Pts',(0.33750257894188,0.487413127799899,-0.488956887495931));
#29390=CARTESIAN_POINT('Ctrl Pts',(0.0716140663354816,0.525874666261437,
-0.589795072696736));
#29391=CARTESIAN_POINT('Ctrl Pts',(-0.21068026967806,0.564336204722976,
-0.555518355836033));
#29392=CARTESIAN_POINT('Ctrl Pts',(-0.444710491725474,0.602797743184515,
-0.393978992161291));
#29393=CARTESIAN_POINT('Ctrl Pts',(-0.576862493445414,0.641259281646054,
-0.142183967988976));
#29394=CARTESIAN_POINT('Ctrl Pts',(-0.576863088793891,0.679720820107591,
0.142184059267367));
#29395=CARTESIAN_POINT('Ctrl Pts',(-0.44470956834154,0.718182358569131,
0.393978668020424));
#29396=CARTESIAN_POINT('Ctrl Pts',(-0.210682030750213,0.756643897030668,
0.555519091361672));
#29397=CARTESIAN_POINT('Ctrl Pts',(0.0716176281357881,0.795105435492208,
0.589793519606227));
#29398=CARTESIAN_POINT('Ctrl Pts',(0.33749508324653,0.833566973953744,0.488960092834314));
#29399=CARTESIAN_POINT('Ctrl Pts',(0.526087666325587,0.872028512415284,
0.276097799776431));
#29400=CARTESIAN_POINT('Ctrl Pts',(0.57140278473399,0.89766953805631,0.092038813431647));
#29401=CARTESIAN_POINT('Ctrl Pts',(0.57140278473399,0.910490050876822,2.79906636539346E-16));
#29402=CARTESIAN_POINT('Ctrl Pts',(0.474553946216323,-0.111561765583155,
0.));
#29403=CARTESIAN_POINT('Ctrl Pts',(0.474553946216323,-0.0987412527626418,
-0.0764564796257483));
#29404=CARTESIAN_POINT('Ctrl Pts',(0.436924085441389,-0.0731002271216164,
-0.229293819423993));
#29405=CARTESIAN_POINT('Ctrl Pts',(0.28029344651323,-0.0346386886600778,
-0.406092197111352));
#29406=CARTESIAN_POINT('Ctrl Pts',(0.0594797119051372,0.00382284980146056,
-0.489829229563544));
#29407=CARTESIAN_POINT('Ctrl Pts',(-0.174974371163627,0.0422843882629991,
-0.461366967583472));
#29408=CARTESIAN_POINT('Ctrl Pts',(-0.369337104437002,0.0807459267245375,
-0.327204006955578));
#29409=CARTESIAN_POINT('Ctrl Pts',(-0.479092464392592,0.119207465186076,
-0.118085979220413));
#29410=CARTESIAN_POINT('Ctrl Pts',(-0.479091915422023,0.157669003647615,
0.118085781150671));
#29411=CARTESIAN_POINT('Ctrl Pts',(-0.369337955888923,0.196130542109153,
0.327204710311264));
#29412=CARTESIAN_POINT('Ctrl Pts',(-0.17497274727977,0.234592080570691,
0.461365371232019));
#29413=CARTESIAN_POINT('Ctrl Pts',(0.0594764275706395,0.27305361903223,
0.489832598580241));
#29414=CARTESIAN_POINT('Ctrl Pts',(0.280300358290614,0.311515157493768,
0.406085170317839));
#29415=CARTESIAN_POINT('Ctrl Pts',(0.436910810251582,0.349976695955307,
0.229308481892446));
#29416=CARTESIAN_POINT('Ctrl Pts',(0.493430286203431,0.388438234416845,
3.28230202345129E-16));
#29417=CARTESIAN_POINT('Ctrl Pts',(0.436910810251583,0.426899772878384,
-0.229308481892445));
#29418=CARTESIAN_POINT('Ctrl Pts',(0.280300358290614,0.465361311339922,
-0.406085170317838));
#29419=CARTESIAN_POINT('Ctrl Pts',(0.0594764275706403,0.503822849801461,
-0.489832598580241));
#29420=CARTESIAN_POINT('Ctrl Pts',(-0.17497274727977,0.542284388262999,
-0.461365371232019));
#29421=CARTESIAN_POINT('Ctrl Pts',(-0.369337955888923,0.580745926724537,
-0.327204710311264));
#29422=CARTESIAN_POINT('Ctrl Pts',(-0.479091915422023,0.619207465186076,
-0.118085781150672));
#29423=CARTESIAN_POINT('Ctrl Pts',(-0.479092464392592,0.657669003647615,
0.118085979220413));
#29424=CARTESIAN_POINT('Ctrl Pts',(-0.369337104437003,0.696130542109153,
0.327204006955579));
#29425=CARTESIAN_POINT('Ctrl Pts',(-0.174974371163627,0.734592080570691,
0.461366967583471));
#29426=CARTESIAN_POINT('Ctrl Pts',(0.0594797119051365,0.773053619032229,
0.489829229563544));
#29427=CARTESIAN_POINT('Ctrl Pts',(0.280293446513229,0.811515157493768,
0.406092197111352));
#29428=CARTESIAN_POINT('Ctrl Pts',(0.436924085441388,0.849976695955308,
0.229293819423994));
#29429=CARTESIAN_POINT('Ctrl Pts',(0.474553946216323,0.875617721596332,
0.0764564796257487));
#29430=CARTESIAN_POINT('Ctrl Pts',(0.474553946216323,0.888438234416845,
2.32464388502626E-16));
#29431=CARTESIAN_POINT('Ctrl Pts',(0.396775149169774,-0.0496835058675068,
0.));
#29432=CARTESIAN_POINT('Ctrl Pts',(0.396775149169774,-0.036862993046994,
-0.0639325270983766));
#29433=CARTESIAN_POINT('Ctrl Pts',(0.365314671027668,-0.0112219674059683,
-0.19170987675844));
#29434=CARTESIAN_POINT('Ctrl Pts',(0.23435429480531,0.0272395710555702,
-0.339537237215488));
#29435=CARTESIAN_POINT('Ctrl Pts',(0.0497313786444746,0.0657011095171087,
-0.409547504928549));
#29436=CARTESIAN_POINT('Ctrl Pts',(-0.146296899267444,0.104162647978647,
-0.385751347000212));
#29437=CARTESIAN_POINT('Ctrl Pts',(-0.308804333876165,0.142624186440185,
-0.273576498871778));
#29438=CARTESIAN_POINT('Ctrl Pts',(-0.400571315183775,0.181085724901724,
-0.0987322989296554));
#29439=CARTESIAN_POINT('Ctrl Pts',(-0.400570833992816,0.219547263363262,
0.098732083557009));
#29440=CARTESIAN_POINT('Ctrl Pts',(-0.308805080202088,0.258008801824801,
0.273577263668698));
#29441=CARTESIAN_POINT('Ctrl Pts',(-0.146295475879243,0.296470340286339,
0.385749611149152));
#29442=CARTESIAN_POINT('Ctrl Pts',(0.0497284998160722,0.334931878747878,
0.409551168080821));
#29443=CARTESIAN_POINT('Ctrl Pts',(0.234360353208027,0.373393417209416,
0.339529585460424));
#29444=CARTESIAN_POINT('Ctrl Pts',(0.365303034882358,0.411854955670955,
0.19172582146083));
#29445=CARTESIAN_POINT('Ctrl Pts',(0.412559215796984,0.450316494132494,
2.28334053805307E-16));
#29446=CARTESIAN_POINT('Ctrl Pts',(0.365303034882358,0.488778032594032,
-0.191725821460829));
#29447=CARTESIAN_POINT('Ctrl Pts',(0.234360353208027,0.52723957105557,-0.339529585460423));
#29448=CARTESIAN_POINT('Ctrl Pts',(0.049728499816073,0.565701109517109,
-0.409551168080821));
#29449=CARTESIAN_POINT('Ctrl Pts',(-0.146295475879243,0.604162647978647,
-0.385749611149151));
#29450=CARTESIAN_POINT('Ctrl Pts',(-0.308805080202087,0.642624186440186,
-0.273577263668699));
#29451=CARTESIAN_POINT('Ctrl Pts',(-0.400570833992816,0.681085724901724,
-0.0987320835570092));
#29452=CARTESIAN_POINT('Ctrl Pts',(-0.400571315183774,0.719547263363262,
0.0987322989296545));
#29453=CARTESIAN_POINT('Ctrl Pts',(-0.308804333876166,0.758008801824802,
0.273576498871779));
#29454=CARTESIAN_POINT('Ctrl Pts',(-0.146296899267444,0.79647034028634,
0.385751347000211));
#29455=CARTESIAN_POINT('Ctrl Pts',(0.0497313786444738,0.834931878747878,
0.409547504928549));
#29456=CARTESIAN_POINT('Ctrl Pts',(0.234354294805309,0.873393417209416,
0.339537237215489));
#29457=CARTESIAN_POINT('Ctrl Pts',(0.365314671027668,0.911854955670954,
0.191709876758441));
#29458=CARTESIAN_POINT('Ctrl Pts',(0.396775149169774,0.937495981311981,
0.0639325270983769));
#29459=CARTESIAN_POINT('Ctrl Pts',(0.396775149169774,0.950316494132494,
1.94363766564791E-16));
#29460=CARTESIAN_POINT('Ctrl Pts',(0.396939270424005,0.0496169828764393,
0.));
#29461=CARTESIAN_POINT('Ctrl Pts',(0.396939270424005,0.0624374956969522,
-0.0639374232798038));
#29462=CARTESIAN_POINT('Ctrl Pts',(0.36546008089603,0.0880785213379777,
-0.191798112042878));
#29463=CARTESIAN_POINT('Ctrl Pts',(0.234449450409805,0.126540059799516,
-0.339668537739251));
#29464=CARTESIAN_POINT('Ctrl Pts',(0.049750996607657,0.165001598261055,
-0.409714888680431));
#29465=CARTESIAN_POINT('Ctrl Pts',(-0.146355584839357,0.203463136722593,
-0.385905355800823));
#29466=CARTESIAN_POINT('Ctrl Pts',(-0.308928706451725,0.241924675184131,
-0.273687199853259));
#29467=CARTESIAN_POINT('Ctrl Pts',(-0.400732481863726,0.28038621364567,
-0.0987717444550605));
#29468=CARTESIAN_POINT('Ctrl Pts',(-0.400732067194017,0.318847752107208,
0.0987716785889419));
#29469=CARTESIAN_POINT('Ctrl Pts',(-0.308929349603364,0.357309290568747,
0.273687433751705));
#29470=CARTESIAN_POINT('Ctrl Pts',(-0.146354358224513,0.395770829030285,
0.385904825042549));
#29471=CARTESIAN_POINT('Ctrl Pts',(0.0497485157569321,0.434232367491824,
0.40971600936184));
#29472=CARTESIAN_POINT('Ctrl Pts',(0.234454671281171,0.472693905953362,
0.339666223345759));
#29473=CARTESIAN_POINT('Ctrl Pts',(0.365450053365557,0.511155444414901,
0.191802985182395));
#29474=CARTESIAN_POINT('Ctrl Pts',(0.412725251465001,0.549616982876439,
3.13959323982298E-16));
#29475=CARTESIAN_POINT('Ctrl Pts',(0.365450053365557,0.588078521337977,
-0.191802985182395));
#29476=CARTESIAN_POINT('Ctrl Pts',(0.234454671281172,0.626540059799516,
-0.339666223345758));
#29477=CARTESIAN_POINT('Ctrl Pts',(0.0497485157569325,0.665001598261056,
-0.409716009361841));
#29478=CARTESIAN_POINT('Ctrl Pts',(-0.146354358224513,0.703463136722593,
-0.385904825042548));
#29479=CARTESIAN_POINT('Ctrl Pts',(-0.308929349603364,0.741924675184131,
-0.273687433751706));
#29480=CARTESIAN_POINT('Ctrl Pts',(-0.400732067194016,0.78038621364567,
-0.0987716785889423));
#29481=CARTESIAN_POINT('Ctrl Pts',(-0.400732481863727,0.818847752107209,
0.09877174445506));
#29482=CARTESIAN_POINT('Ctrl Pts',(-0.308928706451726,0.857309290568746,
0.273687199853259));
#29483=CARTESIAN_POINT('Ctrl Pts',(-0.146355584839357,0.895770829030286,
0.385905355800823));
#29484=CARTESIAN_POINT('Ctrl Pts',(0.0497509966076566,0.934232367491823,
0.409714888680431));
#29485=CARTESIAN_POINT('Ctrl Pts',(0.234449450409805,0.972693905953362,
0.339668537739251));
#29486=CARTESIAN_POINT('Ctrl Pts',(0.36546008089603,1.0111554444149,0.191798112042878));
#29487=CARTESIAN_POINT('Ctrl Pts',(0.396939270424005,1.03679647005593,0.0639374232798042));
#29488=CARTESIAN_POINT('Ctrl Pts',(0.396939270424005,1.04961698287644,1.94444162792257E-16));
#29489=CARTESIAN_POINT('Ctrl Pts',(0.474480121999477,0.111725197096412,
0.));
#29490=CARTESIAN_POINT('Ctrl Pts',(0.474480121999477,0.124545709916925,
-0.0764586335789696));
#29491=CARTESIAN_POINT('Ctrl Pts',(0.436859829833703,0.150186735557951,
-0.229252323181468));
#29492=CARTESIAN_POINT('Ctrl Pts',(0.28025100438353,0.188648274019489,-0.406034984914813));
#29493=CARTESIAN_POINT('Ctrl Pts',(0.0594710800733114,0.227109812481028,
-0.489754346320688));
#29494=CARTESIAN_POINT('Ctrl Pts',(-0.174948343135337,0.265571350942566,
-0.461298814622112));
#29495=CARTESIAN_POINT('Ctrl Pts',(-0.369281839162736,0.304032889404105,
-0.327154709430175));
#29496=CARTESIAN_POINT('Ctrl Pts',(-0.479020883931678,0.342494427865643,
-0.118068517820842));
#29497=CARTESIAN_POINT('Ctrl Pts',(-0.47902029155056,0.380955966327182,
0.118068222258303));
#29498=CARTESIAN_POINT('Ctrl Pts',(-0.369282757944306,0.41941750478872,
0.327155758983302));
#29499=CARTESIAN_POINT('Ctrl Pts',(-0.17494659084079,0.457879043250258,
0.461296432432969));
#29500=CARTESIAN_POINT('Ctrl Pts',(0.0594675360258692,0.496340581711797,
0.489759373275717));
#29501=CARTESIAN_POINT('Ctrl Pts',(0.280258462718537,0.534802120173335,
0.406024477645537));
#29502=CARTESIAN_POINT('Ctrl Pts',(0.436845504891309,0.573263658634874,
0.22927420538536));
#29503=CARTESIAN_POINT('Ctrl Pts',(0.493356533724516,0.611725197096412,
3.99584594159288E-16));
#29504=CARTESIAN_POINT('Ctrl Pts',(0.43684550489131,0.650186735557951,-0.229274205385359));
#29505=CARTESIAN_POINT('Ctrl Pts',(0.280258462718538,0.688648274019488,
-0.406024477645536));
#29506=CARTESIAN_POINT('Ctrl Pts',(0.0594675360258697,0.727109812481028,
-0.489759373275717));
#29507=CARTESIAN_POINT('Ctrl Pts',(-0.174946590840789,0.765571350942565,
-0.461296432432969));
#29508=CARTESIAN_POINT('Ctrl Pts',(-0.369282757944306,0.804032889404106,
-0.327155758983302));
#29509=CARTESIAN_POINT('Ctrl Pts',(-0.47902029155056,0.842494427865642,
-0.118068222258304));
#29510=CARTESIAN_POINT('Ctrl Pts',(-0.479020883931677,0.880955966327181,
0.118068517820842));
#29511=CARTESIAN_POINT('Ctrl Pts',(-0.369281839162738,0.91941750478872,
0.327154709430175));
#29512=CARTESIAN_POINT('Ctrl Pts',(-0.174948343135337,0.957879043250258,
0.461298814622112));
#29513=CARTESIAN_POINT('Ctrl Pts',(0.0594710800733105,0.996340581711796,
0.489754346320688));
#29514=CARTESIAN_POINT('Ctrl Pts',(0.28025100438353,1.03480212017334,0.406034984914813));
#29515=CARTESIAN_POINT('Ctrl Pts',(0.436859829833702,1.07326365863487,0.229252323181468));
#29516=CARTESIAN_POINT('Ctrl Pts',(0.474480121999477,1.0989046842759,0.0764586335789701));
#29517=CARTESIAN_POINT('Ctrl Pts',(0.474480121999477,1.11172519709641,2.32428225066282E-16));
#29518=CARTESIAN_POINT('Ctrl Pts',(0.571396374369977,0.0893939875669938,
0.));
#29519=CARTESIAN_POINT('Ctrl Pts',(0.571396374369977,0.102214500387507,
-0.0920304506152003));
#29520=CARTESIAN_POINT('Ctrl Pts',(0.526079825991483,0.127855526028532,
-0.27609774238039));
#29521=CARTESIAN_POINT('Ctrl Pts',(0.337490690748289,0.166317064490071,
-0.488951496511335));
#29522=CARTESIAN_POINT('Ctrl Pts',(0.0716165005604001,0.204778602951609,
-0.589786215561319));
#29523=CARTESIAN_POINT('Ctrl Pts',(-0.210679045222389,0.243240141413148,
-0.555510970358107));
#29524=CARTESIAN_POINT('Ctrl Pts',(-0.444703436119133,0.281701679874686,
-0.393973411075695));
#29525=CARTESIAN_POINT('Ctrl Pts',(-0.576855077960488,0.320163218336225,
-0.142181989990421));
#29526=CARTESIAN_POINT('Ctrl Pts',(-0.576854505315029,0.358624756797763,
0.142181949601214));
#29527=CARTESIAN_POINT('Ctrl Pts',(-0.444704324290748,0.397086295259301,
0.393973554508792));
#29528=CARTESIAN_POINT('Ctrl Pts',(-0.210677351306959,0.43554783372084,
0.555510645023163));
#29529=CARTESIAN_POINT('Ctrl Pts',(0.0716130745857797,0.474009372182378,
0.589786903242894));
#29530=CARTESIAN_POINT('Ctrl Pts',(0.337497900602802,0.512470910643917,
0.48895010790376));
#29531=CARTESIAN_POINT('Ctrl Pts',(0.526065978296192,0.550932449105455,
0.276100726868827));
#29532=CARTESIAN_POINT('Ctrl Pts',(0.594118706507634,0.589393987566993,
4.28126350884951E-16));
#29533=CARTESIAN_POINT('Ctrl Pts',(0.526065978296193,0.627855526028533,
-0.276100726868826));
#29534=CARTESIAN_POINT('Ctrl Pts',(0.337497900602802,0.66631706449007,-0.48895010790376));
#29535=CARTESIAN_POINT('Ctrl Pts',(0.0716130745857805,0.70477860295161,
-0.589786903242894));
#29536=CARTESIAN_POINT('Ctrl Pts',(-0.210677351306959,0.743240141413148,
-0.555510645023163));
#29537=CARTESIAN_POINT('Ctrl Pts',(-0.444704324290748,0.781701679874686,
-0.393973554508792));
#29538=CARTESIAN_POINT('Ctrl Pts',(-0.576854505315029,0.820163218336225,
-0.142181949601214));
#29539=CARTESIAN_POINT('Ctrl Pts',(-0.576855077960488,0.858624756797763,
0.14218198999042));
#29540=CARTESIAN_POINT('Ctrl Pts',(-0.444703436119134,0.897086295259303,
0.393973411075695));
#29541=CARTESIAN_POINT('Ctrl Pts',(-0.210679045222389,0.935547833720839,
0.555510970358107));
#29542=CARTESIAN_POINT('Ctrl Pts',(0.0716165005603993,0.97400937218238,
0.589786215561319));
#29543=CARTESIAN_POINT('Ctrl Pts',(0.337490690748288,1.01247091064392,0.488951496511335));
#29544=CARTESIAN_POINT('Ctrl Pts',(0.526079825991483,1.05093244910546,0.27609774238039));
#29545=CARTESIAN_POINT('Ctrl Pts',(0.571396374369977,1.07657347474648,0.0920304506152009));
#29546=CARTESIAN_POINT('Ctrl Pts',(0.571396374369977,1.08939398756699,2.79903496366638E-16));
#29547=CARTESIAN_POINT('Ctrl Pts',(0.6,0.0299199300341885,0.));
#29548=CARTESIAN_POINT('Ctrl Pts',(0.6,0.0427404428547013,-0.0967139473831177));
#29549=CARTESIAN_POINT('Ctrl Pts',(0.552435179671515,0.068381468495727,
-0.289887226338725));
#29550=CARTESIAN_POINT('Ctrl Pts',(0.354391522537672,0.106843006957265,
-0.513460478205433));
#29551=CARTESIAN_POINT('Ctrl Pts',(0.0752049467059282,0.145304545418804,
-0.619317597467292));
#29552=CARTESIAN_POINT('Ctrl Pts',(-0.22123195578055,0.183766083880342,
-0.583339105657478));
#29553=CARTESIAN_POINT('Ctrl Pts',(-0.46697685403316,0.222227622341881,
-0.413704130059871));
#29554=CARTESIAN_POINT('Ctrl Pts',(-0.60574803137234,0.260689160803419,
-0.149304452108144));
#29555=CARTESIAN_POINT('Ctrl Pts',(-0.605747193107107,0.299150699264958,
0.149303878416068));
#29556=CARTESIAN_POINT('Ctrl Pts',(-0.466978154180352,0.337612237726497,
0.41370616725484));
#29557=CARTESIAN_POINT('Ctrl Pts',(-0.221229476147838,0.376073776188034,
0.58333448166239));
#29558=CARTESIAN_POINT('Ctrl Pts',(0.0751999316038799,0.414535314649573,
0.619327354407488));
#29559=CARTESIAN_POINT('Ctrl Pts',(0.354402076660262,0.452996853111111,
0.513440053483591));
#29560=CARTESIAN_POINT('Ctrl Pts',(0.552414908766819,0.49145839157265,0.28992970372914));
#29561=CARTESIAN_POINT('Ctrl Pts',(0.623876181188225,0.529919930034188,
3.71042837433625E-16));
#29562=CARTESIAN_POINT('Ctrl Pts',(0.552414908766819,0.568381468495727,
-0.289929703729139));
#29563=CARTESIAN_POINT('Ctrl Pts',(0.354402076660263,0.606843006957265,
-0.51344005348359));
#29564=CARTESIAN_POINT('Ctrl Pts',(0.0751999316038808,0.645304545418805,
-0.619327354407488));
#29565=CARTESIAN_POINT('Ctrl Pts',(-0.221229476147837,0.683766083880342,
-0.583334481662391));
#29566=CARTESIAN_POINT('Ctrl Pts',(-0.466978154180352,0.722227622341881,
-0.41370616725484));
#29567=CARTESIAN_POINT('Ctrl Pts',(-0.605747193107107,0.760689160803419,
-0.149303878416068));
#29568=CARTESIAN_POINT('Ctrl Pts',(-0.60574803137234,0.799150699264958,
0.149304452108143));
#29569=CARTESIAN_POINT('Ctrl Pts',(-0.466976854033161,0.837612237726496,
0.41370413005987));
#29570=CARTESIAN_POINT('Ctrl Pts',(-0.22123195578055,0.876073776188035,
0.583339105657478));
#29571=CARTESIAN_POINT('Ctrl Pts',(0.0752049467059273,0.914535314649573,
0.619317597467291));
#29572=CARTESIAN_POINT('Ctrl Pts',(0.354391522537671,0.952996853111112,
0.513460478205434));
#29573=CARTESIAN_POINT('Ctrl Pts',(0.552435179671515,0.99145839157265,0.289887226338726));
#29574=CARTESIAN_POINT('Ctrl Pts',(0.6,1.01709941721368,0.0967139473831183));
#29575=CARTESIAN_POINT('Ctrl Pts',(0.6,1.02991993003419,2.93915231795365E-16));
#29576=CARTESIAN_POINT('Ctrl Pts',(0.6,1.22464679914735E-17,0.));
#29577=CARTESIAN_POINT('Ctrl Pts',(0.6,0.0128205128205128,-0.0966643893412244));
#29578=CARTESIAN_POINT('Ctrl Pts',(0.552422075024677,0.0384615384615385,
-0.289907779312461));
#29579=CARTESIAN_POINT('Ctrl Pts',(0.354387423761003,0.076923076923077,
-0.513439446520879));
#29580=CARTESIAN_POINT('Ctrl Pts',(0.0752027553952744,0.115384615384615,
-0.619312950390957));
#29581=CARTESIAN_POINT('Ctrl Pts',(-0.221227750860346,0.153846153846154,
-0.583326335743102));
#29582=CARTESIAN_POINT('Ctrl Pts',(-0.466969125257516,0.192307692307692,
-0.413698471057249));
#29583=CARTESIAN_POINT('Ctrl Pts',(-0.605737625154647,0.230769230769231,
-0.149301246402526));
#29584=CARTESIAN_POINT('Ctrl Pts',(-0.605736940333524,0.269230769230769,
0.14930101675222));
#29585=CARTESIAN_POINT('Ctrl Pts',(-0.466970187413293,0.307692307692308,
0.413699286558057));
#29586=CARTESIAN_POINT('Ctrl Pts',(-0.221225725123394,0.346153846153846,
0.583324484886018));
#29587=CARTESIAN_POINT('Ctrl Pts',(0.0751986583056162,0.384615384615385,
0.619316856641734));
#29588=CARTESIAN_POINT('Ctrl Pts',(0.354396045955746,0.423076923076923,
0.513431304005641));
#29589=CARTESIAN_POINT('Ctrl Pts',(0.55240551470084,0.461538461538462,0.289924779022985));
#29590=CARTESIAN_POINT('Ctrl Pts',(0.623865568763842,0.5,3.99584594159288E-16));
#29591=CARTESIAN_POINT('Ctrl Pts',(0.552405514700841,0.538461538461539,
-0.289924779022984));
#29592=CARTESIAN_POINT('Ctrl Pts',(0.354396045955747,0.576923076923077,
-0.513431304005641));
#29593=CARTESIAN_POINT('Ctrl Pts',(0.0751986583056171,0.615384615384616,
-0.619316856641735));
#29594=CARTESIAN_POINT('Ctrl Pts',(-0.221225725123393,0.653846153846154,
-0.583324484886017));
#29595=CARTESIAN_POINT('Ctrl Pts',(-0.466970187413293,0.692307692307693,
-0.413699286558058));
#29596=CARTESIAN_POINT('Ctrl Pts',(-0.605736940333523,0.730769230769231,
-0.149301016752221));
#29597=CARTESIAN_POINT('Ctrl Pts',(-0.605737625154647,0.769230769230769,
0.149301246402525));
#29598=CARTESIAN_POINT('Ctrl Pts',(-0.466969125257516,0.807692307692308,
0.41369847105725));
#29599=CARTESIAN_POINT('Ctrl Pts',(-0.221227750860347,0.846153846153846,
0.583326335743102));
#29600=CARTESIAN_POINT('Ctrl Pts',(0.0752027553952735,0.884615384615385,
0.619312950390957));
#29601=CARTESIAN_POINT('Ctrl Pts',(0.354387423761003,0.923076923076923,
0.513439446520879));
#29602=CARTESIAN_POINT('Ctrl Pts',(0.552422075024676,0.961538461538462,
0.289907779312462));
#29603=CARTESIAN_POINT('Ctrl Pts',(0.6,0.987179487179487,0.096664389341225));
#29604=CARTESIAN_POINT('Ctrl Pts',(0.6,1.,2.93915231795365E-16));
#29605=CARTESIAN_POINT('',(0.6,-1.22464679914735E-17,0.));
#29606=CARTESIAN_POINT('Origin',(0.5,0.,0.));
#29607=CARTESIAN_POINT('',(0.6,1.,2.93915231795365E-16));
#29608=CARTESIAN_POINT('Ctrl Pts',(0.6,1.22464679914735E-17,0.));
#29609=CARTESIAN_POINT('Ctrl Pts',(0.6,0.0128205128205128,-0.0966643893412244));
#29610=CARTESIAN_POINT('Ctrl Pts',(0.552422075024677,0.0384615384615385,
-0.289907779312461));
#29611=CARTESIAN_POINT('Ctrl Pts',(0.354387423761003,0.076923076923077,
-0.513439446520879));
#29612=CARTESIAN_POINT('Ctrl Pts',(0.0752027553952744,0.115384615384615,
-0.619312950390957));
#29613=CARTESIAN_POINT('Ctrl Pts',(-0.221227750860346,0.153846153846154,
-0.583326335743102));
#29614=CARTESIAN_POINT('Ctrl Pts',(-0.466969125257516,0.192307692307692,
-0.413698471057249));
#29615=CARTESIAN_POINT('Ctrl Pts',(-0.605737625154647,0.230769230769231,
-0.149301246402526));
#29616=CARTESIAN_POINT('Ctrl Pts',(-0.605736940333524,0.269230769230769,
0.14930101675222));
#29617=CARTESIAN_POINT('Ctrl Pts',(-0.466970187413293,0.307692307692308,
0.413699286558057));
#29618=CARTESIAN_POINT('Ctrl Pts',(-0.221225725123394,0.346153846153846,
0.583324484886018));
#29619=CARTESIAN_POINT('Ctrl Pts',(0.0751986583056162,0.384615384615385,
0.619316856641734));
#29620=CARTESIAN_POINT('Ctrl Pts',(0.354396045955746,0.423076923076923,
0.513431304005641));
#29621=CARTESIAN_POINT('Ctrl Pts',(0.55240551470084,0.461538461538462,0.289924779022985));
#29622=CARTESIAN_POINT('Ctrl Pts',(0.623865568763842,0.5,3.99584594159288E-16));
#29623=CARTESIAN_POINT('Ctrl Pts',(0.552405514700841,0.538461538461539,
-0.289924779022984));
#29624=CARTESIAN_POINT('Ctrl Pts',(0.354396045955747,0.576923076923077,
-0.513431304005641));
#29625=CARTESIAN_POINT('Ctrl Pts',(0.0751986583056171,0.615384615384616,
-0.619316856641735));
#29626=CARTESIAN_POINT('Ctrl Pts',(-0.221225725123393,0.653846153846154,
-0.583324484886017));
#29627=CARTESIAN_POINT('Ctrl Pts',(-0.466970187413293,0.692307692307693,
-0.413699286558058));
#29628=CARTESIAN_POINT('Ctrl Pts',(-0.605736940333523,0.730769230769231,
-0.149301016752221));
#29629=CARTESIAN_POINT('Ctrl Pts',(-0.605737625154647,0.769230769230769,
0.149301246402525));
#29630=CARTESIAN_POINT('Ctrl Pts',(-0.466969125257516,0.807692307692308,
0.41369847105725));
#29631=CARTESIAN_POINT('Ctrl Pts',(-0.221227750860347,0.846153846153846,
0.583326335743102));
#29632=CARTESIAN_POINT('Ctrl Pts',(0.0752027553952735,0.884615384615385,
0.619312950390957));
#29633=CARTESIAN_POINT('Ctrl Pts',(0.354387423761003,0.923076923076923,
0.513439446520879));
#29634=CARTESIAN_POINT('Ctrl Pts',(0.552422075024676,0.961538461538462,
0.289907779312462));
#29635=CARTESIAN_POINT('Ctrl Pts',(0.6,0.987179487179487,0.096664389341225));
#29636=CARTESIAN_POINT('Ctrl Pts',(0.6,1.,2.93915231795365E-16));
#29637=CARTESIAN_POINT('Origin',(0.5,1.,2.44929359829471E-16));
#29638=CARTESIAN_POINT('Origin',(0.5,1.,2.44929359829471E-16));
#29639=CARTESIAN_POINT('Origin',(0.5,1.44560289664734E-18,0.));
#29640=CARTESIAN_POINT('',(0.,0.,0.));
#29641=CARTESIAN_POINT('Origin',(0.,0.,0.));
#29642=CARTESIAN_POINT('',(-0.2,-2.44929359829471E-17,0.1));
#29643=CARTESIAN_POINT('Origin',(0.,0.,0.1));
#29644=CARTESIAN_POINT('',(-0.2,-2.44929359829471E-17,0.));
#29645=CARTESIAN_POINT('',(-0.2,-2.44929359829471E-17,0.));
#29646=CARTESIAN_POINT('Origin',(0.,0.,0.));
#29647=CARTESIAN_POINT('Origin',(0.,0.,0.));
#29648=CARTESIAN_POINT('',(-0.4,-4.89858719658941E-17,0.1));
#29649=CARTESIAN_POINT('Origin',(0.,0.,0.1));
#29650=CARTESIAN_POINT('',(-0.4,-4.89858719658941E-17,0.));
#29651=CARTESIAN_POINT('',(-0.4,-4.89858719658941E-17,0.));
#29652=CARTESIAN_POINT('Origin',(0.,0.,0.));
#29653=CARTESIAN_POINT('Origin',(0.,0.,0.1));
#29654=CARTESIAN_POINT('Origin',(0.,0.,0.));
#29655=CARTESIAN_POINT('',(0.,0.,0.));
#29656=CARTESIAN_POINT('Origin',(0.,0.,0.));
#29657=CARTESIAN_POINT('',(-0.195633559071744,0.00012731057411345,0.0225869692124231));
#29658=CARTESIAN_POINT('',(-0.195587799559821,0.000207186393275607,0.0124130307875758));
#29659=CARTESIAN_POINT('',(-0.1954,-2.39295984553393E-17,0.));
#29660=CARTESIAN_POINT('',(0.0861525859670522,0.175382131162755,0.));
#29661=CARTESIAN_POINT('Ctrl Pts',(-0.195633559071744,0.00012731057411345,
0.0225869692124231));
#29662=CARTESIAN_POINT('Ctrl Pts',(-0.195680032440099,0.00682557629313676,
0.0222037301306047));
#29663=CARTESIAN_POINT('Ctrl Pts',(-0.195365903766855,0.0135191473590706,
0.0218204910487863));
#29664=CARTESIAN_POINT('Ctrl Pts',(-0.194676806606145,0.0201735328972743,
0.0214372519669679));
#29665=CARTESIAN_POINT('Ctrl Pts',(-0.188017193281744,0.0844832371344698,
0.01773353028412));
#29666=CARTESIAN_POINT('Ctrl Pts',(-0.146336311091822,0.145133095416213,
0.0140298086012721));
#29667=CARTESIAN_POINT('Ctrl Pts',(-0.0886884671668765,0.17445317403525,
0.0103260869184242));
#29668=CARTESIAN_POINT('Ctrl Pts',(-0.0351138290053491,0.201701592986141,
0.00688405794561611));
#29669=CARTESIAN_POINT('Ctrl Pts',(0.0322511385444639,0.201891139473935,
0.00344202897280807));
#29670=CARTESIAN_POINT('Ctrl Pts',(0.0863567639152679,0.175641488315944,
2.92734586571086E-18));
#29671=CARTESIAN_POINT('',(-0.0861525859670574,0.175382131162752,1.38777878078145E-17));
#29672=CARTESIAN_POINT('Origin',(0.,0.,0.));
#29673=CARTESIAN_POINT('Ctrl Pts',(-0.0861525859670571,0.175382131162752,
2.28983498828939E-16));
#29674=CARTESIAN_POINT('Ctrl Pts',(-0.144496782441851,0.146721837385109,
0.00370621399437224));
#29675=CARTESIAN_POINT('Ctrl Pts',(-0.18691020329229,0.0869083656944534,
0.00741242798874424));
#29676=CARTESIAN_POINT('Ctrl Pts',(-0.194380023116171,0.0227435527544788,
0.0111186419831163));
#29677=CARTESIAN_POINT('Ctrl Pts',(-0.195249630318745,0.0152737362394887,
0.0115501049179361));
#29678=CARTESIAN_POINT('Ctrl Pts',(-0.195645657185248,0.00774494727773659,
0.0119815678527559));
#29679=CARTESIAN_POINT('Ctrl Pts',(-0.195587799559821,0.000207186393275607,
0.0124130307875758));
#29680=CARTESIAN_POINT('Origin',(0.,0.,0.));
#29681=CARTESIAN_POINT('',(-0.195128203910989,9.79727872364722E-5,0.092586969212423));
#29682=CARTESIAN_POINT('',(-0.195118672945361,9.16100096969453E-5,0.0824130307875757));
#29683=CARTESIAN_POINT('',(-0.1954,-2.39295984553393E-17,0.));
#29684=CARTESIAN_POINT('Ctrl Pts',(-0.195128203910989,9.79727872364722E-5,
0.092586969212423));
#29685=CARTESIAN_POINT('Ctrl Pts',(-0.19524730612105,0.0263901717292074,
0.0910927268943587));
#29686=CARTESIAN_POINT('Ctrl Pts',(-0.190305141123492,0.0526394079969068,
0.0895984845762944));
#29687=CARTESIAN_POINT('Ctrl Pts',(-0.180089049647467,0.0766440059940591,
0.0881042422582301));
#29688=CARTESIAN_POINT('Ctrl Pts',(-0.154766811710363,0.136143291361155,
0.0844005205753822));
#29689=CARTESIAN_POINT('Ctrl Pts',(-0.0970428066964404,0.181852045762203,
0.0806967988925343));
#29690=CARTESIAN_POINT('Ctrl Pts',(-0.0333230591869142,0.192861999489257,
0.0769930772096863));
#29691=CARTESIAN_POINT('Ctrl Pts',(0.030396688322612,0.20387195321631,0.0732893555268384));
#29692=CARTESIAN_POINT('Ctrl Pts',(0.100112178327742,0.18018310626937,0.0695856338439906));
#29693=CARTESIAN_POINT('Ctrl Pts',(0.143930998255098,0.132629143144902,
0.0658819121611426));
#29694=CARTESIAN_POINT('Ctrl Pts',(0.187749818182454,0.0850751800204342,
0.0621781904782947));
#29695=CARTESIAN_POINT('Ctrl Pts',(0.205671968032037,0.0136561007184397,
0.0584744687954468));
#29696=CARTESIAN_POINT('Ctrl Pts',(0.189499805994521,-0.0489512382298273,
0.0547707471125989));
#29697=CARTESIAN_POINT('Ctrl Pts',(0.173327643957006,-0.111558577178094,
0.051067025429751));
#29698=CARTESIAN_POINT('Ctrl Pts',(0.123061170032392,-0.165354175772633,
0.0473633037469032));
#29699=CARTESIAN_POINT('Ctrl Pts',(0.0616932989107385,-0.18573955796291,
0.0436595820640553));
#29700=CARTESIAN_POINT('Ctrl Pts',(0.000325427789084558,-0.206124940153187,
0.0399558603812074));
#29701=CARTESIAN_POINT('Ctrl Pts',(-0.0721438405296094,-0.193100105939202,
0.0362521386983595));
#29702=CARTESIAN_POINT('Ctrl Pts',(-0.122559302459517,-0.152602913735885,
0.0325484170155115));
#29703=CARTESIAN_POINT('Ctrl Pts',(-0.167758072371516,-0.11629613001496,
0.029227934414482));
#29704=CARTESIAN_POINT('Ctrl Pts',(-0.195230901779331,-0.0579081973692791,
0.0259074518134526));
#29705=CARTESIAN_POINT('Ctrl Pts',(-0.195633559071744,0.00012731057411345,
0.0225869692124231));
#29706=CARTESIAN_POINT('Ctrl Pts',(-0.195587799559821,0.000207186393275607,
0.0124130307875758));
#29707=CARTESIAN_POINT('Ctrl Pts',(-0.195148667238412,-0.0570034995103637,
0.015687781847128));
#29708=CARTESIAN_POINT('Ctrl Pts',(-0.168562951923343,-0.114731024226281,
0.0189625329066803));
#29709=CARTESIAN_POINT('Ctrl Pts',(-0.12444215732779,-0.151113938431406,
0.0222372839662326));
#29710=CARTESIAN_POINT('Ctrl Pts',(-0.0745082529182101,-0.192290462488019,
0.0259434979606046));
#29711=CARTESIAN_POINT('Ctrl Pts',(-0.00211422530173012,-0.20612735641195,
0.0296497119549767));
#29712=CARTESIAN_POINT('Ctrl Pts',(0.0595334795120667,-0.186428772433344,
0.0333559259493488));
#29713=CARTESIAN_POINT('Ctrl Pts',(0.121181184325864,-0.166730188454737,
0.0370621399437209));
#29714=CARTESIAN_POINT('Ctrl Pts',(0.172082566336977,-0.113496126573593,
0.040768353938093));
#29715=CARTESIAN_POINT('Ctrl Pts',(0.18894870924304,-0.0510370283185346,
0.0444745679324651));
#29716=CARTESIAN_POINT('Ctrl Pts',(0.205814852149104,0.0114220699365238,
0.0481807819268372));
#29717=CARTESIAN_POINT('Ctrl Pts',(0.188645755950116,0.0831062045654966,
0.0518869959212093));
#29718=CARTESIAN_POINT('Ctrl Pts',(0.145292142815886,0.131145007703775,
0.0555932099155814));
#29719=CARTESIAN_POINT('Ctrl Pts',(0.101938529681656,0.179183810842053,
0.0592994239099535));
#29720=CARTESIAN_POINT('Ctrl Pts',(0.0324003996121834,0.203577282489637,
0.0630056379043256));
#29721=CARTESIAN_POINT('Ctrl Pts',(-0.0314654015224673,0.193172336479658,
0.0667118518986976));
#29722=CARTESIAN_POINT('Ctrl Pts',(-0.0953312026571179,0.18276739046968,
0.0704180658930697));
#29723=CARTESIAN_POINT('Ctrl Pts',(-0.153524674856946,0.137564026802139,
0.0741242798874417));
#29724=CARTESIAN_POINT('Ctrl Pts',(-0.179395555636014,0.0782560471576942,
0.0778304938818138));
#29725=CARTESIAN_POINT('Ctrl Pts',(-0.190058212652462,0.0538123240897563,
0.0793580061837345));
#29726=CARTESIAN_POINT('Ctrl Pts',(-0.195230335199157,0.0269726953471863,
0.0808855184856551));
#29727=CARTESIAN_POINT('Ctrl Pts',(-0.195118672945361,9.16100096969453E-5,
0.0824130307875757));
#29728=CARTESIAN_POINT('Origin',(0.,0.,0.));
#29729=CARTESIAN_POINT('',(-0.195279554503994,-0.000168121501241181,0.162586969212423));
#29730=CARTESIAN_POINT('',(-0.195287184048439,-0.0001702989282844,0.152413030787576));
#29731=CARTESIAN_POINT('',(-0.1954,-2.39295984553393E-17,0.));
#29732=CARTESIAN_POINT('Ctrl Pts',(-0.195279554503994,-0.000168121501241181,
0.162586969212423));
#29733=CARTESIAN_POINT('Ctrl Pts',(-0.194903656010943,0.0455834752155161,
0.159981723658113));
#29734=CARTESIAN_POINT('Ctrl Pts',(-0.178856730317397,0.091572573117829,
0.157376478103802));
#29735=CARTESIAN_POINT('Ctrl Pts',(-0.149500760249196,0.126316552728133,
0.154771232549492));
#29736=CARTESIAN_POINT('Ctrl Pts',(-0.107767134532898,0.175709989142681,
0.151067510866644));
#29737=CARTESIAN_POINT('Ctrl Pts',(-0.039135122029848,0.202376358702057,
0.147363789183796));
#29738=CARTESIAN_POINT('Ctrl Pts',(0.0249990333148566,0.194116955279127,
0.143660067500948));
#29739=CARTESIAN_POINT('Ctrl Pts',(0.0891331886595613,0.185857551856197,
0.139956345818101));
#29740=CARTESIAN_POINT('Ctrl Pts',(0.14876948684592,0.142672375450961,0.136252624135253));
#29741=CARTESIAN_POINT('Ctrl Pts',(0.176626827046517,0.0843167597229759,
0.132548902452405));
#29742=CARTESIAN_POINT('Ctrl Pts',(0.204484167247113,0.0259611439949913,
0.128845180769557));
#29743=CARTESIAN_POINT('Ctrl Pts',(0.200562549461947,-0.0475649110557425,
0.125141459086709));
#29744=CARTESIAN_POINT('Ctrl Pts',(0.166655969053473,-0.102626219289756,
0.121437737403861));
#29745=CARTESIAN_POINT('Ctrl Pts',(0.132749388644999,-0.157687527523771,
0.117734015721013));
#29746=CARTESIAN_POINT('Ctrl Pts',(0.0688578456132156,-0.194284088941065,
0.114030294038165));
#29747=CARTESIAN_POINT('Ctrl Pts',(0.00420898544956178,-0.19567474659654,
0.110326572355317));
#29748=CARTESIAN_POINT('Ctrl Pts',(-0.0604398747140919,-0.197065404252014,
0.106622850672469));
#29749=CARTESIAN_POINT('Ctrl Pts',(-0.125846052009616,-0.16325015814567,
0.102919128989622));
#29750=CARTESIAN_POINT('Ctrl Pts',(-0.162088905227235,-0.109697626925925,
0.0992154073067737));
#29751=CARTESIAN_POINT('Ctrl Pts',(-0.183709816073764,-0.0777505145902677,
0.0970059279419901));
#29752=CARTESIAN_POINT('Ctrl Pts',(-0.194952091996443,-0.0387793032173158,
0.0947964485772066));
#29753=CARTESIAN_POINT('Ctrl Pts',(-0.195128203910989,9.79727872364722E-5,
0.092586969212423));
#29754=CARTESIAN_POINT('Ctrl Pts',(-0.195118672945361,9.16100096969453E-5,
0.0824130307875757));
#29755=CARTESIAN_POINT('Ctrl Pts',(-0.194959408276249,-0.0382490737583375,
0.0845917324800272));
#29756=CARTESIAN_POINT('Ctrl Pts',(-0.184051065227066,-0.0766740948347571,
0.0867704341724787));
#29757=CARTESIAN_POINT('Ctrl Pts',(-0.162993550876047,-0.10835175828476,
0.0889491358649302));
#29758=CARTESIAN_POINT('Ctrl Pts',(-0.127172375978705,-0.162238988461419,
0.0926553498593023));
#29759=CARTESIAN_POINT('Ctrl Pts',(-0.0619817368257128,-0.196600853193387,
0.0963615638536743));
#29760=CARTESIAN_POINT('Ctrl Pts',(0.0027186436745272,-0.195701720127518,
0.100067777848046));
#29761=CARTESIAN_POINT('Ctrl Pts',(0.0674190241747668,-0.194802587061648,
0.103773991842418));
#29762=CARTESIAN_POINT('Ctrl Pts',(0.131629146022255,-0.15864245619794,
0.107480205836791));
#29763=CARTESIAN_POINT('Ctrl Pts',(0.165939903784035,-0.103781956343241,
0.111186419831163));
#29764=CARTESIAN_POINT('Ctrl Pts',(0.200250661545815,-0.0489214564885407,
0.114892633825535));
#29765=CARTESIAN_POINT('Ctrl Pts',(0.204662055221888,0.0246394123571516,
0.118598847819907));
#29766=CARTESIAN_POINT('Ctrl Pts',(0.177153295980734,0.0832073910176122,
0.122305061814279));
#29767=CARTESIAN_POINT('Ctrl Pts',(0.149644536739581,0.141775369678073,
0.126011275808651));
#29768=CARTESIAN_POINT('Ctrl Pts',(0.0902156245812001,0.185350458153303,
0.129717489803023));
#29769=CARTESIAN_POINT('Ctrl Pts',(0.0260864347694114,0.193974733338565,
0.133423703797395));
#29770=CARTESIAN_POINT('Ctrl Pts',(-0.0380427550423769,0.202599008523827,
0.137129917791767));
#29771=CARTESIAN_POINT('Ctrl Pts',(-0.106872222507573,0.176272470419122,
0.140836131786139));
#29772=CARTESIAN_POINT('Ctrl Pts',(-0.148876654315921,0.127053027794487,
0.144542345780511));
#29773=CARTESIAN_POINT('Ctrl Pts',(-0.178610829781436,0.0922114770268632,
0.147165907449533));
#29774=CARTESIAN_POINT('Ctrl Pts',(-0.194903067523895,0.0458983666015645,
0.149789469118554));
#29775=CARTESIAN_POINT('Ctrl Pts',(-0.195287184048439,-0.0001702989282844,
0.152413030787576));
#29776=CARTESIAN_POINT('Origin',(0.,0.,0.));
#29777=CARTESIAN_POINT('',(-0.19571996697324,4.08272333451705E-6,0.232586969212423));
#29778=CARTESIAN_POINT('',(-0.195720915199432,4.37834080700025E-6,0.222413030787575));
#29779=CARTESIAN_POINT('',(-0.1954,-2.39295984553393E-17,0.));
#29780=CARTESIAN_POINT('Ctrl Pts',(-0.19571996697324,4.08272333451705E-6,
0.232586969212423));
#29781=CARTESIAN_POINT('Ctrl Pts',(-0.19573993069631,0.0648866965015804,
0.228870720421867));
#29782=CARTESIAN_POINT('Ctrl Pts',(-0.160252793092098,0.129750264469882,
0.225154471631311));
#29783=CARTESIAN_POINT('Ctrl Pts',(-0.105631192010051,0.164767712566922,
0.221438222840754));
#29784=CARTESIAN_POINT('Ctrl Pts',(-0.0511937149515876,0.19966712030426,
0.217734501157906));
#29785=CARTESIAN_POINT('Ctrl Pts',(0.0222490761444335,0.204921286910345,
0.214030779475058));
#29786=CARTESIAN_POINT('Ctrl Pts',(0.0811002035332165,0.178126653559889,
0.210327057792211));
#29787=CARTESIAN_POINT('Ctrl Pts',(0.139951330921999,0.151332020209433,
0.206623336109363));
#29788=CARTESIAN_POINT('Ctrl Pts',(0.184210794603544,0.0924885869024359,
0.202919614426515));
#29789=CARTESIAN_POINT('Ctrl Pts',(0.193631757329266,0.028514740055385,
0.199215892743667));
#29790=CARTESIAN_POINT('Ctrl Pts',(0.203052720054988,-0.0354591067916664,
0.195512171060819));
#29791=CARTESIAN_POINT('Ctrl Pts',(0.177635181824887,-0.104563367178771,
0.191808449377971));
#29792=CARTESIAN_POINT('Ctrl Pts',(0.129006594271768,-0.147185755477259,
0.188104727695123));
#29793=CARTESIAN_POINT('Ctrl Pts',(0.0803780067186484,-0.189808143775746,
0.184401006012275));
#29794=CARTESIAN_POINT('Ctrl Pts',(0.00853836984250916,-0.205948659985616,
0.180697284329427));
#29795=CARTESIAN_POINT('Ctrl Pts',(-0.0536487147273854,-0.188223703762279,
0.176993562646579));
#29796=CARTESIAN_POINT('Ctrl Pts',(-0.11583579929728,-0.170498747538942,
0.173289840963732));
#29797=CARTESIAN_POINT('Ctrl Pts',(-0.168370331560931,-0.118908318882399,
0.169586119280884));
#29798=CARTESIAN_POINT('Ctrl Pts',(-0.187219978227984,-0.0570528529192665,
0.165882397598036));
#29799=CARTESIAN_POINT('Ctrl Pts',(-0.192810540551016,-0.0387073187246384,
0.164783921469498));
#29800=CARTESIAN_POINT('Ctrl Pts',(-0.195438048401311,-0.0194588316428207,
0.163685445340961));
#29801=CARTESIAN_POINT('Ctrl Pts',(-0.195279554503994,-0.000168121501241181,
0.162586969212423));
#29802=CARTESIAN_POINT('Ctrl Pts',(-0.195287184048439,-0.0001702989282844,
0.152413030787576));
#29803=CARTESIAN_POINT('Ctrl Pts',(-0.195445695530526,-0.0191812291650776,
0.153495683112926));
#29804=CARTESIAN_POINT('Ctrl Pts',(-0.192895173588402,-0.0381505322742495,
0.154578335438277));
#29805=CARTESIAN_POINT('Ctrl Pts',(-0.187462310228399,-0.0562548805321496,
0.155660987763628));
#29806=CARTESIAN_POINT('Ctrl Pts',(-0.168864138181028,-0.118230999089587,
0.159367201758));
#29807=CARTESIAN_POINT('Ctrl Pts',(-0.116488397934787,-0.170070889059896,
0.163073415752372));
#29808=CARTESIAN_POINT('Ctrl Pts',(-0.0543243355780667,-0.188030816136644,
0.166779629746744));
#29809=CARTESIAN_POINT('Ctrl Pts',(0.0078397267786532,-0.205990743213392,
0.170485843741116));
#29810=CARTESIAN_POINT('Ctrl Pts',(0.0797921112458524,-0.190070707396579,
0.174192057735488));
#29811=CARTESIAN_POINT('Ctrl Pts',(0.128577075941843,-0.147562399010748,
0.17789827172986));
#29812=CARTESIAN_POINT('Ctrl Pts',(0.177362040637834,-0.105054090624917,
0.181604485724232));
#29813=CARTESIAN_POINT('Ctrl Pts',(0.202979585562615,-0.0359575096700667,
0.185310699718604));
#29814=CARTESIAN_POINT('Ctrl Pts',(0.193696313672928,0.028079594435252,
0.189016913712976));
#29815=CARTESIAN_POINT('Ctrl Pts',(0.184413041783241,0.0921166985405712,
0.192723127707349));
#29816=CARTESIAN_POINT('Ctrl Pts',(0.140228953079084,0.151094325796358,
0.196429341701721));
#29817=CARTESIAN_POINT('Ctrl Pts',(0.0813813216582781,0.177999452248681,
0.200135555696093));
#29818=CARTESIAN_POINT('Ctrl Pts',(0.0225336902374724,0.204904578701004,
0.203841769690465));
#29819=CARTESIAN_POINT('Ctrl Pts',(-0.0509774838999832,0.199737204349863,
0.207547983684837));
#29820=CARTESIAN_POINT('Ctrl Pts',(-0.105482489992153,0.164864094185095,
0.211254197679209));
#29821=CARTESIAN_POINT('Ctrl Pts',(-0.16018451812442,0.129864926401004,
0.214973808715331));
#29822=CARTESIAN_POINT('Ctrl Pts',(-0.195742302622205,0.0649448754401196,
0.218693419751453));
#29823=CARTESIAN_POINT('Ctrl Pts',(-0.195720915199432,4.37834080700025E-6,
0.222413030787575));
#29824=CARTESIAN_POINT('Origin',(0.,0.,0.));
#29825=CARTESIAN_POINT('',(-0.195267691385146,0.000165493661177622,0.302586969212423));
#29826=CARTESIAN_POINT('',(-0.195274315056508,0.000167675988910205,0.292413030787576));
#29827=CARTESIAN_POINT('',(-0.1954,-2.39295984553393E-17,0.));
#29828=CARTESIAN_POINT('Ctrl Pts',(-0.195267691385146,0.000165493661177622,
0.302586969212423));
#29829=CARTESIAN_POINT('Ctrl Pts',(-0.195426560914452,0.0198992208020636,
0.301463438868469));
#29830=CARTESIAN_POINT('Ctrl Pts',(-0.192675342506316,0.0395896803504792,
0.300339908524515));
#29831=CARTESIAN_POINT('Ctrl Pts',(-0.186830808103941,0.0583146374609883,
0.29921637818056));
#29832=CARTESIAN_POINT('Ctrl Pts',(-0.167564280138135,0.120041523640586,
0.295512656497712));
#29833=CARTESIAN_POINT('Ctrl Pts',(-0.114682887836242,0.171276357431471,
0.291808934814864));
#29834=CARTESIAN_POINT('Ctrl Pts',(-0.0523776367443795,0.188581364320311,
0.288105213132016));
#29835=CARTESIAN_POINT('Ctrl Pts',(0.00992761434748341,0.20588637120915,
0.284401491449168));
#29836=CARTESIAN_POINT('Ctrl Pts',(0.0816567242293159,0.189261551195942,
0.280697769766321));
#29837=CARTESIAN_POINT('Ctrl Pts',(0.129996651882171,0.146312057934516,
0.276994048083473));
#29838=CARTESIAN_POINT('Ctrl Pts',(0.178336579535026,0.103362564673089,
0.273290326400625));
#29839=CARTESIAN_POINT('Ctrl Pts',(0.203287324958903,0.0340883981634439,
0.269586604717777));
#29840=CARTESIAN_POINT('Ctrl Pts',(0.193434974962867,-0.0298204336020968,
0.265882883034929));
#29841=CARTESIAN_POINT('Ctrl Pts',(0.183582624966831,-0.0937292653676373,
0.262179161352081));
#29842=CARTESIAN_POINT('Ctrl Pts',(0.138927179550881,-0.152272762389073,
0.258475439669233));
#29843=CARTESIAN_POINT('Ctrl Pts',(0.0798966206784796,-0.178669745083631,
0.254771717986385));
#29844=CARTESIAN_POINT('Ctrl Pts',(0.0208660618060775,-0.205066727778188,
0.251067996303538));
#29845=CARTESIAN_POINT('Ctrl Pts',(-0.0525396105227766,-0.199317196145866,
0.24736427462069));
#29846=CARTESIAN_POINT('Ctrl Pts',(-0.10674039873032,-0.16405131839538,
0.243660552937842));
#29847=CARTESIAN_POINT('Ctrl Pts',(-0.160757863467609,-0.128904720517098,
0.239969358362702));
#29848=CARTESIAN_POINT('Ctrl Pts',(-0.195700137841649,-0.0644411052866131,
0.236278163787563));
#29849=CARTESIAN_POINT('Ctrl Pts',(-0.19571996697324,4.08272333451705E-6,
0.232586969212423));
#29850=CARTESIAN_POINT('Ctrl Pts',(-0.195720915199432,4.37834080700025E-6,
0.222413030787575));
#29851=CARTESIAN_POINT('Ctrl Pts',(-0.195699681840184,-0.0644683222376,
0.226105847740198));
#29852=CARTESIAN_POINT('Ctrl Pts',(-0.160725113883781,-0.128960760246236,
0.22979866469282));
#29853=CARTESIAN_POINT('Ctrl Pts',(-0.106669244200308,-0.164098742623895,
0.233491481645442));
#29854=CARTESIAN_POINT('Ctrl Pts',(-0.0524172671136578,-0.199364200861572,
0.237197695639814));
#29855=CARTESIAN_POINT('Ctrl Pts',(0.0210547116140745,-0.205061829112049,
0.240903909634186));
#29856=CARTESIAN_POINT('Ctrl Pts',(0.0800949322066953,-0.178581989384044,
0.244610123628558));
#29857=CARTESIAN_POINT('Ctrl Pts',(0.139135152799316,-0.152102149656038,
0.24831633762293));
#29858=CARTESIAN_POINT('Ctrl Pts',(0.183743615256826,-0.0934448419495488,
0.252022551617302));
#29859=CARTESIAN_POINT('Ctrl Pts',(0.193488676008295,-0.0294763859316313,
0.255728765611674));
#29860=CARTESIAN_POINT('Ctrl Pts',(0.203233736759764,0.0344920700862864,
0.259434979606046));
#29861=CARTESIAN_POINT('Ctrl Pts',(0.178115395805193,0.103771674415633,
0.263141193600418));
#29862=CARTESIAN_POINT('Ctrl Pts',(0.129638398231036,0.146630865646616,
0.26684740759479));
#29863=CARTESIAN_POINT('Ctrl Pts',(0.0811614006568792,0.1894900568776,0.270553621589162));
#29864=CARTESIAN_POINT('Ctrl Pts',(0.00932574646313782,0.205928835010221,
0.274259835583535));
#29865=CARTESIAN_POINT('Ctrl Pts',(-0.0529662765081927,0.188417882975093,
0.277966049577907));
#29866=CARTESIAN_POINT('Ctrl Pts',(-0.115258299479523,0.170906930939964,
0.281672263572279));
#29867=CARTESIAN_POINT('Ctrl Pts',(-0.168006691228442,0.119446248737086,
0.285378477566651));
#29868=CARTESIAN_POINT('Ctrl Pts',(-0.187051544101399,0.0576059451476712,
0.289084691561023));
#29869=CARTESIAN_POINT('Ctrl Pts',(-0.192752575844056,0.0390941962730205,
0.290194137969874));
#29870=CARTESIAN_POINT('Ctrl Pts',(-0.195433466869055,0.0196523398123763,
0.291303584378725));
#29871=CARTESIAN_POINT('Ctrl Pts',(-0.195274315056508,0.000167675988910205,
0.292413030787576));
#29872=CARTESIAN_POINT('Origin',(0.,0.,0.));
#29873=CARTESIAN_POINT('',(-0.195135107115213,-0.000103745302926256,0.372586969212423));
#29874=CARTESIAN_POINT('',(-0.195125983814034,-9.67513988672578E-5,0.362413030787576));
#29875=CARTESIAN_POINT('',(-0.1954,-2.39295984553393E-17,0.));
#29876=CARTESIAN_POINT('Ctrl Pts',(-0.195135107115213,-0.000103745302926256,
0.372586969212423));
#29877=CARTESIAN_POINT('Ctrl Pts',(-0.19494564270682,0.0392108141373472,
0.370352435632223));
#29878=CARTESIAN_POINT('Ctrl Pts',(-0.183428685915158,0.078627490539017,
0.368117902052023));
#29879=CARTESIAN_POINT('Ctrl Pts',(-0.161345116677478,0.110788542383069,
0.365883368471823));
#29880=CARTESIAN_POINT('Ctrl Pts',(-0.124741775852795,0.164095230684139,
0.362179646788975));
#29881=CARTESIAN_POINT('Ctrl Pts',(-0.0591089924893776,0.197468687095231,
0.358475925106126));
#29882=CARTESIAN_POINT('Ctrl Pts',(0.00552900452708404,0.195641963566092,
0.354772203423278));
#29883=CARTESIAN_POINT('Ctrl Pts',(0.0701670015435453,0.193815240036952,
0.351068481740431));
#29884=CARTESIAN_POINT('Ctrl Pts',(0.13381021221305,0.156788336567581,0.347364760057583));
#29885=CARTESIAN_POINT('Ctrl Pts',(0.16734455320356,0.101499499073225,0.343661038374735));
#29886=CARTESIAN_POINT('Ctrl Pts',(0.20087889419407,0.0462106615788698,
0.339957316691887));
#29887=CARTESIAN_POINT('Ctrl Pts',(0.204304365505584,-0.0273401099404705,
0.336253595009039));
#29888=CARTESIAN_POINT('Ctrl Pts',(0.176053958557416,-0.0855064411333041,
0.332549873326191));
#29889=CARTESIAN_POINT('Ctrl Pts',(0.147803551609248,-0.143672772326139,
0.328846151643343));
#29890=CARTESIAN_POINT('Ctrl Pts',(0.0878772664013962,-0.186454663192466,
0.325142429960495));
#29891=CARTESIAN_POINT('Ctrl Pts',(0.0236888497103484,-0.194281203925035,
0.321438708277648));
#29892=CARTESIAN_POINT('Ctrl Pts',(-0.0404995669806982,-0.202107744657604,
0.3177349865948));
#29893=CARTESIAN_POINT('Ctrl Pts',(-0.108950115154941,-0.174978935256416,
0.314031264911952));
#29894=CARTESIAN_POINT('Ctrl Pts',(-0.150349557427203,-0.125305061271667,
0.310327543229104));
#29895=CARTESIAN_POINT('Ctrl Pts',(-0.179190407667273,-0.0906998424134863,
0.30774735189021));
#29896=CARTESIAN_POINT('Ctrl Pts',(-0.194902846959061,-0.0451530792879088,
0.305167160551317));
#29897=CARTESIAN_POINT('Ctrl Pts',(-0.195267691385146,0.000165493661177622,
0.302586969212423));
#29898=CARTESIAN_POINT('Ctrl Pts',(-0.195274315056508,0.000167675988910205,
0.292413030787576));
#29899=CARTESIAN_POINT('Ctrl Pts',(-0.194901804708373,-0.045438081105706,
0.295009798373097));
#29900=CARTESIAN_POINT('Ctrl Pts',(-0.178970412039892,-0.0912783539307832,
0.297606565958618));
#29901=CARTESIAN_POINT('Ctrl Pts',(-0.149789482266332,-0.125975537577289,
0.300203333544139));
#29902=CARTESIAN_POINT('Ctrl Pts',(-0.108141253561316,-0.175496791736879,
0.303909547538511));
#29903=CARTESIAN_POINT('Ctrl Pts',(-0.03950348215429,-0.202319375080107,
0.307615761532883));
#29904=CARTESIAN_POINT('Ctrl Pts',(0.0246862437687336,-0.194157962588032,
0.311321975527255));
#29905=CARTESIAN_POINT('Ctrl Pts',(0.0888759696917571,-0.185996550095957,
0.315028189521628));
#29906=CARTESIAN_POINT('Ctrl Pts',(0.148617650130778,-0.14285114176858,
0.318734403516));
#29907=CARTESIAN_POINT('Ctrl Pts',(0.176548299529208,-0.084483270534745,
0.322440617510372));
#29908=CARTESIAN_POINT('Ctrl Pts',(0.204478948927638,-0.0261153993009101,
0.326146831504744));
#29909=CARTESIAN_POINT('Ctrl Pts',(0.200598567285476,0.0474749348393822,
0.329853045499116));
#29910=CARTESIAN_POINT('Ctrl Pts',(0.166684453569178,0.102581762536563,
0.333559259493488));
#29911=CARTESIAN_POINT('Ctrl Pts',(0.13277033985288,0.157688590233743,0.33726547348786));
#29912=CARTESIAN_POINT('Ctrl Pts',(0.0688224940624468,0.194311911487812,
0.340971687482232));
#29913=CARTESIAN_POINT('Ctrl Pts',(0.00413041672205065,0.195677450731496,
0.344677901476604));
#29914=CARTESIAN_POINT('Ctrl Pts',(-0.0605616606183457,0.19704298997518,
0.348384115470976));
#29915=CARTESIAN_POINT('Ctrl Pts',(-0.125997969508704,0.163150747208479,
0.352090329465349));
#29916=CARTESIAN_POINT('Ctrl Pts',(-0.162207261036362,0.109524104808107,
0.355796543459721));
#29917=CARTESIAN_POINT('Ctrl Pts',(-0.183754705311226,0.0776119342016343,
0.358002039235672));
#29918=CARTESIAN_POINT('Ctrl Pts',(-0.194952253842872,0.0387114015523011,
0.360207535011624));
#29919=CARTESIAN_POINT('Ctrl Pts',(-0.195125983814034,-9.67513988672578E-5,
0.362413030787576));
#29920=CARTESIAN_POINT('Origin',(0.,0.,0.));
#29921=CARTESIAN_POINT('',(-0.195645574651684,-0.000107576288577632,0.442586969212423));
#29922=CARTESIAN_POINT('',(-0.195628130950281,-0.000119277919923279,0.432413030787576));
#29923=CARTESIAN_POINT('',(-0.1954,-2.39295984553393E-17,0.));
#29924=CARTESIAN_POINT('Ctrl Pts',(-0.195645574651684,-0.000107576288577632,
0.442586969212423));
#29925=CARTESIAN_POINT('Ctrl Pts',(-0.195258201164419,0.0583617837825317,
0.439241432395977));
#29926=CARTESIAN_POINT('Ctrl Pts',(-0.167312331125722,0.117152394520949,
0.435895895579531));
#29927=CARTESIAN_POINT('Ctrl Pts',(-0.121525966387556,0.153420296221226,
0.432550358763085));
#29928=CARTESIAN_POINT('Ctrl Pts',(-0.070837553387317,0.193571166257503,
0.428846637080237));
#29929=CARTESIAN_POINT('Ctrl Pts',(0.00171598407939347,0.206118438706562,
0.425142915397389));
#29930=CARTESIAN_POINT('Ctrl Pts',(0.0629444641593513,0.18532226587955,
0.421439193714541));
#29931=CARTESIAN_POINT('Ctrl Pts',(0.124172944239309,0.164526093052537,
0.417735472031693));
#29932=CARTESIAN_POINT('Ctrl Pts',(0.174076366932515,0.110386474949453,
0.414031750348845));
#29933=CARTESIAN_POINT('Ctrl Pts',(0.189826022128925,0.0476700023258525,
0.410328028665997));
#29934=CARTESIAN_POINT('Ctrl Pts',(0.205575677325334,-0.0150464702977478,
0.406624306983149));
#29935=CARTESIAN_POINT('Ctrl Pts',(0.187171565024948,-0.086339797441863,
0.402920585300301));
#29936=CARTESIAN_POINT('Ctrl Pts',(0.143032790007833,-0.133596290298842,
0.399216863617453));
#29937=CARTESIAN_POINT('Ctrl Pts',(0.0988940149907184,-0.180852783155821,
0.395513141934605));
#29938=CARTESIAN_POINT('Ctrl Pts',(0.0290205772568748,-0.204072441725662,
0.391809420251758));
#29939=CARTESIAN_POINT('Ctrl Pts',(-0.0346233738762281,-0.192633252011348,
0.38810569856891));
#29940=CARTESIAN_POINT('Ctrl Pts',(-0.0982673250093302,-0.181194062297035,
0.384401976886062));
#29941=CARTESIAN_POINT('Ctrl Pts',(-0.155681789541692,-0.135096024298568,
0.380698255203214));
#29942=CARTESIAN_POINT('Ctrl Pts',(-0.1806020726649,-0.0754270452038098,
0.376994533520366));
#29943=CARTESIAN_POINT('Ctrl Pts',(-0.190487422217158,-0.0517576224744695,
0.375525345417718));
#29944=CARTESIAN_POINT('Ctrl Pts',(-0.19525967846073,-0.0259527562563923,
0.374056157315071));
#29945=CARTESIAN_POINT('Ctrl Pts',(-0.195135107115213,-0.000103745302926256,
0.372586969212423));
#29946=CARTESIAN_POINT('Ctrl Pts',(-0.195125983814034,-9.67513988672578E-5,
0.362413030787576));
#29947=CARTESIAN_POINT('Ctrl Pts',(-0.195244197476311,-0.0265035587897937,
0.363913749005996));
#29948=CARTESIAN_POINT('Ctrl Pts',(-0.190258326051973,-0.0528675939020291,
0.365414467224416));
#29949=CARTESIAN_POINT('Ctrl Pts',(-0.1799560505048,-0.0769580726996389,
0.366915185442837));
#29950=CARTESIAN_POINT('Ctrl Pts',(-0.154513274280624,-0.136452565772967,
0.370621399437209));
#29951=CARTESIAN_POINT('Ctrl Pts',(-0.0966454476673152,-0.18208050988558,
0.374327613431581));
#29952=CARTESIAN_POINT('Ctrl Pts',(-0.0328572905191125,-0.192943316874967,
0.378033827425953));
#29953=CARTESIAN_POINT('Ctrl Pts',(0.0309308666290907,-0.203806123864353,
0.381740041420325));
#29954=CARTESIAN_POINT('Ctrl Pts',(0.100639354312189,-0.179903793730513,
0.385446255414697));
#29955=CARTESIAN_POINT('Ctrl Pts',(0.144340173058911,-0.132184112162819,
0.389152469409069));
#29956=CARTESIAN_POINT('Ctrl Pts',(0.188040991805633,-0.0844644305951239,
0.392858683403441));
#29957=CARTESIAN_POINT('Ctrl Pts',(0.205734141615979,-0.0129273975935752,
0.396564897397814));
#29958=CARTESIAN_POINT('Ctrl Pts',(0.189315776078089,0.0496614739501458,
0.400271111392186));
#29959=CARTESIAN_POINT('Ctrl Pts',(0.172897410540198,0.112250345493866,
0.403977325386558));
#29960=CARTESIAN_POINT('Ctrl Pts',(0.122367529654071,0.165891055579759,
0.40768353938093));
#29961=CARTESIAN_POINT('Ctrl Pts',(0.0608699149567017,0.186014995417357,
0.411389753375302));
#29962=CARTESIAN_POINT('Ctrl Pts',(-0.000627699740667481,0.206138935254955,
0.415095967369674));
#29963=CARTESIAN_POINT('Ctrl Pts',(-0.0730930482492791,0.19274610484426,
0.418802181364046));
#29964=CARTESIAN_POINT('Ctrl Pts',(-0.123335429038162,0.151970711029871,
0.422508395358418));
#29965=CARTESIAN_POINT('Ctrl Pts',(-0.168092015819396,0.115647443240051,
0.425809940501471));
#29966=CARTESIAN_POINT('Ctrl Pts',(-0.195213599025838,0.0575947822566119,
0.429111485644523));
#29967=CARTESIAN_POINT('Ctrl Pts',(-0.195628130950281,-0.000119277919923279,
0.432413030787576));
#29968=CARTESIAN_POINT('Origin',(0.,0.,0.));
#29969=CARTESIAN_POINT('',(-0.195458266482996,0.000173443779922018,0.512586969212423));
#29970=CARTESIAN_POINT('',(-0.195491180920002,0.000168629508682236,0.502413030787576));
#29971=CARTESIAN_POINT('',(-0.1954,-2.39295984553393E-17,0.));
#29972=CARTESIAN_POINT('Ctrl Pts',(-0.195458266482996,0.000173443779922018,
0.512586969212423));
#29973=CARTESIAN_POINT('Ctrl Pts',(-0.195579683437623,0.013363129532035,
0.511834150842579));
#29974=CARTESIAN_POINT('Ctrl Pts',(-0.194358523444966,0.0265304620125551,
0.511081332472735));
#29975=CARTESIAN_POINT('Ctrl Pts',(-0.191712292268468,0.0394048828472761,
0.510328514102891));
#29976=CARTESIAN_POINT('Ctrl Pts',(-0.178693343503641,0.10274455880328,
0.506624792420043));
#29977=CARTESIAN_POINT('Ctrl Pts',(-0.131181246839585,0.158994452273665,
0.502921070737195));
#29978=CARTESIAN_POINT('Ctrl Pts',(-0.0709107816346671,0.18242261056952,
0.499217349054347));
#29979=CARTESIAN_POINT('Ctrl Pts',(-0.0106403164297495,0.205850768865374,
0.495513627371499));
#29980=CARTESIAN_POINT('Ctrl Pts',(0.0623885173160298,0.196457191986698,
0.491809905688651));
#29981=CARTESIAN_POINT('Ctrl Pts',(0.114768109757825,0.158539044975217,
0.488106184005803));
#29982=CARTESIAN_POINT('Ctrl Pts',(0.167147702199619,0.120620897963737,
0.484402462322955));
#29983=CARTESIAN_POINT('Ctrl Pts',(0.19887805333743,0.0541781808194522,
0.480698740640107));
#29984=CARTESIAN_POINT('Ctrl Pts',(0.195443866449662,-0.0103943670439598,
0.476995018957259));
#29985=CARTESIAN_POINT('Ctrl Pts',(0.192009679561895,-0.0749669149073727,
0.473291297274411));
#29986=CARTESIAN_POINT('Ctrl Pts',(0.153410954648549,-0.137669293489913,
0.469587575591563));
#29987=CARTESIAN_POINT('Ctrl Pts',(0.0973049796091196,-0.169817810439032,
0.465883853908716));
#29988=CARTESIAN_POINT('Ctrl Pts',(0.0411990045696909,-0.20196632738815,
0.462180132225868));
#29989=CARTESIAN_POINT('Ctrl Pts',(-0.0324142205958206,-0.203560982703848,
0.45847641054302));
#29990=CARTESIAN_POINT('Ctrl Pts',(-0.0898597516275757,-0.17387228886878,
0.454772688860172));
#29991=CARTESIAN_POINT('Ctrl Pts',(-0.147305282659331,-0.144183595033712,
0.451068967177324));
#29992=CARTESIAN_POINT('Ctrl Pts',(-0.18858311955733,-0.0832115520478776,
0.447365245494476));
#29993=CARTESIAN_POINT('Ctrl Pts',(-0.194810393739446,-0.0188482967432128,
0.443661523811628));
#29994=CARTESIAN_POINT('Ctrl Pts',(-0.19541262996613,-0.0126237620787308,
0.443303338945226));
#29995=CARTESIAN_POINT('Ctrl Pts',(-0.195687048211354,-0.00636751036633503,
0.442945154078825));
#29996=CARTESIAN_POINT('Ctrl Pts',(-0.195645574651684,-0.000107576288577632,
0.442586969212423));
#29997=CARTESIAN_POINT('Ctrl Pts',(-0.195628130950281,-0.000119277919923279,
0.432413030787576));
#29998=CARTESIAN_POINT('Ctrl Pts',(-0.195678939935296,-0.00719326340995119,
0.432817699638895));
#29999=CARTESIAN_POINT('Ctrl Pts',(-0.195328521122814,-0.014262162001596,
0.433222368490215));
#30000=CARTESIAN_POINT('Ctrl Pts',(-0.194560169264522,-0.0212853377401693,
0.433627037341534));
#30001=CARTESIAN_POINT('Ctrl Pts',(-0.187523115632842,-0.0856080354777335,
0.437333251335906));
#30002=CARTESIAN_POINT('Ctrl Pts',(-0.145429595300328,-0.146095473734778,
0.441039465330279));
#30003=CARTESIAN_POINT('Ctrl Pts',(-0.0875593536694013,-0.175043093699665,
0.444745679324651));
#30004=CARTESIAN_POINT('Ctrl Pts',(-0.0296891120384743,-0.203990713664554,
0.448451893319023));
#30005=CARTESIAN_POINT('Ctrl Pts',(0.0439578508908652,-0.201398515337285,
0.452158107313395));
#30006=CARTESIAN_POINT('Ctrl Pts',(0.09964962855145,-0.168453781781564,
0.455864321307767));
#30007=CARTESIAN_POINT('Ctrl Pts',(0.155341406212034,-0.135509048225843,
0.459570535302139));
#30008=CARTESIAN_POINT('Ctrl Pts',(0.193077998603865,-0.072211779441669,
0.463276749296511));
#30009=CARTESIAN_POINT('Ctrl Pts',(0.195575227831571,-0.00755349757277263,
0.466982963290883));
#30010=CARTESIAN_POINT('Ctrl Pts',(0.198072457059277,0.0571047842961237,
0.470689177285256));
#30011=CARTESIAN_POINT('Ctrl Pts',(0.16533032312286,0.123124079249743,0.474395391279627));
#30012=CARTESIAN_POINT('Ctrl Pts',(0.112345433605614,0.160266118112717,
0.478101605273999));
#30013=CARTESIAN_POINT('Ctrl Pts',(0.059360544088369,0.197408156975691,
0.481807819268371));
#30014=CARTESIAN_POINT('Ctrl Pts',(-0.0138671010097046,0.20567293974802,
0.485514033262744));
#30015=CARTESIAN_POINT('Ctrl Pts',(-0.0737976517839776,0.181275016640803,
0.489220247257116));
#30016=CARTESIAN_POINT('Ctrl Pts',(-0.133728202558251,0.156877093533586,
0.492926461251488));
#30017=CARTESIAN_POINT('Ctrl Pts',(-0.180361659008724,0.0998164645468222,
0.49663267524586));
#30018=CARTESIAN_POINT('Ctrl Pts',(-0.192338886510923,0.0362281355122108,
0.500338889240232));
#30019=CARTESIAN_POINT('Ctrl Pts',(-0.194573194011967,0.0243659678682544,
0.501030269756014));
#30020=CARTESIAN_POINT('Ctrl Pts',(-0.195601481281436,0.0122766393772507,
0.501721650271795));
#30021=CARTESIAN_POINT('Ctrl Pts',(-0.195491180920002,0.000168629508682236,
0.502413030787576));
#30022=CARTESIAN_POINT('Origin',(0.,0.,0.));
#30023=CARTESIAN_POINT('',(-0.19507978584999,-3.45334863967226E-6,0.582586969212423));
#30024=CARTESIAN_POINT('',(-0.195080468396925,1.8981806121043E-5,0.572413030787576));
#30025=CARTESIAN_POINT('',(-0.1954,-2.39295984553393E-17,0.));
#30026=CARTESIAN_POINT('Ctrl Pts',(-0.195079815420139,-3.45302974047446E-6,
0.582586969212423));
#30027=CARTESIAN_POINT('Ctrl Pts',(-0.195074640707532,0.0328120037045956,
0.580723147606333));
#30028=CARTESIAN_POINT('Ctrl Pts',(-0.187237758907749,0.0656297824114404,
0.578859326000243));
#30029=CARTESIAN_POINT('Ctrl Pts',(-0.1715829951129,0.0941574404236039,
0.576995504394152));
#30030=CARTESIAN_POINT('Ctrl Pts',(-0.14047439120071,0.150846613462089,
0.573291782711304));
#30031=CARTESIAN_POINT('Ctrl Pts',(-0.0784943311216198,0.190594846094957,
0.569588061028457));
#30032=CARTESIAN_POINT('Ctrl Pts',(-0.0139960769924853,0.195218999146749,
0.565884339345609));
#30033=CARTESIAN_POINT('Ctrl Pts',(0.0505021771366483,0.199843152198542,
0.562180617662761));
#30034=CARTESIAN_POINT('Ctrl Pts',(0.117518625315826,0.169343225669258,
0.558476895979913));
#30035=CARTESIAN_POINT('Ctrl Pts',(0.156396070392606,0.117671648942254,
0.554773174297065));
#30036=CARTESIAN_POINT('Ctrl Pts',(0.195273515469386,0.0660000722152496,
0.551069452614217));
#30037=CARTESIAN_POINT('Ctrl Pts',(0.206011957443768,-0.00684315470947738,
0.547365730931369));
#30038=CARTESIAN_POINT('Ctrl Pts',(0.183699012241942,-0.0675353292756691,
0.543662009248521));
#30039=CARTESIAN_POINT('Ctrl Pts',(0.161386067040115,-0.128227503841861,
0.539958287565673));
#30040=CARTESIAN_POINT('Ctrl Pts',(0.106021734662079,-0.176768626049519,
0.536254565882826));
#30041=CARTESIAN_POINT('Ctrl Pts',(0.0429328609649713,-0.190953180775813,
0.532550844199978));
#30042=CARTESIAN_POINT('Ctrl Pts',(-0.0201560127321352,-0.205137735502108,
0.52884712251713));
#30043=CARTESIAN_POINT('Ctrl Pts',(-0.0909694277483132,-0.184965722747041,
0.525143400834282));
#30044=CARTESIAN_POINT('Ctrl Pts',(-0.137113234823603,-0.139664987148696,
0.521439679151434));
#30045=CARTESIAN_POINT('Ctrl Pts',(-0.173877852911313,-0.103572077852157,
0.51848877583843));
#30046=CARTESIAN_POINT('Ctrl Pts',(-0.194982335358017,-0.0515275892214865,
0.515537872525427));
#30047=CARTESIAN_POINT('Ctrl Pts',(-0.195458266482996,0.000173443779922018,
0.512586969212423));
#30048=CARTESIAN_POINT('Ctrl Pts',(-0.195491180920002,0.000168629508682236,
0.502413030787576));
#30049=CARTESIAN_POINT('Ctrl Pts',(-0.195010205227512,-0.0526295513449078,
0.505427864266167));
#30050=CARTESIAN_POINT('Ctrl Pts',(-0.172879182329996,-0.105782955367232,
0.508442697744757));
#30051=CARTESIAN_POINT('Ctrl Pts',(-0.134689356786549,-0.142005289462677,
0.511457531223348));
#30052=CARTESIAN_POINT('Ctrl Pts',(-0.0877416010060499,-0.186534356320495,
0.51516374521772));
#30053=CARTESIAN_POINT('Ctrl Pts',(-0.0165250908911267,-0.205476460953673,
0.518869959212092));
#30054=CARTESIAN_POINT('Ctrl Pts',(0.0463414671012952,-0.190155708549211,
0.522576173206464));
#30055=CARTESIAN_POINT('Ctrl Pts',(0.109208025093718,-0.174834956144749,
0.526282387200837));
#30056=CARTESIAN_POINT('Ctrl Pts',(0.163724630963639,-0.125251346702646,
0.529988601195209));
#30057=CARTESIAN_POINT('Ctrl Pts',(0.184921496651671,-0.0641152489120857,
0.533694815189581));
#30058=CARTESIAN_POINT('Ctrl Pts',(0.206118362339704,-0.00297915112152539,
0.537401029183953));
#30059=CARTESIAN_POINT('Ctrl Pts',(0.193995487845847,0.0697094350174917,
0.541107243178325));
#30060=CARTESIAN_POINT('Ctrl Pts',(0.154105412656959,0.120657560296821,
0.544813457172697));
#30061=CARTESIAN_POINT('Ctrl Pts',(0.114215337468071,0.171605685576151,
0.548519671167069));
#30062=CARTESIAN_POINT('Ctrl Pts',(0.0465580615841514,0.200813349995792,
0.552225885161441));
#30063=CARTESIAN_POINT('Ctrl Pts',(-0.0178779150223708,0.194902809680635,
0.555932099155813));
#30064=CARTESIAN_POINT('Ctrl Pts',(-0.0823138916288934,0.188992269365477,
0.559638313150186));
#30065=CARTESIAN_POINT('Ctrl Pts',(-0.143528568958019,0.14796352431552,
0.563344527144558));
#30066=CARTESIAN_POINT('Ctrl Pts',(-0.173484296927877,0.0906086297567353,
0.56705074113893));
#30067=CARTESIAN_POINT('Ctrl Pts',(-0.187931321146693,0.0629475576708828,
0.568838171021812));
#30068=CARTESIAN_POINT('Ctrl Pts',(-0.195107725773013,0.031489133949035,
0.570625600904694));
#30069=CARTESIAN_POINT('Ctrl Pts',(-0.195080468396925,1.8981806121043E-5,
0.572413030787576));
#30070=CARTESIAN_POINT('Origin',(0.,0.,0.));
#30071=CARTESIAN_POINT('',(-0.195470932084261,-0.000171584046685047,0.652586969212424));
#30072=CARTESIAN_POINT('',(-0.195421427783755,-0.000177812761388513,0.642413030787576));
#30073=CARTESIAN_POINT('',(-0.1954,-2.39295984553393E-17,0.));
#30074=CARTESIAN_POINT('Ctrl Pts',(-0.195470932084261,-0.000171584046685047,
0.652586969212424));
#30075=CARTESIAN_POINT('Ctrl Pts',(-0.194992946923152,0.0519398730151351,
0.649612144370087));
#30076=CARTESIAN_POINT('Ctrl Pts',(-0.173506994162404,0.104399306729571,
0.64663731952775));
#30077=CARTESIAN_POINT('Ctrl Pts',(-0.136210733975536,0.140545308526766,
0.643662494685414));
#30078=CARTESIAN_POINT('Ctrl Pts',(-0.0897760782010601,0.185547867567989,
0.639958773002566));
#30079=CARTESIAN_POINT('Ctrl Pts',(-0.0188341937200331,0.205263315093338,
0.636255051319719));
#30080=CARTESIAN_POINT('Ctrl Pts',(0.0441620008484366,0.190672665791667,
0.632551329636871));
#30081=CARTESIAN_POINT('Ctrl Pts',(0.107158195416906,0.176082016489995,
0.628847607954023));
#30082=CARTESIAN_POINT('Ctrl Pts',(0.162208700072817,0.127185270361303,
0.625143886271175));
#30083=CARTESIAN_POINT('Ctrl Pts',(0.184130231899333,0.0663506254660481,
0.621440164588327));
#30084=CARTESIAN_POINT('Ctrl Pts',(0.20605176372585,0.00551598057079281,
0.617736442905479));
#30085=CARTESIAN_POINT('Ctrl Pts',(0.194844322722972,-0.0672565630910262,
0.614032721222632));
#30086=CARTESIAN_POINT('Ctrl Pts',(0.155634840229719,-0.118676637573315,
0.610328999539784));
#30087=CARTESIAN_POINT('Ctrl Pts',(0.116425357736466,-0.170096712055603,
0.606625277856936));
#30088=CARTESIAN_POINT('Ctrl Pts',(0.0492138337528384,-0.200164317358361,
0.602921556174087));
#30089=CARTESIAN_POINT('Ctrl Pts',(-0.0152532956197894,-0.195124792816734,
0.59921783449124));
#30090=CARTESIAN_POINT('Ctrl Pts',(-0.0797204249924167,-0.190085268275106,
0.595514112808392));
#30091=CARTESIAN_POINT('Ctrl Pts',(-0.141443159754043,-0.149938613889095,
0.591810391125544));
#30092=CARTESIAN_POINT('Ctrl Pts',(-0.172185953262212,-0.0930502299740384,
0.588106669442696));
#30093=CARTESIAN_POINT('Ctrl Pts',(-0.187458069522289,-0.0647897528391999,
0.586266769365939));
#30094=CARTESIAN_POINT('Ctrl Pts',(-0.195084923717034,-0.0323977343102287,
0.584426869289181));
#30095=CARTESIAN_POINT('Ctrl Pts',(-0.195079815420139,-3.45302974047446E-6,
0.582586969212423));
#30096=CARTESIAN_POINT('Ctrl Pts',(-0.195080468396925,1.8981806121043E-5,
0.572413030787576));
#30097=CARTESIAN_POINT('Ctrl Pts',(-0.195051207937167,-0.0337638415069996,
0.574331814899066));
#30098=CARTESIAN_POINT('Ctrl Pts',(-0.186720620393942,-0.0675601803708791,
0.576250599010555));
#30099=CARTESIAN_POINT('Ctrl Pts',(-0.170171536425399,-0.0966869859783203,
0.578169383122045));
#30100=CARTESIAN_POINT('Ctrl Pts',(-0.138206269342473,-0.15294666308698,
0.581875597116418));
#30101=CARTESIAN_POINT('Ctrl Pts',(-0.0755789565660301,-0.191784973236686,
0.585581811110791));
#30102=CARTESIAN_POINT('Ctrl Pts',(-0.0109742658556152,-0.195413127900566,
0.589288025105163));
#30103=CARTESIAN_POINT('Ctrl Pts',(0.0536304248547996,-0.199041282564447,
0.592994239099535));
#30104=CARTESIAN_POINT('Ctrl Pts',(0.120212493499187,-0.1674592817425,0.596700453093906));
#30105=CARTESIAN_POINT('Ctrl Pts',(0.158275908344154,-0.115132366886058,
0.600406667088278));
#30106=CARTESIAN_POINT('Ctrl Pts',(0.19633932318912,-0.0628054520296152,
0.60411288108265));
#30107=CARTESIAN_POINT('Ctrl Pts',(0.205884084234667,0.0102663768613233,
0.607819095077022));
#30108=CARTESIAN_POINT('Ctrl Pts',(0.182538483877546,0.0706146370849535,
0.611525309071394));
#30109=CARTESIAN_POINT('Ctrl Pts',(0.159192883520425,0.130962897308584,
0.615231523065767));
#30110=CARTESIAN_POINT('Ctrl Pts',(0.102956921760636,0.178587588864905,
0.618937737060139));
#30111=CARTESIAN_POINT('Ctrl Pts',(0.0395878889512919,0.191675569949154,
0.622643951054511));
#30112=CARTESIAN_POINT('Ctrl Pts',(-0.0237811438580523,0.204763551033402,
0.626350165048883));
#30113=CARTESIAN_POINT('Ctrl Pts',(-0.0942832477169518,0.183314821645578,
0.630056379043255));
#30114=CARTESIAN_POINT('Ctrl Pts',(-0.139626929730598,0.137153365109863,
0.633762593037627));
#30115=CARTESIAN_POINT('Ctrl Pts',(-0.17490486198241,0.101239194403086,
0.63664607228761));
#30116=CARTESIAN_POINT('Ctrl Pts',(-0.194954331224527,0.0503663409317413,
0.639529551537593));
#30117=CARTESIAN_POINT('Ctrl Pts',(-0.195421427783755,-0.000177812761388513,
0.642413030787576));
#30118=CARTESIAN_POINT('Origin',(0.,0.,0.));
#30119=CARTESIAN_POINT('',(-0.195636369417486,0.000113518110994186,0.722586969212423));
#30120=CARTESIAN_POINT('',(-0.195675615924934,8.51174274233985E-5,0.712413030787576));
#30121=CARTESIAN_POINT('',(-0.1954,-2.39295984553393E-17,0.));
#30122=CARTESIAN_POINT('Ctrl Pts',(-0.195636369417486,0.000113518110994186,
0.722586969212423));
#30123=CARTESIAN_POINT('Ctrl Pts',(-0.195682546989371,0.00679235189129894,
0.722204862816689));
#30124=CARTESIAN_POINT('Ctrl Pts',(-0.195370156992351,0.0134668159558925,
0.721822756420955));
#30125=CARTESIAN_POINT('Ctrl Pts',(-0.194684940168549,0.0201027826582277,
0.72144065002522));
#30126=CARTESIAN_POINT('Ctrl Pts',(-0.188043197355288,0.0844245894546327,
0.717736928342373));
#30127=CARTESIAN_POINT('Ctrl Pts',(-0.146373463610807,0.145129475044757,
0.714033206659525));
#30128=CARTESIAN_POINT('Ctrl Pts',(-0.0887378837876281,0.174447515831938,
0.710329484976677));
#30129=CARTESIAN_POINT('Ctrl Pts',(-0.031102303964449,0.203765556619118,
0.706625763293829));
#30130=CARTESIAN_POINT('Ctrl Pts',(0.0424991219374283,0.201696752603353,
0.702922041610981));
#30131=CARTESIAN_POINT('Ctrl Pts',(0.0983968473233738,0.169187494324663,
0.699218319928133));
#30132=CARTESIAN_POINT('Ctrl Pts',(0.154294572709319,0.136678236045973,
0.695514598245285));
#30133=CARTESIAN_POINT('Ctrl Pts',(0.192488597579333,0.0737285235043576,
0.691810876562437));
#30134=CARTESIAN_POINT('Ctrl Pts',(0.195506767226643,0.00913519390189264,
0.68810715487959));
#30135=CARTESIAN_POINT('Ctrl Pts',(0.198524936873952,-0.0554581357005719,
0.684403433196742));
#30136=CARTESIAN_POINT('Ctrl Pts',(0.166367251298559,-0.121695082363886,
0.680699711513894));
#30137=CARTESIAN_POINT('Ctrl Pts',(0.113744494695038,-0.159275037986524,
0.676995989831046));
#30138=CARTESIAN_POINT('Ctrl Pts',(0.0611217380915185,-0.196854993609162,
0.673292268148198));
#30139=CARTESIAN_POINT('Ctrl Pts',(-0.0119660895401274,-0.205777958191125,
0.669588546465349));
#30140=CARTESIAN_POINT('Ctrl Pts',(-0.072084391141631,-0.181962051958034,
0.665884824782502));
#30141=CARTESIAN_POINT('Ctrl Pts',(-0.132202692743136,-0.158146145724943,
0.662181103099654));
#30142=CARTESIAN_POINT('Ctrl Pts',(-0.179351468314497,-0.101591368676797,
0.658477381416807));
#30143=CARTESIAN_POINT('Ctrl Pts',(-0.191962142566216,-0.0381691448741754,
0.654773659733959));
#30144=CARTESIAN_POINT('Ctrl Pts',(-0.19444393828574,-0.0256875756563692,
0.654044762893447));
#30145=CARTESIAN_POINT('Ctrl Pts',(-0.195588048853217,-0.0129400253566584,
0.653315866052935));
#30146=CARTESIAN_POINT('Ctrl Pts',(-0.195470932084261,-0.000171584046685047,
0.652586969212424));
#30147=CARTESIAN_POINT('Ctrl Pts',(-0.195421427783755,-0.000177812761388513,
0.642413030787576));
#30148=CARTESIAN_POINT('Ctrl Pts',(-0.195554703085897,-0.0145994290672205,
0.643235765531965));
#30149=CARTESIAN_POINT('Ctrl Pts',(-0.194093747105224,-0.0289942854151266,
0.644058500276354));
#30150=CARTESIAN_POINT('Ctrl Pts',(-0.190937423221194,-0.0430072724152966,
0.644881235020743));
#30151=CARTESIAN_POINT('Ctrl Pts',(-0.17671897452975,-0.106132269721135,
0.648587449015115));
#30152=CARTESIAN_POINT('Ctrl Pts',(-0.128096816978468,-0.161508080649208,
0.652293663009487));
#30153=CARTESIAN_POINT('Ctrl Pts',(-0.067340953434779,-0.183771382585667,
0.65599987700386));
#30154=CARTESIAN_POINT('Ctrl Pts',(-0.00658508989108841,-0.206034684522128,
0.659706090998232));
#30155=CARTESIAN_POINT('Ctrl Pts',(0.06630447964501,-0.195185477466974,
0.663412304992604));
#30156=CARTESIAN_POINT('Ctrl Pts',(0.117942751209788,-0.156192933591821,
0.667118518986976));
#30157=CARTESIAN_POINT('Ctrl Pts',(0.169581022774564,-0.117200389716668,
0.670824732981348));
#30158=CARTESIAN_POINT('Ctrl Pts',(0.19996799636802,-0.0500645090215166,
0.67453094697572));
#30159=CARTESIAN_POINT('Ctrl Pts',(0.195185778931935,0.0144650188277344,
0.678237160970092));
#30160=CARTESIAN_POINT('Ctrl Pts',(0.190403561495849,0.0789945466769872,
0.681943374964464));
#30161=CARTESIAN_POINT('Ctrl Pts',(0.15045215303022,0.14091772168034,0.685649588958836));
#30162=CARTESIAN_POINT('Ctrl Pts',(0.0936301652358751,0.171872386452436,
0.689355802953208));
#30163=CARTESIAN_POINT('Ctrl Pts',(0.0368081774415317,0.202827051224532,
0.69306201694758));
#30164=CARTESIAN_POINT('Ctrl Pts',(-0.0368843896815252,0.202813205765373,
0.696768230941953));
#30165=CARTESIAN_POINT('Ctrl Pts',(-0.0936947418561655,0.171837191595589,
0.700474444936325));
#30166=CARTESIAN_POINT('Ctrl Pts',(-0.150505094030807,0.140861177425805,
0.704180658930697));
#30167=CARTESIAN_POINT('Ctrl Pts',(-0.190433231257031,0.078922994545395,
0.707886872925069));
#30168=CARTESIAN_POINT('Ctrl Pts',(-0.195191200566454,0.0143916742729559,
0.711593086919441));
#30169=CARTESIAN_POINT('Ctrl Pts',(-0.195542076848464,0.00963281429343837,
0.711866401542153));
#30170=CARTESIAN_POINT('Ctrl Pts',(-0.195701686505733,0.00485985200318871,
0.712139716164864));
#30171=CARTESIAN_POINT('Ctrl Pts',(-0.195675615924934,8.51174274233985E-5,
0.712413030787576));
#30172=CARTESIAN_POINT('Origin',(0.,0.,0.));
#30173=CARTESIAN_POINT('',(-0.195128545551857,9.80157954364874E-5,0.792586969212424));
#30174=CARTESIAN_POINT('',(-0.195166123101285,0.000126544742759004,0.782413030787576));
#30175=CARTESIAN_POINT('',(-0.1954,-2.39295984553393E-17,0.));
#30176=CARTESIAN_POINT('Ctrl Pts',(-0.195128545551857,9.80157954364874E-5,
0.792586969212424));
#30177=CARTESIAN_POINT('Ctrl Pts',(-0.195247914943593,0.0263701155015296,
0.791093859580443));
#30178=CARTESIAN_POINT('Ctrl Pts',(-0.190313505751618,0.0525992349613935,
0.789600749948463));
#30179=CARTESIAN_POINT('Ctrl Pts',(-0.180112460177197,0.0765888339627252,
0.788107640316483));
#30180=CARTESIAN_POINT('Ctrl Pts',(-0.154808334564134,0.136096050365993,
0.784403918633635));
#30181=CARTESIAN_POINT('Ctrl Pts',(-0.0970981193167941,0.181823294990903,
0.780700196950786));
#30182=CARTESIAN_POINT('Ctrl Pts',(-0.0333818027149729,0.192852282969788,
0.776996475267938));
#30183=CARTESIAN_POINT('Ctrl Pts',(0.0303345138868501,0.203881270948674,
0.773292753585091));
#30184=CARTESIAN_POINT('Ctrl Pts',(0.100056931843154,0.180212002281536,
0.769589031902244));
#30185=CARTESIAN_POINT('Ctrl Pts',(0.143890387011628,0.132672168613705,
0.765885310219396));
#30186=CARTESIAN_POINT('Ctrl Pts',(0.187723842180101,0.0851323349458752,
0.762181588536548));
#30187=CARTESIAN_POINT('Ctrl Pts',(0.205668334560742,0.013721936277351,
0.758477866853699));
#30188=CARTESIAN_POINT('Ctrl Pts',(0.18951501609247,-0.0488917833023672,
0.754774145170851));
#30189=CARTESIAN_POINT('Ctrl Pts',(0.173361697624198,-0.111505502882086,
0.751070423488003));
#30190=CARTESIAN_POINT('Ctrl Pts',(0.123110568307013,-0.165322543373001,
0.747366701805156));
#30191=CARTESIAN_POINT('Ctrl Pts',(0.061749399359133,-0.185723879665063,
0.743662980122308));
#30192=CARTESIAN_POINT('Ctrl Pts',(0.000388230411252383,-0.206125215957126,
0.73995925843946));
#30193=CARTESIAN_POINT('Ctrl Pts',(-0.072082978167322,-0.193110848050335,
0.736255536756612));
#30194=CARTESIAN_POINT('Ctrl Pts',(-0.122511706515588,-0.152634300095596,
0.732551815073764));
#30195=CARTESIAN_POINT('Ctrl Pts',(-0.16773779241913,-0.116333645789233,
0.72923019978665));
#30196=CARTESIAN_POINT('Ctrl Pts',(-0.195234952088687,-0.0579449614967985,
0.725908584499537));
#30197=CARTESIAN_POINT('Ctrl Pts',(-0.195636369417486,0.000113518110994186,
0.722586969212423));
#30198=CARTESIAN_POINT('Ctrl Pts',(-0.195675615924934,8.51174274233985E-5,
0.712413030787576));
#30199=CARTESIAN_POINT('Ctrl Pts',(-0.195348162971424,-0.0598867317271105,
0.715845930159236));
#30200=CARTESIAN_POINT('Ctrl Pts',(-0.165727828481393,-0.120138176331325,
0.719278829530897));
#30201=CARTESIAN_POINT('Ctrl Pts',(-0.117884051406102,-0.156237241050387,
0.722711728902558));
#30202=CARTESIAN_POINT('Ctrl Pts',(-0.0662311315437018,-0.195210378436822,
0.72641794289693));
#30203=CARTESIAN_POINT('Ctrl Pts',(0.00666250957372189,-0.206032195545224,
0.730124156891302));
#30204=CARTESIAN_POINT('Ctrl Pts',(0.0674100031098693,-0.183746065393738,
0.733830370885674));
#30205=CARTESIAN_POINT('Ctrl Pts',(0.128157496646017,-0.161459935242253,
0.737536584880046));
#30206=CARTESIAN_POINT('Ctrl Pts',(0.176758842600887,-0.10606585783088,
0.741242798874417));
#30207=CARTESIAN_POINT('Ctrl Pts',(0.19095357026966,-0.0429355222190436,
0.744949012868789));
#30208=CARTESIAN_POINT('Ctrl Pts',(0.205148297938434,0.0201948133927931,
0.748655226863161));
#30209=CARTESIAN_POINT('Ctrl Pts',(0.184936407321109,0.0910614072050953,
0.752361440857534));
#30210=CARTESIAN_POINT('Ctrl Pts',(0.139575382755531,0.137205822017881,
0.756067654851907));
#30211=CARTESIAN_POINT('Ctrl Pts',(0.0942143581899539,0.183350236830666,
0.759773868846279));
#30212=CARTESIAN_POINT('Ctrl Pts',(0.0237041996761252,0.204772472643938,
0.76348008284065));
#30213=CARTESIAN_POINT('Ctrl Pts',(-0.0396599106844383,0.191660680765389,
0.767186296835022));
#30214=CARTESIAN_POINT('Ctrl Pts',(-0.103024021045003,0.178548888886839,
0.770892510829394));
#30215=CARTESIAN_POINT('Ctrl Pts',(-0.159242083252301,0.130903069316467,
0.774598724823766));
#30216=CARTESIAN_POINT('Ctrl Pts',(-0.182565005336597,0.0705460409477194,
0.778304938818139));
#30217=CARTESIAN_POINT('Ctrl Pts',(-0.19118230851659,0.0482454556858425,
0.779674302807951));
#30218=CARTESIAN_POINT('Ctrl Pts',(-0.195308968355645,0.0242096139413284,
0.781043666797764));
#30219=CARTESIAN_POINT('Ctrl Pts',(-0.195166123101285,0.000126544742759004,
0.782413030787576));
#30220=CARTESIAN_POINT('Origin',(0.,0.,0.));
#30221=CARTESIAN_POINT('',(-0.195279013340439,-0.000168009551267251,0.862586969212423));
#30222=CARTESIAN_POINT('',(-0.195215444869335,-0.000150235120299324,0.852413030787576));
#30223=CARTESIAN_POINT('',(-0.1954,-2.39295984553393E-17,0.));
#30224=CARTESIAN_POINT('Ctrl Pts',(-0.195279013340439,-0.000168009551267251,
0.862586969212423));
#30225=CARTESIAN_POINT('Ctrl Pts',(-0.194903607268958,0.0455640131522026,
0.859982856344197));
#30226=CARTESIAN_POINT('Ctrl Pts',(-0.178871895344458,0.0915331173731693,
0.857378743475971));
#30227=CARTESIAN_POINT('Ctrl Pts',(-0.149539281844263,0.126270942713959,
0.854774630607745));
#30228=CARTESIAN_POINT('Ctrl Pts',(-0.107820722729247,0.175677110357261,
0.851070908924897));
#30229=CARTESIAN_POINT('Ctrl Pts',(-0.0391968436807465,0.202364430724413,
0.847367187242049));
#30230=CARTESIAN_POINT('Ctrl Pts',(0.024939826400162,0.194124580780539,
0.843663465559201));
#30231=CARTESIAN_POINT('Ctrl Pts',(0.0890764964810705,0.185884730836666,
0.839959743876352));
#30232=CARTESIAN_POINT('Ctrl Pts',(0.148725957594388,0.142717710581768,
0.836256022193505));
#30233=CARTESIAN_POINT('Ctrl Pts',(0.176601098282085,0.0843706103134459,
0.832552300510657));
#30234=CARTESIAN_POINT('Ctrl Pts',(0.204476238969783,0.0260235100451228,
0.828848578827809));
#30235=CARTESIAN_POINT('Ctrl Pts',(0.200577059231861,-0.0475036702366233,
0.825144857144961));
#30236=CARTESIAN_POINT('Ctrl Pts',(0.166687269277466,-0.102575348200379,
0.821441135462114));
#30237=CARTESIAN_POINT('Ctrl Pts',(0.132797479323072,-0.157647026164133,
0.817737413779266));
#30238=CARTESIAN_POINT('Ctrl Pts',(0.0689170791522051,-0.194263201809897,
0.814033692096418));
#30239=CARTESIAN_POINT('Ctrl Pts',(0.00426865627857745,-0.195673519857469,
0.81032997041357));
#30240=CARTESIAN_POINT('Ctrl Pts',(-0.060379766595052,-0.197083837905041,
0.806626248730722));
#30241=CARTESIAN_POINT('Ctrl Pts',(-0.125796212171444,-0.16328829835442,
0.802922527047874));
#30242=CARTESIAN_POINT('Ctrl Pts',(-0.162055416970245,-0.109746934488294,
0.799218805365026));
#30243=CARTESIAN_POINT('Ctrl Pts',(-0.183697171385623,-0.0777901098892797,
0.797008193314158));
#30244=CARTESIAN_POINT('Ctrl Pts',(-0.194951814111497,-0.0387989405753114,
0.794797581263291));
#30245=CARTESIAN_POINT('Ctrl Pts',(-0.195128545551857,9.80157954364874E-5,
0.792586969212424));
#30246=CARTESIAN_POINT('Ctrl Pts',(-0.195166123101285,0.000126544742759004,
0.782413030787576));
#30247=CARTESIAN_POINT('Ctrl Pts',(-0.194922354508138,-0.0409717467160323,
0.784749880792136));
#30248=CARTESIAN_POINT('Ctrl Pts',(-0.182244856716882,-0.0822075748123473,
0.787086730796695));
#30249=CARTESIAN_POINT('Ctrl Pts',(-0.158232634722073,-0.115191832939155,
0.789423580801255));
#30250=CARTESIAN_POINT('Ctrl Pts',(-0.120149560061961,-0.167504441290151,
0.793129794795627));
#30251=CARTESIAN_POINT('Ctrl Pts',(-0.0535556287804454,-0.199061420825021,
0.796836008789999));
#30252=CARTESIAN_POINT('Ctrl Pts',(0.0110476940437387,-0.195408990384897,
0.800542222784371));
#30253=CARTESIAN_POINT('Ctrl Pts',(0.0756510168679237,-0.191756559944773,
0.804248436778743));
#30254=CARTESIAN_POINT('Ctrl Pts',(0.138263731234777,-0.152894719529654,
0.807954650773115));
#30255=CARTESIAN_POINT('Ctrl Pts',(0.170207855773424,-0.0966230350379699,
0.811660864767488));
#30256=CARTESIAN_POINT('Ctrl Pts',(0.202151980312072,-0.0403513505462853,
0.81536707876186));
#30257=CARTESIAN_POINT('Ctrl Pts',(0.203427515022513,0.0333301780219651,
0.819073292756232));
#30258=CARTESIAN_POINT('Ctrl Pts',(0.173450237337761,0.0906738122863988,
0.822779506750604));
#30259=CARTESIAN_POINT('Ctrl Pts',(0.143472959653009,0.148017446550833,
0.826485720744976));
#30260=CARTESIAN_POINT('Ctrl Pts',(0.0822428695730641,0.189023186511451,
0.830191934739348));
#30261=CARTESIAN_POINT('Ctrl Pts',(0.0178046765554912,0.194909513773745,
0.83389814873372));
#30262=CARTESIAN_POINT('Ctrl Pts',(-0.0466335164620799,0.200795841036038,
0.837604362728092));
#30263=CARTESIAN_POINT('Ctrl Pts',(-0.114279812417278,0.171562755600011,
0.841310576722464));
#30264=CARTESIAN_POINT('Ctrl Pts',(-0.154150740386038,0.120599644714809,
0.845016790716836));
#30265=CARTESIAN_POINT('Ctrl Pts',(-0.180673309918174,0.0866984359672774,
0.84748220407375));
#30266=CARTESIAN_POINT('Ctrl Pts',(-0.194905131081074,0.0431815751432988,
0.849947617430663));
#30267=CARTESIAN_POINT('Ctrl Pts',(-0.195215444869335,-0.000150235120299324,
0.852413030787576));
#30268=CARTESIAN_POINT('Origin',(0.,0.,0.));
#30269=CARTESIAN_POINT('',(-0.195719986784682,3.71606954582295E-6,0.932586969212424));
#30270=CARTESIAN_POINT('',(-0.195707453392556,-4.66568259871601E-5,0.922413030787576));
#30271=CARTESIAN_POINT('',(-0.1954,-2.39295984553393E-17,0.));
#30272=CARTESIAN_POINT('Ctrl Pts',(-0.195719986784682,3.71606954582295E-6,
0.932586969212424));
#30273=CARTESIAN_POINT('Ctrl Pts',(-0.195738156138108,0.0648665395087412,
0.928871853107952));
#30274=CARTESIAN_POINT('Ctrl Pts',(-0.160275715576186,0.129712057687137,
0.925156737003479));
#30275=CARTESIAN_POINT('Ctrl Pts',(-0.10568144211536,0.164735485073218,
0.921441620899007));
#30276=CARTESIAN_POINT('Ctrl Pts',(-0.0512546116502832,0.199651494094127,
0.917737899216159));
#30277=CARTESIAN_POINT('Ctrl Pts',(0.0221865722997436,0.204928064005996,
0.914034177533311));
#30278=CARTESIAN_POINT('Ctrl Pts',(0.0810458692323854,0.178151382429043,
0.910330455850463));
#30279=CARTESIAN_POINT('Ctrl Pts',(0.139905166165026,0.151374700852089,
0.906626734167615));
#30280=CARTESIAN_POINT('Ctrl Pts',(0.184182576080283,0.0925447677863139,
0.902923012484767));
#30281=CARTESIAN_POINT('Ctrl Pts',(0.193623051178265,0.0285737974246437,
0.899219290801919));
#30282=CARTESIAN_POINT('Ctrl Pts',(0.203063526276248,-0.0353971729370283,
0.895515569119071));
#30283=CARTESIAN_POINT('Ctrl Pts',(0.177667066556955,-0.104509180594595,
0.891811847436224));
#30284=CARTESIAN_POINT('Ctrl Pts',(0.129051481285208,-0.147146399547075,
0.888108125753376));
#30285=CARTESIAN_POINT('Ctrl Pts',(0.0804358960134615,-0.189783618499555,
0.884404404070528));
#30286=CARTESIAN_POINT('Ctrl Pts',(0.00860118518926115,-0.205946048746948,
0.88070068238768));
#30287=CARTESIAN_POINT('Ctrl Pts',(-0.0535913025040727,-0.188240059832962,
0.876996960704832));
#30288=CARTESIAN_POINT('Ctrl Pts',(-0.115783790197406,-0.170534070918976,
0.873293239021984));
#30289=CARTESIAN_POINT('Ctrl Pts',(-0.168334054759872,-0.118959662843613,
0.869589517339136));
#30290=CARTESIAN_POINT('Ctrl Pts',(-0.187202567450341,-0.0571099513462054,
0.865885795656288));
#30291=CARTESIAN_POINT('Ctrl Pts',(-0.192804495632289,-0.0387472087407564,
0.864786186841667));
#30292=CARTESIAN_POINT('Ctrl Pts',(-0.195437531748109,-0.0194787452297348,
0.863686578027045));
#30293=CARTESIAN_POINT('Ctrl Pts',(-0.195279013340439,-0.000168009551267251,
0.862586969212423));
#30294=CARTESIAN_POINT('Ctrl Pts',(-0.195215444869335,-0.000150235120299324,
0.852413030787576));
#30295=CARTESIAN_POINT('Ctrl Pts',(-0.195371620524508,-0.021958398707372,
0.853653831425035));
#30296=CARTESIAN_POINT('Ctrl Pts',(-0.192001564940553,-0.0437196901383431,
0.854894632062494));
#30297=CARTESIAN_POINT('Ctrl Pts',(-0.184897391479539,-0.0641847309864828,
0.856135432699953));
#30298=CARTESIAN_POINT('Ctrl Pts',(-0.163677554621959,-0.125312859468192,
0.859841646694325));
#30299=CARTESIAN_POINT('Ctrl Pts',(-0.10914232092448,-0.174875980097234,
0.863547860688697));
#30300=CARTESIAN_POINT('Ctrl Pts',(-0.0462700104058479,-0.190173108515756,
0.867254074683069));
#30301=CARTESIAN_POINT('Ctrl Pts',(0.0166023001127845,-0.205470236934278,
0.870960288677441));
#30302=CARTESIAN_POINT('Ctrl Pts',(0.0878116874525705,-0.186501373142281,
0.874666502671813));
#30303=CARTESIAN_POINT('Ctrl Pts',(0.134742707561642,-0.141954668207959,
0.878372716666185));
#30304=CARTESIAN_POINT('Ctrl Pts',(0.181673727670714,-0.0974079632736377,
0.882078930660557));
#30305=CARTESIAN_POINT('Ctrl Pts',(0.204326380549072,-0.0272834171969915,
0.885785144654929));
#30306=CARTESIAN_POINT('Ctrl Pts',(0.192325259761237,0.0363004067433246,
0.889491358649301));
#30307=CARTESIAN_POINT('Ctrl Pts',(0.180324138973402,0.0998842306836407,
0.893197572643673));
#30308=CARTESIAN_POINT('Ctrl Pts',(0.133669244519374,0.156927332487627,
0.896903786638045));
#30309=CARTESIAN_POINT('Ctrl Pts',(0.0737295301650971,0.181302734225987,
0.900610000632418));
#30310=CARTESIAN_POINT('Ctrl Pts',(0.0137898158108199,0.205678135964346,
0.90431621462679));
#30311=CARTESIAN_POINT('Ctrl Pts',(-0.059434718443707,0.19738583763708,
0.908022428621162));
#30312=CARTESIAN_POINT('Ctrl Pts',(-0.112405647662483,0.160223891616111,
0.911728642615534));
#30313=CARTESIAN_POINT('Ctrl Pts',(-0.163307724594775,0.124513356361944,
0.915290105339548));
#30314=CARTESIAN_POINT('Ctrl Pts',(-0.195507366281261,0.0621442230158499,
0.918851568063562));
#30315=CARTESIAN_POINT('Ctrl Pts',(-0.195707453392556,-4.66568259871601E-5,
0.922413030787576));
#30316=CARTESIAN_POINT('Origin',(0.,0.,0.));
#30317=CARTESIAN_POINT('',(-0.195268202714777,0.000165579016441021,1.00258696921242));
#30318=CARTESIAN_POINT('',(-0.19535343393295,0.000178280253715055,0.992413030787576));
#30319=CARTESIAN_POINT('',(-0.1954,-2.39295984553393E-17,0.));
#30320=CARTESIAN_POINT('Ctrl Pts',(-0.195268202714777,0.000165579016441021,
1.00258696921242));
#30321=CARTESIAN_POINT('Ctrl Pts',(-0.19542709496717,0.0198793394721131,
1.00146457155455));
#30322=CARTESIAN_POINT('Ctrl Pts',(-0.192681564478375,0.0395498739780043,
1.00034217389668));
#30323=CARTESIAN_POINT('Ctrl Pts',(-0.186848643290836,0.0582577638715851,
0.999219776238813));
#30324=CARTESIAN_POINT('Ctrl Pts',(-0.167600993827966,0.11999062383733,
0.995516054555966));
#30325=CARTESIAN_POINT('Ctrl Pts',(-0.114735119634562,0.171241362792136,
0.991812332873117));
#30326=CARTESIAN_POINT('Ctrl Pts',(-0.0524351231736321,0.18856531990772,
0.988108611190269));
#30327=CARTESIAN_POINT('Ctrl Pts',(0.00986487328729629,0.205889277023303,
0.984404889507421));
#30328=CARTESIAN_POINT('Ctrl Pts',(0.0815989920157509,0.189286452299667,
0.980701167824573));
#30329=CARTESIAN_POINT('Ctrl Pts',(0.129952003507049,0.146351732792493,
0.976997446141725));
#30330=CARTESIAN_POINT('Ctrl Pts',(0.178305014998348,0.103417013285319,
0.973293724458878));
#30331=CARTESIAN_POINT('Ctrl Pts',(0.20327691925249,0.0341503989946047,
0.969590002776029));
#30332=CARTESIAN_POINT('Ctrl Pts',(0.19344406978275,-0.0297614493697593,
0.965886281093181));
#30333=CARTESIAN_POINT('Ctrl Pts',(0.18361122031301,-0.0936732977341234,
0.962182559410334));
#30334=CARTESIAN_POINT('Ctrl Pts',(0.138973617119388,-0.152230380172138,
0.958478837727486));
#30335=CARTESIAN_POINT('Ctrl Pts',(0.0799511084736072,-0.178645358874384,
0.954775116044638));
#30336=CARTESIAN_POINT('Ctrl Pts',(0.0209285998278261,-0.20506033757663,
0.95107139436179));
#30337=CARTESIAN_POINT('Ctrl Pts',(-0.0524788142701144,-0.199333212543108,
0.947367672678942));
#30338=CARTESIAN_POINT('Ctrl Pts',(-0.106690354347858,-0.16408387214268,
0.943663950996094));
#30339=CARTESIAN_POINT('Ctrl Pts',(-0.160735113766186,-0.128942975594381,
0.93997162373487));
#30340=CARTESIAN_POINT('Ctrl Pts',(-0.195701928883641,-0.0644612332051665,
0.936279296473647));
#30341=CARTESIAN_POINT('Ctrl Pts',(-0.195719986784682,3.71606954582295E-6,
0.932586969212424));
#30342=CARTESIAN_POINT('Ctrl Pts',(-0.195707453392556,-4.66568259871601E-5,
0.922413030787576));
#30343=CARTESIAN_POINT('Ctrl Pts',(-0.195715585687005,-0.00257432861687418,
0.922557782057934));
#30344=CARTESIAN_POINT('Ctrl Pts',(-0.195670857405051,-0.00510170594794435,
0.922702533328292));
#30345=CARTESIAN_POINT('Ctrl Pts',(-0.195572375776859,-0.00762698699047084,
0.92284728459865));
#30346=CARTESIAN_POINT('Ctrl Pts',(-0.193050850489432,-0.0722843258614067,
0.926553498593022));
#30347=CARTESIAN_POINT('Ctrl Pts',(-0.155290475731554,-0.135567409888606,
0.930259712587394));
#30348=CARTESIAN_POINT('Ctrl Pts',(-0.0995863227266852,-0.168491214354887,
0.933965926581766));
#30349=CARTESIAN_POINT('Ctrl Pts',(-0.0438821697218168,-0.201415018821168,
0.937672140576139));
#30350=CARTESIAN_POINT('Ctrl Pts',(0.0297657615300397,-0.203979543726533,
0.94137835457051));
#30351=CARTESIAN_POINT('Ctrl Pts',(0.0876251218790847,-0.175010180082627,
0.945084568564882));
#30352=CARTESIAN_POINT('Ctrl Pts',(0.145484482228131,-0.146040816438721,
0.948790782559255));
#30353=CARTESIAN_POINT('Ctrl Pts',(0.187555271674363,-0.0855375642455424,
0.952496996553627));
#30354=CARTESIAN_POINT('Ctrl Pts',(0.194568154283725,-0.021212227253196,
0.956203210547999));
#30355=CARTESIAN_POINT('Ctrl Pts',(0.201581036893087,0.0431131097391505,
0.959909424542371));
#30356=CARTESIAN_POINT('Ctrl Pts',(0.173536012665579,0.111260531530666,
0.963615638536743));
#30357=CARTESIAN_POINT('Ctrl Pts',(0.123278314419194,0.152017044141902,
0.967321852531115));
#30358=CARTESIAN_POINT('Ctrl Pts',(0.0730206161728088,0.192773556753138,
0.971028066525487));
#30359=CARTESIAN_POINT('Ctrl Pts',(0.000550243907548716,0.206139160184095,
0.974734280519859));
#30360=CARTESIAN_POINT('Ctrl Pts',(-0.0609398062732146,0.185992111567971,
0.978440494514231));
#30361=CARTESIAN_POINT('Ctrl Pts',(-0.122429856453979,0.165845062951848,
0.982146708508603));
#30362=CARTESIAN_POINT('Ctrl Pts',(-0.172939584550245,0.112185362288641,
0.985852922502976));
#30363=CARTESIAN_POINT('Ctrl Pts',(-0.189334427223443,0.0495903289718102,
0.989559136497348));
#30364=CARTESIAN_POINT('Ctrl Pts',(-0.193542598326109,0.0335236538822793,
0.990510434594091));
#30365=CARTESIAN_POINT('Ctrl Pts',(-0.195503184094814,0.0168682937546108,
0.991461732690834));
#30366=CARTESIAN_POINT('Ctrl Pts',(-0.19535343393295,0.000178280253715055,
0.992413030787576));
#30367=CARTESIAN_POINT('Origin',(0.,0.,0.));
#30368=CARTESIAN_POINT('',(-0.195129684289216,-0.000113636086278679,1.07258696921242));
#30369=CARTESIAN_POINT('',(-0.195093054978418,-5.50606481354719E-5,1.06241303078758));
#30370=CARTESIAN_POINT('',(-0.1954,-2.39295984553393E-17,0.));
#30371=CARTESIAN_POINT('Ctrl Pts',(-0.195129684289216,-0.000113636086278679,
1.07258696921242));
#30372=CARTESIAN_POINT('Ctrl Pts',(-0.194942963316978,0.0391854106201406,
1.07035356831831));
#30373=CARTESIAN_POINT('Ctrl Pts',(-0.183442754086643,0.0785903964976412,
1.06812016742419));
#30374=CARTESIAN_POINT('Ctrl Pts',(-0.161381630858742,0.110744756631717,
1.06588676653008));
#30375=CARTESIAN_POINT('Ctrl Pts',(-0.124796949325566,0.164067382739912,
1.06218304484723));
#30376=CARTESIAN_POINT('Ctrl Pts',(-0.0591690439027595,0.197450300329055,
1.05847932316438));
#30377=CARTESIAN_POINT('Ctrl Pts',(0.00547076636758263,0.195640786233593,
1.05477560148153));
#30378=CARTESIAN_POINT('Ctrl Pts',(0.0701105766379276,0.19383127213813,
1.05107187979868));
#30379=CARTESIAN_POINT('Ctrl Pts',(0.133762291755807,0.156829326358058,
1.04736815811584));
#30380=CARTESIAN_POINT('Ctrl Pts',(0.167312833478204,0.101552035674769,
1.04366443643299));
#30381=CARTESIAN_POINT('Ctrl Pts',(0.200863375200599,0.0462747449914819,
1.03996071475014));
#30382=CARTESIAN_POINT('Ctrl Pts',(0.204312743527515,-0.0272778905950186,
1.03625699306729));
#30383=CARTESIAN_POINT('Ctrl Pts',(0.17608042651717,-0.0854535269464722,
1.03255327138444));
#30384=CARTESIAN_POINT('Ctrl Pts',(0.147848109506825,-0.143629163297926,
1.0288495497016));
#30385=CARTESIAN_POINT('Ctrl Pts',(0.0879341071592168,-0.186427800414334,
1.02514582801875));
#30386=CARTESIAN_POINT('Ctrl Pts',(0.0237478981470821,-0.194273555725334,
1.0214421063359));
#30387=CARTESIAN_POINT('Ctrl Pts',(-0.0404383108650536,-0.202119311036335,
1.01773838465305));
#30388=CARTESIAN_POINT('Ctrl Pts',(-0.108896726541717,-0.175012184541928,
1.0140346629702));
#30389=CARTESIAN_POINT('Ctrl Pts',(-0.15031122201388,-0.125351130806383,
1.01033094128736));
#30390=CARTESIAN_POINT('Ctrl Pts',(-0.17917522457641,-0.0907396556226723,
1.00774961726238));
#30391=CARTESIAN_POINT('Ctrl Pts',(-0.194902777514884,-0.0451727225472274,
1.0051682932374));
#30392=CARTESIAN_POINT('Ctrl Pts',(-0.195268202714777,0.000165579016441021,
1.00258696921242));
#30393=CARTESIAN_POINT('Ctrl Pts',(-0.19535343393295,0.000178280253715055,
0.992413030787576));
#30394=CARTESIAN_POINT('Ctrl Pts',(-0.194919764294582,-0.0481552375812319,
0.995167946685205));
#30395=CARTESIAN_POINT('Ctrl Pts',(-0.176787653021499,-0.0967793777264111,
0.997922862582834));
#30396=CARTESIAN_POINT('Ctrl Pts',(-0.144290486192301,-0.132238333502052,
1.00067777848046));
#30397=CARTESIAN_POINT('Ctrl Pts',(-0.100571745237828,-0.179941596688631,
1.00438399247484));
#30398=CARTESIAN_POINT('Ctrl Pts',(-0.0308543060787511,-0.203817757091334,
1.00809020646921));
#30399=CARTESIAN_POINT('Ctrl Pts',(0.0329297761185238,-0.192930969998698,
1.01179642046358));
#30400=CARTESIAN_POINT('Ctrl Pts',(0.0967138583157977,-0.182044182906063,
1.01550263445795));
#30401=CARTESIAN_POINT('Ctrl Pts',(0.15456458355127,-0.136394448318089,
1.01920884845232));
#30402=CARTESIAN_POINT('Ctrl Pts',(0.179984980484802,-0.076890421197536,
1.0229150624467));
#30403=CARTESIAN_POINT('Ctrl Pts',(0.205405377418334,-0.0173863940769825,
1.02662127644107));
#30404=CARTESIAN_POINT('Ctrl Pts',(0.198395446049928,0.05597192557615,1.03032749043544));
#30405=CARTESIAN_POINT('Ctrl Pts',(0.162166047466929,0.109585000349956,
1.03403370442981));
#30406=CARTESIAN_POINT('Ctrl Pts',(0.12593664888393,0.163198075123761,1.03773991842419));
#30407=CARTESIAN_POINT('Ctrl Pts',(0.0604877830863377,0.19706590501824,
1.04144613241856));
#30408=CARTESIAN_POINT('Ctrl Pts',(-0.0042038551539475,0.195675976549601,
1.04515234641293));
#30409=CARTESIAN_POINT('Ctrl Pts',(-0.0688954933942345,0.194286048080962,
1.0488585604073));
#30410=CARTESIAN_POINT('Ctrl Pts',(-0.132829904077215,0.157638361249205,
1.05256477440167));
#30411=CARTESIAN_POINT('Ctrl Pts',(-0.166723158702796,0.102518946943711,
1.05627098839605));
#30412=CARTESIAN_POINT('Ctrl Pts',(-0.185446111291195,0.0720704641366568,
1.05831833585989));
#30413=CARTESIAN_POINT('Ctrl Pts',(-0.195001820365716,0.0359852200961074,
1.06036568332373));
#30414=CARTESIAN_POINT('Ctrl Pts',(-0.195093054978418,-5.50606481354719E-5,
1.06241303078758));
#30415=CARTESIAN_POINT('Origin',(0.,0.,-0.129405622560369));
#30416=CARTESIAN_POINT('',(-0.155334812646815,-9.04610707407963E-5,1.09559437743963));
#30417=CARTESIAN_POINT('',(-0.155659711405804,-0.000105088068675666,1.10940562256037));
#30418=CARTESIAN_POINT('',(-0.15555,-2.01987159101623E-14,-0.129405622560369));
#30419=CARTESIAN_POINT('',(0.0499806597877791,0.147301514408978,1.14445));
#30420=CARTESIAN_POINT('Ctrl Pts',(-0.155334812646815,-9.04610707408108E-5,
1.09559437743963));
#30421=CARTESIAN_POINT('Ctrl Pts',(-0.155432667860164,-0.0206859868644216,
1.09706469822836));
#30422=CARTESIAN_POINT('Ctrl Pts',(-0.142041322258558,-0.0930327919713715,
1.10223874069994));
#30423=CARTESIAN_POINT('Ctrl Pts',(-0.0324962964057439,-0.180887727526569,
1.11111650485437));
#30424=CARTESIAN_POINT('Ctrl Pts',(0.134445241673909,-0.125560970886474,
1.12222766990291));
#30425=CARTESIAN_POINT('Ctrl Pts',(0.178171768593789,0.0450698535437549,
1.13333883495146));
#30426=CARTESIAN_POINT('Ctrl Pts',(0.0989503531151977,0.130685679928735,
1.14074627831715));
#30427=CARTESIAN_POINT('Ctrl Pts',(0.0499806597877626,0.147301514408983,
1.14445));
#30428=CARTESIAN_POINT('',(0.155548765964692,0.000619602180124784,1.14445));
#30429=CARTESIAN_POINT('Origin',(0.,0.,1.14445));
#30430=CARTESIAN_POINT('Ctrl Pts',(-0.155659711405804,-0.00010508806867568,
1.10940562256037));
#30431=CARTESIAN_POINT('Ctrl Pts',(-0.155726922058417,-0.0079449137192624,
1.1099684397238));
#30432=CARTESIAN_POINT('Ctrl Pts',(-0.151630179095532,-0.0673453815214831,
1.1142374708816));
#30433=CARTESIAN_POINT('Ctrl Pts',(-0.075277483453787,-0.167898453189698,
1.12221271603377));
#30434=CARTESIAN_POINT('Ctrl Pts',(0.100462758039806,-0.153944373403644,
1.13333135801688));
#30435=CARTESIAN_POINT('Ctrl Pts',(0.155754888396286,-0.0511266487217653,
1.14074378600563));
#30436=CARTESIAN_POINT('Ctrl Pts',(0.155548765964692,0.000619602180124784,
1.14445));
#30437=CARTESIAN_POINT('Origin',(0.,0.,-0.129405622560369));
#30438=CARTESIAN_POINT('',(-0.155445081536763,0.000131810726739325,1.02559437743963));
#30439=CARTESIAN_POINT('',(-0.155305653540906,-4.38315446397164E-5,1.03940562256037));
#30440=CARTESIAN_POINT('',(-0.15555,-2.01987159101623E-14,-0.129405622560369));
#30441=CARTESIAN_POINT('Ctrl Pts',(-0.155445081536763,0.000131810726739319,
1.02559437743963));
#30442=CARTESIAN_POINT('Ctrl Pts',(-0.155154181384031,-0.0359601688445403,
1.02817570146461));
#30443=CARTESIAN_POINT('Ctrl Pts',(-0.124670140973274,-0.124280598265434,
1.03446074717243));
#30444=CARTESIAN_POINT('Ctrl Pts',(0.0223056668548975,-0.182477852394609,
1.04444951456311));
#30445=CARTESIAN_POINT('Ctrl Pts',(0.165390974917898,-0.0802670846854376,
1.05556067961165));
#30446=CARTESIAN_POINT('Ctrl Pts',(0.157153269033781,0.0953897085409752,
1.06667184466019));
#30447=CARTESIAN_POINT('Ctrl Pts',(0.00514163720288116,0.183756944970195,
1.07778300970874));
#30448=CARTESIAN_POINT('Ctrl Pts',(-0.130849536725084,0.114582374749785,
1.08742385396855));
#30449=CARTESIAN_POINT('Ctrl Pts',(-0.155186171668149,0.0311939131113674,
1.09336097654551));
#30450=CARTESIAN_POINT('Ctrl Pts',(-0.155334812646815,-9.04610707408108E-5,
1.09559437743963));
#30451=CARTESIAN_POINT('Ctrl Pts',(-0.155305653540906,-4.38315446397077E-5,
1.03940562256037));
#30452=CARTESIAN_POINT('Ctrl Pts',(-0.155364500629154,-0.0232901140548306,
1.0410644890909));
#30453=CARTESIAN_POINT('Ctrl Pts',(-0.139557528484751,-0.0983968830408974,
1.0464295696158));
#30454=CARTESIAN_POINT('Ctrl Pts',(-0.0231259578302998,-0.182421227428175,
1.05550086413507));
#30455=CARTESIAN_POINT('Ctrl Pts',(0.140774638007895,-0.11829694620695,
1.06661950611819));
#30456=CARTESIAN_POINT('Ctrl Pts',(0.175706993010233,0.0541796064983141,
1.07773814810131));
#30457=CARTESIAN_POINT('Ctrl Pts',(0.0497080432048737,0.177049779856472,
1.08885679008442));
#30458=CARTESIAN_POINT('Ctrl Pts',(-0.113185991314487,0.139680492671116,
1.09941261490411));
#30459=CARTESIAN_POINT('Ctrl Pts',(-0.155284332390808,0.0436812153822664,
1.10626222572943));
#30460=CARTESIAN_POINT('Ctrl Pts',(-0.155659711405804,-0.00010508806867568,
1.10940562256037));
#30461=CARTESIAN_POINT('Origin',(0.,0.,-0.129405622560369));
#30462=CARTESIAN_POINT('',(-0.155804728476752,2.95821195149996E-6,0.95559437743963));
#30463=CARTESIAN_POINT('',(-0.155512930646214,0.000141921665610299,0.969405622560371));
#30464=CARTESIAN_POINT('',(-0.15555,-2.01987159101623E-14,-0.129405622560369));
#30465=CARTESIAN_POINT('Ctrl Pts',(-0.155804728476752,2.95821195150548E-6,
0.95559437743963));
#30466=CARTESIAN_POINT('Ctrl Pts',(-0.155790353315504,-0.0513149683984934,
0.959286704700854));
#30467=CARTESIAN_POINT('Ctrl Pts',(-0.100033131917675,-0.154135965233235,
0.966682753644926));
#30468=CARTESIAN_POINT('Ctrl Pts',(0.0750970673805211,-0.167799333720618,
0.977782524271844));
#30469=CARTESIAN_POINT('Ctrl Pts',(0.181699613594968,-0.0279545920640164,
0.988893689320389));
#30470=CARTESIAN_POINT('Ctrl Pts',(0.122062258834496,0.137466418983892,
1.00000485436893));
#30471=CARTESIAN_POINT('Ctrl Pts',(-0.0492515922639386,0.177116921324136,
1.01111601941748));
#30472=CARTESIAN_POINT('Ctrl Pts',(-0.146173837715872,0.0831558022400444,
1.01964586044104));
#30473=CARTESIAN_POINT('Ctrl Pts',(-0.155571569202373,0.015825134364817,
1.02447197978176));
#30474=CARTESIAN_POINT('Ctrl Pts',(-0.155445081536763,0.000131810726739319,
1.02559437743963));
#30475=CARTESIAN_POINT('Ctrl Pts',(-0.155512930646214,0.000141921665610296,
0.969405622560371));
#30476=CARTESIAN_POINT('Ctrl Pts',(-0.155167703869094,-0.0383344278698275,
0.972160538458));
#30477=CARTESIAN_POINT('Ctrl Pts',(-0.121314953523015,-0.129115961930375,
0.97862166835));
#30478=CARTESIAN_POINT('Ctrl Pts',(0.0309373610575528,-0.181257875466721,
0.988789012236375));
#30479=CARTESIAN_POINT('Ctrl Pts',(0.169095195914933,-0.0722381792257861,
0.999907654219489));
#30480=CARTESIAN_POINT('Ctrl Pts',(0.152354231364944,0.102954552944809,
1.01102629620261));
#30481=CARTESIAN_POINT('Ctrl Pts',(-0.00394931635484403,0.183836962465064,
1.02214493818572));
#30482=CARTESIAN_POINT('Ctrl Pts',(-0.133855689695156,0.109373648628768,
1.03160471363831));
#30483=CARTESIAN_POINT('Ctrl Pts',(-0.15523302537302,0.0286463714736223,
1.03735827509653));
#30484=CARTESIAN_POINT('Ctrl Pts',(-0.155305653540906,-4.38315446397077E-5,
1.03940562256037));
#30485=CARTESIAN_POINT('Origin',(0.,0.,-0.129405622560369));
#30486=CARTESIAN_POINT('',(-0.155453687436568,-0.000133745576774406,0.885594377439631));
#30487=CARTESIAN_POINT('',(-0.155794751152569,-3.71416033132788E-5,0.899405622560372));
#30488=CARTESIAN_POINT('',(-0.15555,-2.01987159101623E-14,-0.129405622560369));
#30489=CARTESIAN_POINT('Ctrl Pts',(-0.155453687436568,-0.000133745576774402,
0.885594377439631));
#30490=CARTESIAN_POINT('Ctrl Pts',(-0.155579877499581,-0.0155062375664632,
0.886693986254252));
#30491=CARTESIAN_POINT('Ctrl Pts',(-0.146423861786649,-0.0825096309536398,
0.891497316751722));
#30492=CARTESIAN_POINT('Ctrl Pts',(-0.0503376402892206,-0.17681153483915,
0.900004368932038));
#30493=CARTESIAN_POINT('Ctrl Pts',(0.12121644264892,-0.138212772940753,
0.911115533980582));
#30494=CARTESIAN_POINT('Ctrl Pts',(0.181867711471885,0.026839009932345,
0.922226699029127));
#30495=CARTESIAN_POINT('Ctrl Pts',(0.0761253709552246,0.167335367481701,
0.933337864077668));
#30496=CARTESIAN_POINT('Ctrl Pts',(-0.099265255914171,0.154733978795034,
0.944449029126215));
#30497=CARTESIAN_POINT('Ctrl Pts',(-0.155732851093913,0.0517959404958592,
0.951867866913534));
#30498=CARTESIAN_POINT('Ctrl Pts',(-0.155804772838109,0.000161323939398619,
0.955582983018006));
#30499=CARTESIAN_POINT('Ctrl Pts',(-0.155804728476752,2.95821195150548E-6,
0.95559437743963));
#30500=CARTESIAN_POINT('Ctrl Pts',(-0.155794751152569,-3.71416033132616E-5,
0.899405622560372));
#30501=CARTESIAN_POINT('Ctrl Pts',(-0.155801224941728,-0.0020493184051098,
0.899550373830729));
#30502=CARTESIAN_POINT('Ctrl Pts',(-0.154853952527048,-0.055575068168544,
0.903401339095459));
#30503=CARTESIAN_POINT('Ctrl Pts',(-0.0935609375970031,-0.15829679799695,
0.91095851835456));
#30504=CARTESIAN_POINT('Ctrl Pts',(0.0823234386500799,-0.164421340203127,
0.922077160337675));
#30505=CARTESIAN_POINT('Ctrl Pts',(0.182795976495949,-0.0199287985657338,
0.933195802320793));
#30506=CARTESIAN_POINT('Ctrl Pts',(0.115819463928053,0.142819381470141,
0.944314444303908));
#30507=CARTESIAN_POINT('Ctrl Pts',(-0.0572526917402423,0.174738822826618,
0.955433086287024));
#30508=CARTESIAN_POINT('Ctrl Pts',(-0.147990815776177,0.0783419353749631,
0.963796812372513));
#30509=CARTESIAN_POINT('Ctrl Pts',(-0.15563214066504,0.01342816322173,0.968454324463628));
#30510=CARTESIAN_POINT('Ctrl Pts',(-0.155512930646214,0.000141921665610296,
0.969405622560371));
#30511=CARTESIAN_POINT('Origin',(0.,0.,-0.129405622560369));
#30512=CARTESIAN_POINT('',(-0.155333906144275,7.80263919018194E-5,0.815594377439631));
#30513=CARTESIAN_POINT('',(-0.155403083159801,-0.000119596074553197,0.829405622560371));
#30514=CARTESIAN_POINT('',(-0.15555,-2.01987159101623E-14,-0.129405622560369));
#30515=CARTESIAN_POINT('Ctrl Pts',(-0.155333906144275,7.80263919018167E-5,
0.815594377439631));
#30516=CARTESIAN_POINT('Ctrl Pts',(-0.155193217426013,-0.0308862600127516,
0.817804989490498));
#30517=CARTESIAN_POINT('Ctrl Pts',(-0.13122308335565,-0.113929638534857,
0.823719323224213));
#30518=CARTESIAN_POINT('Ctrl Pts',(0.00400949547363229,-0.183793690702293,
0.833337378640777));
#30519=CARTESIAN_POINT('Ctrl Pts',(0.156567267939011,-0.0963477420579929,
0.844448543689319));
#30520=CARTESIAN_POINT('Ctrl Pts',(0.165879203582308,0.0792482593671729,
0.855559708737864));
#30521=CARTESIAN_POINT('Ctrl Pts',(0.0234256671005791,0.182338791618694,
0.866670873786407));
#30522=CARTESIAN_POINT('Ctrl Pts',(-0.124241507899534,0.124912116508194,
0.87668243002033));
#30523=CARTESIAN_POINT('Ctrl Pts',(-0.155154841917538,0.0362716593952071,
0.882990264571404));
#30524=CARTESIAN_POINT('Ctrl Pts',(-0.155453687436568,-0.000133745576774402,
0.885594377439631));
#30525=CARTESIAN_POINT('Ctrl Pts',(-0.155403083159801,-0.000119596074553188,
0.829405622560371));
#30526=CARTESIAN_POINT('Ctrl Pts',(-0.155527408252746,-0.017480188940304,
0.830646423197829));
#30527=CARTESIAN_POINT('Ctrl Pts',(-0.14483135129372,-0.0865473027753662,
0.83559343782966));
#30528=CARTESIAN_POINT('Ctrl Pts',(-0.0434704832044991,-0.178666848096071,
0.844246666455862));
#30529=CARTESIAN_POINT('Ctrl Pts',(0.126590215885116,-0.133365823077974,
0.855365308438979));
#30530=CARTESIAN_POINT('Ctrl Pts',(0.18068878531032,0.0341040818691465,
0.866483950422094));
#30531=CARTESIAN_POINT('Ctrl Pts',(0.069268588294083,0.170333168137465,
0.877602592405212));
#30532=CARTESIAN_POINT('Ctrl Pts',(-0.103328002592178,0.150787500329959,
0.888576483117969));
#30533=CARTESIAN_POINT('Ctrl Pts',(-0.155635469933735,0.0494704907375218,
0.895844159836357));
#30534=CARTESIAN_POINT('Ctrl Pts',(-0.155794751152569,-3.71416033132616E-5,
0.899405622560372));
#30535=CARTESIAN_POINT('Origin',(0.,0.,-0.129405622560369));
#30536=CARTESIAN_POINT('',(-0.155738164088485,9.0367155389158E-5,0.745594377439631));
#30537=CARTESIAN_POINT('',(-0.155363820104426,0.000100737127591941,0.759405622560371));
#30538=CARTESIAN_POINT('',(-0.15555,-2.01987159101623E-14,-0.129405622560369));
#30539=CARTESIAN_POINT('Ctrl Pts',(-0.155738164088485,9.03671553891608E-5,
0.745594377439631));
#30540=CARTESIAN_POINT('Ctrl Pts',(-0.155418612064456,-0.0461276292775272,
0.748915992726744));
#30541=CARTESIAN_POINT('Ctrl Pts',(-0.109121796390773,-0.144436334125619,
0.755941329696705));
#30542=CARTESIAN_POINT('Ctrl Pts',(0.0580004387659595,-0.174448118065669,
0.766670388349515));
#30543=CARTESIAN_POINT('Ctrl Pts',(0.17800908511122,-0.0459234407622611,
0.777781553398057));
#30544=CARTESIAN_POINT('Ctrl Pts',(0.135154441460109,0.124617309179735,
0.788892718446602));
#30545=CARTESIAN_POINT('Ctrl Pts',(-0.0313551099181417,0.181143738163968,
0.800003883495145));
#30546=CARTESIAN_POINT('Ctrl Pts',(-0.141757073229054,0.0936656796997624,
0.808904436492822));
#30547=CARTESIAN_POINT('Ctrl Pts',(-0.155428931266511,0.0209921774117757,
0.81410126780765));
#30548=CARTESIAN_POINT('Ctrl Pts',(-0.155333906144275,7.80263919018167E-5,
0.815594377439631));
#30549=CARTESIAN_POINT('Ctrl Pts',(-0.155363820104426,0.000100737127591942,
0.759405622560371));
#30550=CARTESIAN_POINT('Ctrl Pts',(-0.155169765832855,-0.0326159426902871,
0.76174247256493));
#30551=CARTESIAN_POINT('Ctrl Pts',(-0.129071878250434,-0.117503987929593,
0.767785536563862));
#30552=CARTESIAN_POINT('Ctrl Pts',(0.0103792628149562,-0.18358593744105,
0.777534814557165));
#30553=CARTESIAN_POINT('Ctrl Pts',(0.159909575810308,-0.0907769413831382,
0.78865345654028));
#30554=CARTESIAN_POINT('Ctrl Pts',(0.162955779866738,0.0851876712390422,
0.799772098523398));
#30555=CARTESIAN_POINT('Ctrl Pts',(0.0167274199086701,0.183116681231986,
0.810890740506512));
#30556=CARTESIAN_POINT('Ctrl Pts',(-0.126795424285233,0.121093838634352,
0.820768581852172));
#30557=CARTESIAN_POINT('Ctrl Pts',(-0.155156054962447,0.0343750973057136,
0.826940209203457));
#30558=CARTESIAN_POINT('Ctrl Pts',(-0.155403083159801,-0.000119596074553188,
0.829405622560371));
#30559=CARTESIAN_POINT('Origin',(0.,0.,-0.129405622560369));
#30560=CARTESIAN_POINT('',(-0.155606466149984,-0.000136591087330588,0.67559437743963));
#30561=CARTESIAN_POINT('',(-0.155769406638298,6.77585252333857E-5,0.689405622560371));
#30562=CARTESIAN_POINT('',(-0.15555,-2.01987159101623E-14,-0.129405622560369));
#30563=CARTESIAN_POINT('Ctrl Pts',(-0.155606466149984,-0.000136591087330577,
0.67559437743963));
#30564=CARTESIAN_POINT('Ctrl Pts',(-0.155699698050756,-0.010301028373747,
0.676323274280142));
#30565=CARTESIAN_POINT('Ctrl Pts',(-0.150160999329305,-0.0720125819190329,
0.680755892803501));
#30566=CARTESIAN_POINT('Ctrl Pts',(-0.0677079673289082,-0.170914680334463,
0.68889223300971));
#30567=CARTESIAN_POINT('Ctrl Pts',(0.106838781720774,-0.149605051766532,
0.700003398058251));
#30568=CARTESIAN_POINT('Ctrl Pts',(0.183637062036826,0.00858057341481814,
0.711114563106797));
#30569=CARTESIAN_POINT('Ctrl Pts',(0.0924229284360449,0.1589156980696,0.722225728155339));
#30570=CARTESIAN_POINT('Ctrl Pts',(-0.0833503847528551,0.163856370505402,
0.733336893203883));
#30571=CARTESIAN_POINT('Ctrl Pts',(-0.153115801604342,0.0622214122864029,
0.741126442965314));
#30572=CARTESIAN_POINT('Ctrl Pts',(-0.155774924177056,0.00540711533618156,
0.745212271043896));
#30573=CARTESIAN_POINT('Ctrl Pts',(-0.155738164088485,9.03671553891608E-5,
0.745594377439631));
#30574=CARTESIAN_POINT('Ctrl Pts',(-0.155769406638298,6.77585252333878E-5,
0.689405622560371));
#30575=CARTESIAN_POINT('Ctrl Pts',(-0.155508734647919,-0.0476733936548398,
0.692838521932031));
#30576=CARTESIAN_POINT('Ctrl Pts',(-0.106472330039144,-0.147419539900055,
0.699977635298063));
#30577=CARTESIAN_POINT('Ctrl Pts',(0.0633314188332071,-0.172628667698419,
0.710822962658467));
#30578=CARTESIAN_POINT('Ctrl Pts',(0.17940008868909,-0.0403377453646542,
0.721941604641583));
#30579=CARTESIAN_POINT('Ctrl Pts',(0.131130494233742,0.128904301731096,
0.733060246624699));
#30580=CARTESIAN_POINT('Ctrl Pts',(-0.0372603218894873,0.180064416072257,
0.744178888607816));
#30581=CARTESIAN_POINT('Ctrl Pts',(-0.143301362666466,0.0901927254173143,
0.752960680586373));
#30582=CARTESIAN_POINT('Ctrl Pts',(-0.155477533406966,0.0192722899107996,
0.758036258570558));
#30583=CARTESIAN_POINT('Ctrl Pts',(-0.155363820104426,0.000100737127591942,
0.759405622560371));
#30584=CARTESIAN_POINT('Origin',(0.,0.,-0.129405622560369));
#30585=CARTESIAN_POINT('',(-0.155295085115974,-2.74912889200857E-6,0.60559437743963));
#30586=CARTESIAN_POINT('',(-0.155567057787938,-0.000141549514015751,0.619405622560371));
#30587=CARTESIAN_POINT('',(-0.15555,-2.01987159101623E-14,-0.129405622560369));
#30588=CARTESIAN_POINT('Ctrl Pts',(-0.155295114066544,-2.74881667468134E-6,
0.60559437743963));
#30589=CARTESIAN_POINT('Ctrl Pts',(-0.155299180574127,-0.0257905198155464,
0.607434277516388));
#30590=CARTESIAN_POINT('Ctrl Pts',(-0.137005956536857,-0.103483686203599,
0.612977899275993));
#30591=CARTESIAN_POINT('Ctrl Pts',(-0.0143272298638598,-0.183278278249422,
0.622225242718446));
#30592=CARTESIAN_POINT('Ctrl Pts',(0.146185859526926,-0.111471481859797,
0.63333640776699));
#30593=CARTESIAN_POINT('Ctrl Pts',(0.172951224644592,0.0623223129190563,
0.644447572815534));
#30594=CARTESIAN_POINT('Ctrl Pts',(0.0414808152398764,0.179096450999678,
0.655558737864077));
#30595=CARTESIAN_POINT('Ctrl Pts',(-0.11682689842466,0.135101180160119,
0.66594100607211));
#30596=CARTESIAN_POINT('Ctrl Pts',(-0.155225961585962,0.0413472223515983,
0.672619552597294));
#30597=CARTESIAN_POINT('Ctrl Pts',(-0.155606466149984,-0.000136591087330577,
0.67559437743963));
#30598=CARTESIAN_POINT('Ctrl Pts',(-0.155567057787938,-0.000141549514015748,
0.619405622560371));
#30599=CARTESIAN_POINT('Ctrl Pts',(-0.155673152840384,-0.011622012238534,
0.62022835730476));
#30600=CARTESIAN_POINT('Ctrl Pts',(-0.149271086742403,-0.0747018195902368,
0.62475730604352));
#30601=CARTESIAN_POINT('Ctrl Pts',(-0.0632665469493242,-0.172652453095426,
0.632992468776653));
#30602=CARTESIAN_POINT('Ctrl Pts',(0.110806726459172,-0.146742614445027,
0.644111110759769));
#30603=CARTESIAN_POINT('Ctrl Pts',(0.183376231205259,0.0135898253011021,
0.655229752742886));
#30604=CARTESIAN_POINT('Ctrl Pts',(0.0879651525947856,0.161473395492061,
0.666348394726001));
#30605=CARTESIAN_POINT('Ctrl Pts',(-0.0880258220622017,0.161440330069759,
0.677467036709119));
#30606=CARTESIAN_POINT('Ctrl Pts',(-0.153940153309356,0.0591912849892102,
0.685152779320574));
#30607=CARTESIAN_POINT('Ctrl Pts',(-0.155790160368306,0.00386873070159844,
0.689132307937659));
#30608=CARTESIAN_POINT('Ctrl Pts',(-0.155769406638298,6.77585252333878E-5,
0.689405622560371));
#30609=CARTESIAN_POINT('Origin',(0.,0.,-0.129405622560369));
#30610=CARTESIAN_POINT('',(-0.155596383579478,0.000138071545366175,0.53559437743963));
#30611=CARTESIAN_POINT('',(-0.15529563387483,1.51106445085702E-5,0.549405622560371));
#30612=CARTESIAN_POINT('',(-0.15555,-2.01987159101623E-14,-0.129405622560369));
#30613=CARTESIAN_POINT('Ctrl Pts',(-0.155596383579478,0.000138071545366179,
0.53559437743963));
#30614=CARTESIAN_POINT('Ctrl Pts',(-0.155217514150148,-0.0410190199764792,
0.538545280752634));
#30615=CARTESIAN_POINT('Ctrl Pts',(-0.117330640529453,-0.134449549172498,
0.545199905748485));
#30616=CARTESIAN_POINT('Ctrl Pts',(0.0403262995152723,-0.179359935217008,
0.555558252427184));
#30617=CARTESIAN_POINT('Ctrl Pts',(0.172546185411942,-0.0634350903950841,
0.566669417475728));
#30618=CARTESIAN_POINT('Ctrl Pts',(0.146900873501267,0.11052750860401,0.577780582524271));
#30619=CARTESIAN_POINT('Ctrl Pts',(-0.013146340126236,0.183366765077345,
0.588891747572816));
#30620=CARTESIAN_POINT('Ctrl Pts',(-0.136655195880861,0.104159698732297,
0.598163012544601));
#30621=CARTESIAN_POINT('Ctrl Pts',(-0.155290994688111,0.0261203028467153,
0.60373055583354));
#30622=CARTESIAN_POINT('Ctrl Pts',(-0.155295114066544,-2.74881667468134E-6,
0.60559437743963));
#30623=CARTESIAN_POINT('Ctrl Pts',(-0.15529563387483,1.51106445085633E-5,
0.549405622560371));
#30624=CARTESIAN_POINT('Ctrl Pts',(-0.155272340811799,-0.0268780222436924,
0.55132440667186));
#30625=CARTESIAN_POINT('Ctrl Pts',(-0.135831396530156,-0.105747938365068,
0.556949404777722));
#30626=CARTESIAN_POINT('Ctrl Pts',(-0.0103102773360761,-0.183589824620028,
0.566280616877956));
#30627=CARTESIAN_POINT('Ctrl Pts',(0.14869956060099,-0.108166382022474,
0.577399258861071));
#30628=CARTESIAN_POINT('Ctrl Pts',(0.171494149863546,0.0663421591850832,
0.588517900844189));
#30629=CARTESIAN_POINT('Ctrl Pts',(0.0371926577693494,0.180078404398782,
0.599636542827304));
#30630=CARTESIAN_POINT('Ctrl Pts',(-0.118720103315053,0.132645343006727,
0.609932450066032));
#30631=CARTESIAN_POINT('Ctrl Pts',(-0.155195221197423,0.040094597399841,
0.616522143310387));
#30632=CARTESIAN_POINT('Ctrl Pts',(-0.155567057787938,-0.000141549514015748,
0.619405622560371));
#30633=CARTESIAN_POINT('Origin',(0.,0.,-0.129405622560369));
#30634=CARTESIAN_POINT('',(-0.155745492001379,-8.56371120316567E-5,0.46559437743963));
#30635=CARTESIAN_POINT('',(-0.155622585425313,0.000134239099646036,0.479405622560371));
#30636=CARTESIAN_POINT('',(-0.15555,-2.01987159101623E-14,-0.129405622560369));
#30637=CARTESIAN_POINT('Ctrl Pts',(-0.155745492001379,-8.56371120316864E-5,
0.465594377439631));
#30638=CARTESIAN_POINT('Ctrl Pts',(-0.15577850741697,-0.00506891626144068,
0.465952562306032));
#30639=CARTESIAN_POINT('Ctrl Pts',(-0.153301192978291,-0.0615473136307116,
0.470014468855281));
#30640=CARTESIAN_POINT('Ctrl Pts',(-0.0844041411881997,-0.163316067010957,
0.477780097087378));
#30641=CARTESIAN_POINT('Ctrl Pts',(0.0913973507436636,-0.159507746114991,
0.488891262135923));
#30642=CARTESIAN_POINT('Ctrl Pts',(0.183577980123458,-0.00976329900371924,
0.500002427184466));
#30643=CARTESIAN_POINT('Ctrl Pts',(0.10780025055099,0.148913742733129,0.51111359223301));
#30644=CARTESIAN_POINT('Ctrl Pts',(-0.0666056105926533,0.17134727727987,
0.522224757281553));
#30645=CARTESIAN_POINT('Ctrl Pts',(-0.149938299705611,0.0726891414718789,
0.530385019017093));
#30646=CARTESIAN_POINT('Ctrl Pts',(-0.155693038683329,0.0106378444150779,
0.534841559069786));
#30647=CARTESIAN_POINT('Ctrl Pts',(-0.155596383579478,0.000138071545366179,
0.53559437743963));
#30648=CARTESIAN_POINT('Ctrl Pts',(-0.155622585425313,0.000134239099646029,
0.479405622560371));
#30649=CARTESIAN_POINT('Ctrl Pts',(-0.155239700220769,-0.0418962472451577,
0.482420456038961));
#30650=CARTESIAN_POINT('Ctrl Pts',(-0.115964303797854,-0.136226320639006,
0.489141503511923));
#30651=CARTESIAN_POINT('Ctrl Pts',(0.0435376164803608,-0.17865050090601,
0.499568764979258));
#30652=CARTESIAN_POINT('Ctrl Pts',(0.173732980498774,-0.0602360109052031,
0.510687406962374));
#30653=CARTESIAN_POINT('Ctrl Pts',(0.144781397169404,0.113357278356683,
0.521806048945491));
#30654=CARTESIAN_POINT('Ctrl Pts',(-0.0167962271460079,0.183110382765203,
0.532924690928607));
#30655=CARTESIAN_POINT('Ctrl Pts',(-0.137758975876034,0.102035875886683,
0.542124548800234));
#30656=CARTESIAN_POINT('Ctrl Pts',(-0.155317332364345,0.0250672199885809,
0.547618192677488));
#30657=CARTESIAN_POINT('Ctrl Pts',(-0.15529563387483,1.51106445085633E-5,
0.549405622560371));
#30658=CARTESIAN_POINT('Origin',(0.,0.,-0.129405622560369));
#30659=CARTESIAN_POINT('',(-0.155339129538237,-8.2587420025254E-5,0.39559437743963));
#30660=CARTESIAN_POINT('',(-0.15573160577951,-9.4952305265919E-5,0.409405622560371));
#30661=CARTESIAN_POINT('',(-0.15555,-2.01987159101623E-14,-0.129405622560369));
#30662=CARTESIAN_POINT('Ctrl Pts',(-0.155339129538237,-8.25874200252562E-5,
0.39559437743963));
#30663=CARTESIAN_POINT('Ctrl Pts',(-0.155438295724494,-0.0206599346759669,
0.397063565542278));
#30664=CARTESIAN_POINT('Ctrl Pts',(-0.142062281789543,-0.0929876204718288,
0.402236475327773));
#30665=CARTESIAN_POINT('Ctrl Pts',(-0.0325213021862407,-0.180938005122649,
0.411113106796117));
#30666=CARTESIAN_POINT('Ctrl Pts',(0.134348911316817,-0.125485325124609,
0.42222427184466));
#30667=CARTESIAN_POINT('Ctrl Pts',(0.178301209192838,0.0447758371671112,
0.433335436893204));
#30668=CARTESIAN_POINT('Ctrl Pts',(0.0591229481908682,0.174070887258225,
0.444446601941748));
#30669=CARTESIAN_POINT('Ctrl Pts',(-0.10856218085317,0.145071736103991,
0.455199582123889));
#30670=CARTESIAN_POINT('Ctrl Pts',(-0.155437119708937,0.0464594445617744,
0.462248840623184));
#30671=CARTESIAN_POINT('Ctrl Pts',(-0.155745492001379,-8.56371120316864E-5,
0.465594377439631));
#30672=CARTESIAN_POINT('Ctrl Pts',(-0.15573160577951,-9.49523052659442E-5,
0.40940562256037));
#30673=CARTESIAN_POINT('Ctrl Pts',(-0.155772052747877,-0.00572626470532979,
0.40981029141169));
#30674=CARTESIAN_POINT('Ctrl Pts',(-0.152938259291224,-0.0628915705084586,
0.413921174257381));
#30675=CARTESIAN_POINT('Ctrl Pts',(-0.0822616502622442,-0.164452261823584,
0.421738271097444));
#30676=CARTESIAN_POINT('Ctrl Pts',(0.0936204134582059,-0.158261630557358,
0.43285691308056));
#30677=CARTESIAN_POINT('Ctrl Pts',(0.183742116834086,-0.00709647969689106,
0.443975555063676));
#30678=CARTESIAN_POINT('Ctrl Pts',(0.10554806974386,0.150569354438759,0.455094197046793));
#30679=CARTESIAN_POINT('Ctrl Pts',(-0.0693325883166112,0.170307127625589,
0.466212839029909));
#30680=CARTESIAN_POINT('Ctrl Pts',(-0.150503746143118,0.0709862178387775,
0.474316647534435));
#30681=CARTESIAN_POINT('Ctrl Pts',(-0.155710391061042,0.00977293375193425,
0.478714242044589));
#30682=CARTESIAN_POINT('Ctrl Pts',(-0.155622585425313,0.000134239099646029,
0.479405622560371));
#30683=CARTESIAN_POINT('Origin',(0.,0.,-0.129405622560369));
#30684=CARTESIAN_POINT('',(-0.155444674488022,0.000131742778884735,0.32559437743963));
#30685=CARTESIAN_POINT('',(-0.15533186684889,-7.70198572060954E-5,0.339405622560371));
#30686=CARTESIAN_POINT('',(-0.15555,-2.01987159101623E-14,-0.129405622560369));
#30687=CARTESIAN_POINT('Ctrl Pts',(-0.155444674488022,0.000131742778884739,
0.32559437743963));
#30688=CARTESIAN_POINT('Ctrl Pts',(-0.155154236665719,-0.0359445316439912,
0.328174568778523));
#30689=CARTESIAN_POINT('Ctrl Pts',(-0.124691611905359,-0.124248704432008,
0.334458481800264));
#30690=CARTESIAN_POINT('Ctrl Pts',(0.0222506403513669,-0.18248590575151,
0.344446116504855));
#30691=CARTESIAN_POINT('Ctrl Pts',(0.165365282072159,-0.0803151310699741,
0.355557281553397));
#30692=CARTESIAN_POINT('Ctrl Pts',(0.157184646516792,0.0953372104320743,
0.366668446601942));
#30693=CARTESIAN_POINT('Ctrl Pts',(0.00519332482321354,0.183764050268212,
0.377779611650485));
#30694=CARTESIAN_POINT('Ctrl Pts',(-0.130823935507303,0.114600960175539,
0.387421588596382));
#30695=CARTESIAN_POINT('Ctrl Pts',(-0.155188304621527,0.0312141358191517,
0.39335984385943));
#30696=CARTESIAN_POINT('Ctrl Pts',(-0.155339129538237,-8.25874200252562E-5,
0.39559437743963));
#30697=CARTESIAN_POINT('Ctrl Pts',(-0.15533186684889,-7.70198572060919E-5,
0.339405622560371));
#30698=CARTESIAN_POINT('Ctrl Pts',(-0.155425971941861,-0.0210984061911746,
0.34090634077879));
#30699=CARTESIAN_POINT('Ctrl Pts',(-0.141654850766895,-0.0939166341982764,
0.346113272991582));
#30700=CARTESIAN_POINT('Ctrl Pts',(-0.0308692884081366,-0.181269447386996,
0.355026419198746));
#30701=CARTESIAN_POINT('Ctrl Pts',(0.135606994996762,-0.124186426112907,
0.366145061181863));
#30702=CARTESIAN_POINT('Ctrl Pts',(0.177861387826841,0.0466567491694538,
0.377263703164979));
#30703=CARTESIAN_POINT('Ctrl Pts',(0.0571870330903418,0.174760318061885,
0.388382345148095));
#30704=CARTESIAN_POINT('Ctrl Pts',(-0.109574509035902,0.143939945308724,
0.399096318279893));
#30705=CARTESIAN_POINT('Ctrl Pts',(-0.155401613758806,0.0458488658137791,
0.406104077417318));
#30706=CARTESIAN_POINT('Ctrl Pts',(-0.15573160577951,-9.49523052659442E-5,
0.40940562256037));
#30707=CARTESIAN_POINT('Origin',(0.,0.,-0.129405622560369));
#30708=CARTESIAN_POINT('',(-0.155804712705668,3.25009013604671E-6,0.25559437743963));
#30709=CARTESIAN_POINT('',(-0.155449947323643,0.000133480041304715,0.269405622560371));
#30710=CARTESIAN_POINT('',(-0.15555,-2.01987159101623E-14,-0.129405622560369));
#30711=CARTESIAN_POINT('Ctrl Pts',(-0.155804712705668,3.25009013604029E-6,
0.25559437743963));
#30712=CARTESIAN_POINT('Ctrl Pts',(-0.155788927539753,-0.0512989453804214,
0.259285572014769));
#30713=CARTESIAN_POINT('Ctrl Pts',(-0.10006227616332,-0.154106832868198,
0.266680488272757));
#30714=CARTESIAN_POINT('Ctrl Pts',(0.0750458968510211,-0.167822257683237,
0.277779126213592));
#30715=CARTESIAN_POINT('Ctrl Pts',(0.181691053470019,-0.0280099604209337,
0.288890291262136));
#30716=CARTESIAN_POINT('Ctrl Pts',(0.122104229764526,0.137429086670804,
0.30000145631068));
#30717=CARTESIAN_POINT('Ctrl Pts',(-0.0491976593161155,0.177132117679823,
0.311112621359223));
#30718=CARTESIAN_POINT('Ctrl Pts',(-0.146161229246342,0.0831876851886141,
0.319643595068874));
#30719=CARTESIAN_POINT('Ctrl Pts',(-0.155571144064704,0.0158409610837222,
0.324470847095676));
#30720=CARTESIAN_POINT('Ctrl Pts',(-0.155444674488022,0.000131742778884739,
0.32559437743963));
#30721=CARTESIAN_POINT('Ctrl Pts',(-0.155449947323643,0.000133480041304701,
0.269405622560371));
#30722=CARTESIAN_POINT('Ctrl Pts',(-0.155153406972295,-0.0361714100102126,
0.272002390145891));
#30723=CARTESIAN_POINT('Ctrl Pts',(-0.12437032104418,-0.124745277135715,
0.278305371725784));
#30724=CARTESIAN_POINT('Ctrl Pts',(0.0231926238140432,-0.182410602009977,
0.288314567300049));
#30725=CARTESIAN_POINT('Ctrl Pts',(0.165866396469461,-0.0793716828903688,
0.299433209283165));
#30726=CARTESIAN_POINT('Ctrl Pts',(0.156599354026699,0.096375141196464,
0.310551851266282));
#30727=CARTESIAN_POINT('Ctrl Pts',(0.00388050940998321,0.183838154825996,
0.321670493249398));
#30728=CARTESIAN_POINT('Ctrl Pts',(-0.131300314367493,0.113822266482633,
0.331288417014094));
#30729=CARTESIAN_POINT('Ctrl Pts',(-0.155193567478298,0.0308165737536199,
0.337200126784418));
#30730=CARTESIAN_POINT('Ctrl Pts',(-0.15533186684889,-7.70198572060919E-5,
0.339405622560371));
#30731=CARTESIAN_POINT('Origin',(0.,0.,-0.129405622560369));
#30732=CARTESIAN_POINT('',(-0.155454118234884,-0.000133834695600709,0.18559437743963));
#30733=CARTESIAN_POINT('',(-0.155805467550008,3.4854191793785E-6,0.19940562256037));
#30734=CARTESIAN_POINT('',(-0.15555,-2.01987159101623E-14,-0.129405622560369));
#30735=CARTESIAN_POINT('Ctrl Pts',(-0.155454118234884,-0.000133834695600729,
0.18559437743963));
#30736=CARTESIAN_POINT('Ctrl Pts',(-0.155580288786201,-0.0154903851691022,
0.186692853568168));
#30737=CARTESIAN_POINT('Ctrl Pts',(-0.146436232298065,-0.0824775316270878,
0.191495051379553));
#30738=CARTESIAN_POINT('Ctrl Pts',(-0.0503915664640746,-0.176796168665343,
0.200000970873786));
#30739=CARTESIAN_POINT('Ctrl Pts',(0.121174280763407,-0.138249741391359,
0.21111213592233));
#30740=CARTESIAN_POINT('Ctrl Pts',(0.181875888824183,0.0267835396201195,
0.222223300970874));
#30741=CARTESIAN_POINT('Ctrl Pts',(0.0761764071097843,0.167312138149853,
0.233334466019417));
#30742=CARTESIAN_POINT('Ctrl Pts',(-0.0992180579104728,0.154764252547341,
0.244445631067961));
#30743=CARTESIAN_POINT('Ctrl Pts',(-0.155725669913861,0.0518277207581445,
0.251865601541365));
#30744=CARTESIAN_POINT('Ctrl Pts',(-0.155804766277071,0.00017735852989955,
0.255581850331921));
#30745=CARTESIAN_POINT('Ctrl Pts',(-0.155804712705668,3.25009013604029E-6,
0.25559437743963));
#30746=CARTESIAN_POINT('Ctrl Pts',(-0.155805467550008,3.48541917938314E-6,
0.19940562256037));
#30747=CARTESIAN_POINT('Ctrl Pts',(-0.155788564535512,-0.0513206116891616,
0.203098439512992));
#30748=CARTESIAN_POINT('Ctrl Pts',(-0.100003893378143,-0.154186484140614,
0.210497470459985));
#30749=CARTESIAN_POINT('Ctrl Pts',(0.0752488571272716,-0.167777039880966,
0.221602715401351));
#30750=CARTESIAN_POINT('Ctrl Pts',(0.181781810074028,-0.0276929424335053,
0.232721357384467));
#30751=CARTESIAN_POINT('Ctrl Pts',(0.121794738393109,0.137759091140133,
0.243839999367584));
#30752=CARTESIAN_POINT('Ctrl Pts',(-0.0497615974795104,0.177017821004958,
0.2549586413507));
#30753=CARTESIAN_POINT('Ctrl Pts',(-0.146313162187878,0.0828233020270418,
0.263480515748296));
#30754=CARTESIAN_POINT('Ctrl Pts',(-0.155576641614544,0.0156444291597347,
0.268296176151519));
#30755=CARTESIAN_POINT('Ctrl Pts',(-0.155449947323643,0.000133480041304701,
0.269405622560371));
#30756=CARTESIAN_POINT('Origin',(0.,0.,-0.129405622560369));
#30757=CARTESIAN_POINT('',(-0.155333634177863,7.79921548230329E-5,0.11559437743963));
#30758=CARTESIAN_POINT('',(-0.155460191805193,-0.000135568056800359,0.12940562256037));
#30759=CARTESIAN_POINT('',(-0.15555,-2.01987159101623E-14,-0.129405622560369));
#30760=CARTESIAN_POINT('Ctrl Pts',(-0.155333634177863,7.79921548230561E-5,
0.11559437743963));
#30761=CARTESIAN_POINT('Ctrl Pts',(-0.155193438638927,-0.0308706275100063,
0.117803856804414));
#30762=CARTESIAN_POINT('Ctrl Pts',(-0.131241956589738,-0.11389814578602,
0.123717057852045));
#30763=CARTESIAN_POINT('Ctrl Pts',(0.00395347168138628,-0.183794704008407,
0.133333980582524));
#30764=CARTESIAN_POINT('Ctrl Pts',(0.156537855283131,-0.0963955976349113,
0.144445145631068));
#30765=CARTESIAN_POINT('Ctrl Pts',(0.165903376979378,0.0791977165381959,
0.155556310679611));
#30766=CARTESIAN_POINT('Ctrl Pts',(0.0234812759114929,0.182331608910266,
0.166667475728155));
#30767=CARTESIAN_POINT('Ctrl Pts',(-0.124220109658982,0.124943524423025,
0.176680164648161));
#30768=CARTESIAN_POINT('Ctrl Pts',(-0.155154880719052,0.0362871523529771,
0.18298913188532));
#30769=CARTESIAN_POINT('Ctrl Pts',(-0.155454118234884,-0.000133834695600729,
0.18559437743963));
#30770=CARTESIAN_POINT('Ctrl Pts',(-0.155460191805193,-0.000135568056800364,
0.12940562256037));
#30771=CARTESIAN_POINT('Ctrl Pts',(-0.15558637635503,-0.0152693971168416,
0.130488274885721));
#30772=CARTESIAN_POINT('Ctrl Pts',(-0.146605510259419,-0.0820638709603335,
0.135277141205443));
#30773=CARTESIAN_POINT('Ctrl Pts',(-0.0510374815939226,-0.176654153931159,
0.143772221519537));
#30774=CARTESIAN_POINT('Ctrl Pts',(0.120797626960931,-0.138634273102519,
0.154890863502654));
#30775=CARTESIAN_POINT('Ctrl Pts',(0.181976886629041,0.0263806680570579,
0.16600950548577));
#30776=CARTESIAN_POINT('Ctrl Pts',(0.0764574137846417,0.167229745635935,
0.177128147468886));
#30777=CARTESIAN_POINT('Ctrl Pts',(-0.0991003621173195,0.154889135395602,
0.188246789452002));
#30778=CARTESIAN_POINT('Ctrl Pts',(-0.15572087700955,0.0518861158146895,
0.195672614482497));
#30779=CARTESIAN_POINT('Ctrl Pts',(-0.155805528871865,0.000189682319971778,
0.19939222551862));
#30780=CARTESIAN_POINT('Ctrl Pts',(-0.155805467550008,3.48541917938314E-6,
0.19940562256037));
#30781=CARTESIAN_POINT('Origin',(0.,0.,-0.129405622560369));
#30782=CARTESIAN_POINT('',(-0.155735926886437,0.000101346774827271,0.0455943774396301));
#30783=CARTESIAN_POINT('',(-0.155326046963413,7.29270061605516E-5,0.0594056225603705));
#30784=CARTESIAN_POINT('',(-0.15555,-2.01987159101623E-14,-0.129405622560369));
#30785=CARTESIAN_POINT('Ctrl Pts',(-0.155735926886437,0.000101346774827265,
0.0455943774396301));
#30786=CARTESIAN_POINT('Ctrl Pts',(-0.15541538777776,-0.0460983628495037,
0.0489148600406595));
#30787=CARTESIAN_POINT('Ctrl Pts',(-0.109151218308356,-0.144423481489054,
0.0559390643245367));
#30788=CARTESIAN_POINT('Ctrl Pts',(0.0579488995883613,-0.174456230311225,
0.0666669902912619));
#30789=CARTESIAN_POINT('Ctrl Pts',(0.177994191588978,-0.0459827600750814,
0.0777781553398056));
#30790=CARTESIAN_POINT('Ctrl Pts',(0.135192905881154,0.124578720765632,
0.0888893203883492));
#30791=CARTESIAN_POINT('Ctrl Pts',(-0.0313001003158473,0.181151906168851,
0.100000485436893));
#30792=CARTESIAN_POINT('Ctrl Pts',(-0.141742497137191,0.093698092273704,
0.108902171120653));
#30793=CARTESIAN_POINT('Ctrl Pts',(-0.155428446607623,0.0210081433596544,
0.114100135121566));
#30794=CARTESIAN_POINT('Ctrl Pts',(-0.155333634177863,7.79921548230561E-5,
0.11559437743963));
#30795=CARTESIAN_POINT('Ctrl Pts',(-0.155326046963413,7.29270061605551E-5,
0.0594056225603705));
#30796=CARTESIAN_POINT('Ctrl Pts',(-0.155199262831984,-0.0304485333833814,
0.0615843242528215));
#30797=CARTESIAN_POINT('Ctrl Pts',(-0.131743653601245,-0.113071739766558,
0.0674692399396446));
#30798=CARTESIAN_POINT('Ctrl Pts',(0.00255447675030308,-0.183860034663711,
0.0770603696208398));
#30799=CARTESIAN_POINT('Ctrl Pts',(0.155899683301632,-0.0975032021788082,
0.0881790116039561));
#30800=CARTESIAN_POINT('Ctrl Pts',(0.166434877052597,0.0781732535368643,
0.0992976535870723));
#30801=CARTESIAN_POINT('Ctrl Pts',(0.0245080507541896,0.182238325373942,
0.110416295570189));
#30802=CARTESIAN_POINT('Ctrl Pts',(-0.123863138927055,0.125487925833816,
0.120452285227955));
#30803=CARTESIAN_POINT('Ctrl Pts',(-0.155154412248428,0.0365378245899198,
0.126782060891349));
#30804=CARTESIAN_POINT('Ctrl Pts',(-0.155460191805193,-0.000135568056800364,
0.12940562256037));
#30805=CARTESIAN_POINT('Origin',(0.,0.,1.15));
#30806=CARTESIAN_POINT('',(-0.177892626630995,-0.00012009523392913,1.12223275485995));
#30807=CARTESIAN_POINT('Ctrl Pts',(0.155548765964692,0.000619602180104872,
1.14445));
#30808=CARTESIAN_POINT('Ctrl Pts',(0.156083861551471,-0.0102125174737046,
1.14395805623115));
#30809=CARTESIAN_POINT('Ctrl Pts',(0.15539846640382,-0.0210404421466269,
1.14347026853365));
#30810=CARTESIAN_POINT('Ctrl Pts',(0.153608590638952,-0.0317127652002419,
1.14298392615444));
#30811=CARTESIAN_POINT('Ctrl Pts',(0.152914716720618,-0.0358500616318106,
1.14279538776594));
#30812=CARTESIAN_POINT('Ctrl Pts',(0.152054287987853,-0.0399640361908485,
1.14260706658696));
#30813=CARTESIAN_POINT('Ctrl Pts',(0.151032028551573,-0.0440458121014301,
1.1424188046881));
#30814=CARTESIAN_POINT('Ctrl Pts',(0.150071136707034,-0.0478825535826186,
1.14224184440107));
#30815=CARTESIAN_POINT('Ctrl Pts',(0.148969254907822,-0.0516824965112672,
1.14206531990211));
#30816=CARTESIAN_POINT('Ctrl Pts',(0.147732675525468,-0.0554351396328931,
1.14188926057926));
#30817=CARTESIAN_POINT('Ctrl Pts',(0.144705099540774,-0.0646229138722882,
1.14145820618411));
#30818=CARTESIAN_POINT('Ctrl Pts',(0.14087037084284,-0.0735342808861364,
1.14102963880076));
#30819=CARTESIAN_POINT('Ctrl Pts',(0.136287966367236,-0.0820616333277537,
1.14060170770949));
#30820=CARTESIAN_POINT('Ctrl Pts',(0.134099734044687,-0.0861336938230361,
1.1403973580824));
#30821=CARTESIAN_POINT('Ctrl Pts',(0.131738457084688,-0.090120565054425,
1.14019301071694));
#30822=CARTESIAN_POINT('Ctrl Pts',(0.129223539536337,-0.0939888668888786,
1.1399895855729));
#30823=CARTESIAN_POINT('Ctrl Pts',(0.123841150615535,-0.102267748615928,
1.1395542181223));
#30824=CARTESIAN_POINT('Ctrl Pts',(0.117747056171278,-0.110025200831312,
1.1391220629978));
#30825=CARTESIAN_POINT('Ctrl Pts',(0.11100116606729,-0.117148456023219,
1.13869123413476));
#30826=CARTESIAN_POINT('Ctrl Pts',(0.106906026602935,-0.121472677586479,
1.13842969647966));
#30827=CARTESIAN_POINT('Ctrl Pts',(0.102570142764087,-0.125562999006382,
1.13816864757596));
#30828=CARTESIAN_POINT('Ctrl Pts',(0.0980025572591369,-0.129390839920029,
1.13790766548932));
#30829=CARTESIAN_POINT('Ctrl Pts',(0.0956731876101781,-0.131342955854285,
1.13777457027942));
#30830=CARTESIAN_POINT('Ctrl Pts',(0.0932817165779503,-0.133228060285772,
1.13764139558094));
#30831=CARTESIAN_POINT('Ctrl Pts',(0.0908350990518728,-0.135037587415829,
1.1375084117344));
#30832=CARTESIAN_POINT('Ctrl Pts',(0.0901763381324703,-0.135524809363345,
1.13747260533636));
#30833=CARTESIAN_POINT('Ctrl Pts',(0.0895137718121014,-0.136006421121091,
1.1374368229172));
#30834=CARTESIAN_POINT('Ctrl Pts',(0.0888474357058895,-0.136482361432558,
1.13740106343829));
#30835=CARTESIAN_POINT('Ctrl Pts',(0.0798411198483208,-0.142915254284167,
1.1369177320399));
#30836=CARTESIAN_POINT('Ctrl Pts',(0.0701492813036541,-0.148315340119806,
1.1364385915245));
#30837=CARTESIAN_POINT('Ctrl Pts',(0.059971176200061,-0.152699426079087,
1.13596107719954));
#30838=CARTESIAN_POINT('Ctrl Pts',(0.0530631196487977,-0.155674981295315,
1.13563697994103));
#30839=CARTESIAN_POINT('Ctrl Pts',(0.0459300802687867,-0.158181722966519,
1.13531363179894));
#30840=CARTESIAN_POINT('Ctrl Pts',(0.0386275637501033,-0.16021396300419,
1.13499023090658));
#30841=CARTESIAN_POINT('Ctrl Pts',(0.0351988940876516,-0.161168138149998,
1.13483838806916));
#30842=CARTESIAN_POINT('Ctrl Pts',(0.0317324236549294,-0.162017357570902,
1.13468652012024));
#30843=CARTESIAN_POINT('Ctrl Pts',(0.028249074324747,-0.162757963065587,
1.13453519958799));
#30844=CARTESIAN_POINT('Ctrl Pts',(0.0167982212800381,-0.165192563755867,
1.13403776191718));
#30845=CARTESIAN_POINT('Ctrl Pts',(0.00512774808450533,-0.166468890755321,
1.13354451715097));
#30846=CARTESIAN_POINT('Ctrl Pts',(-0.00655533748915361,-0.166579173106486,
1.13305265956701));
#30847=CARTESIAN_POINT('Ctrl Pts',(-0.0141044995850598,-0.166650433334789,
1.1327348400487));
#30848=CARTESIAN_POINT('Ctrl Pts',(-0.0216594951399176,-0.166233867742642,
1.13241759971353));
#30849=CARTESIAN_POINT('Ctrl Pts',(-0.0291655735035569,-0.165315833865676,
1.13210018160962));
#30850=CARTESIAN_POINT('Ctrl Pts',(-0.0327092118793667,-0.164882427775424,
1.13195032772857));
#30851=CARTESIAN_POINT('Ctrl Pts',(-0.0362323925945039,-0.164338226995567,
1.13180083633464));
#30852=CARTESIAN_POINT('Ctrl Pts',(-0.0397271405986897,-0.163683459359474,
1.13165172827032));
#30853=CARTESIAN_POINT('Ctrl Pts',(-0.0499359232133337,-0.16177076624055,
1.13121615700369));
#30854=CARTESIAN_POINT('Ctrl Pts',(-0.0599087164806791,-0.158916175424461,
1.13078358684414));
#30855=CARTESIAN_POINT('Ctrl Pts',(-0.0695044280650932,-0.155097228857054,
1.13035212687658));
#30856=CARTESIAN_POINT('Ctrl Pts',(-0.0757996376989387,-0.152591831627178,
1.1300690701256));
#30857=CARTESIAN_POINT('Ctrl Pts',(-0.0819325841193579,-0.149670688079838,
1.12978649119439));
#30858=CARTESIAN_POINT('Ctrl Pts',(-0.0878818038415969,-0.146365274834167,
1.12950385616925));
#30859=CARTESIAN_POINT('Ctrl Pts',(-0.0910874459297812,-0.144584205666465,
1.12935156279727));
#30860=CARTESIAN_POINT('Ctrl Pts',(-0.09424019426452,-0.142690781721644,
1.129199221353));
#30861=CARTESIAN_POINT('Ctrl Pts',(-0.0973230172632952,-0.140698989172901,
1.12904742410559));
#30862=CARTESIAN_POINT('Ctrl Pts',(-0.107217543799977,-0.134306197813512,
1.12856022069066));
#30863=CARTESIAN_POINT('Ctrl Pts',(-0.116428399613608,-0.126885604548101,
1.12807698662012));
#30864=CARTESIAN_POINT('Ctrl Pts',(-0.124852487683086,-0.118613771136687,
1.12759508954235));
#30865=CARTESIAN_POINT('Ctrl Pts',(-0.129034307879819,-0.114507532011624,
1.12735586994778));
#30866=CARTESIAN_POINT('Ctrl Pts',(-0.133021908645802,-0.110190752518543,
1.12711697982177));
#30867=CARTESIAN_POINT('Ctrl Pts',(-0.136799920681752,-0.105681293454548,
1.12687809715289));
#30868=CARTESIAN_POINT('Ctrl Pts',(-0.139913092404994,-0.101965391993263,
1.12668125215535));
#30869=CARTESIAN_POINT('Ctrl Pts',(-0.142886395744951,-0.0981144149624532,
1.12648421657965));
#30870=CARTESIAN_POINT('Ctrl Pts',(-0.145693560119959,-0.0941626751454851,
1.12628802354802));
#30871=CARTESIAN_POINT('Ctrl Pts',(-0.152880478586678,-0.0840454080131806,
1.12578572901386));
#30872=CARTESIAN_POINT('Ctrl Pts',(-0.15900482121196,-0.0732463252276768,
1.12528759909576));
#30873=CARTESIAN_POINT('Ctrl Pts',(-0.163934147646496,-0.0619414999212126,
1.12479074962784));
#30874=CARTESIAN_POINT('Ctrl Pts',(-0.166135734382546,-0.0568924219632783,
1.1245688415816));
#30875=CARTESIAN_POINT('Ctrl Pts',(-0.168098373685913,-0.0517419572379162,
1.12434718895784));
#30876=CARTESIAN_POINT('Ctrl Pts',(-0.169806974463718,-0.0465039785200352,
1.12412553479695));
#30877=CARTESIAN_POINT('Ctrl Pts',(-0.171302024805205,-0.0419206715400791,
1.12393158420695));
#30878=CARTESIAN_POINT('Ctrl Pts',(-0.172603159720904,-0.037265702966286,
1.12373744627196));
#30879=CARTESIAN_POINT('Ctrl Pts',(-0.173693332107248,-0.0325769359939504,
1.12354412603317));
#30880=CARTESIAN_POINT('Ctrl Pts',(-0.174146803491923,-0.0306265823819912,
1.12346371196521));
#30881=CARTESIAN_POINT('Ctrl Pts',(-0.174564098410947,-0.0286695573112724,
1.12338340400172));
#30882=CARTESIAN_POINT('Ctrl Pts',(-0.174944665354966,-0.0267065873422436,
1.12330319031487));
#30883=CARTESIAN_POINT('Ctrl Pts',(-0.176644787249262,-0.0179373332737037,
1.1229448485109));
#30884=CARTESIAN_POINT('Ctrl Pts',(-0.177613299278372,-0.00904985393428815,
1.12258838819752));
#30885=CARTESIAN_POINT('Ctrl Pts',(-0.177892626630995,-0.00012009523392913,
1.12223275485995));
#30886=CARTESIAN_POINT('',(0.188128289424299,-0.051655738433239,1.1046));
#30887=CARTESIAN_POINT('Ctrl Pts',(0.188079991776263,-0.0516378774142054,
1.1046));
#30888=CARTESIAN_POINT('Ctrl Pts',(0.189767230432996,-0.0390669740826218,
1.10628778184834));
#30889=CARTESIAN_POINT('Ctrl Pts',(0.190280594088308,-0.0264116239428061,
1.10798825493552));
#30890=CARTESIAN_POINT('Ctrl Pts',(0.189578785198131,-0.013858618669063,
1.10971174069725));
#30891=CARTESIAN_POINT('Ctrl Pts',(0.189002564675101,-0.00355196771938053,
1.11112680950153));
#30892=CARTESIAN_POINT('Ctrl Pts',(0.187606197243972,0.00668612269204304,
1.11255739169934));
#30893=CARTESIAN_POINT('Ctrl Pts',(0.185342457317502,0.0167394104911895,
1.1140092000994));
#30894=CARTESIAN_POINT('Ctrl Pts',(0.184551132811226,0.0202536891903846,
1.1145167016688));
#30895=CARTESIAN_POINT('Ctrl Pts',(0.183655673454389,0.0237360512197014,
1.1150254747949));
#30896=CARTESIAN_POINT('Ctrl Pts',(0.18265534113529,0.0271808706561584,
1.11553563926267));
#30897=CARTESIAN_POINT('Ctrl Pts',(0.18094879298457,0.0330576679230306,
1.11640597026411));
#30898=CARTESIAN_POINT('Ctrl Pts',(0.178936945382248,0.038826456249319,
1.11728051290445));
#30899=CARTESIAN_POINT('Ctrl Pts',(0.176612263817241,0.0444636415640588,
1.1181607012295));
#30900=CARTESIAN_POINT('Ctrl Pts',(0.172529449099474,0.0543641731105064,
1.11970656708142));
#30901=CARTESIAN_POINT('Ctrl Pts',(0.167482382247398,0.0638604192469179,
1.12126984735358));
#30902=CARTESIAN_POINT('Ctrl Pts',(0.161567727140847,0.0728508334626257,
1.12285831080443));
#30903=CARTESIAN_POINT('Ctrl Pts',(0.159791310571961,0.0755510282307451,
1.12333539234888));
#30904=CARTESIAN_POINT('Ctrl Pts',(0.157935831204718,0.07820633305328,1.12381491808146));
#30905=CARTESIAN_POINT('Ctrl Pts',(0.156005857937656,0.080810555607592,
1.12429655968642));
#30906=CARTESIAN_POINT('Ctrl Pts',(0.149084780910453,0.0901495579668382,
1.12602377461955));
#30907=CARTESIAN_POINT('Ctrl Pts',(0.141258220296783,0.0987686403112959,
1.12776582990404));
#30908=CARTESIAN_POINT('Ctrl Pts',(0.132662596065602,0.106547632773669,
1.12953438681126));
#30909=CARTESIAN_POINT('Ctrl Pts',(0.125865807878512,0.11269868854969,1.13093283169111));
#30910=CARTESIAN_POINT('Ctrl Pts',(0.11858709408701,0.11832389399092,1.13234784666969));
#30911=CARTESIAN_POINT('Ctrl Pts',(0.110887722236713,0.123341541992538,
1.13378519708595));
#30912=CARTESIAN_POINT('Ctrl Pts',(0.108018415924993,0.125211456754541,
1.13432085099405));
#30913=CARTESIAN_POINT('Ctrl Pts',(0.105090557092059,0.126996521585399,
1.13485961189033));
#30914=CARTESIAN_POINT('Ctrl Pts',(0.102119703918859,0.128685646974318,
1.13539959124502));
#30915=CARTESIAN_POINT('Ctrl Pts',(0.0927768272952827,0.133997686711853,
1.13709774332326));
#30916=CARTESIAN_POINT('Ctrl Pts',(0.082979544177925,0.138384526176108,
1.13881348137989));
#30917=CARTESIAN_POINT('Ctrl Pts',(0.0728343136972591,0.141721417442936,
1.14055808556308));
#30918=CARTESIAN_POINT('Ctrl Pts',(0.0653892612002304,0.144170186912073,
1.14183835906254));
#30919=CARTESIAN_POINT('Ctrl Pts',(0.0577564921504827,0.146052612758731,
1.14313417790127));
#30920=CARTESIAN_POINT('Ctrl Pts',(0.0499806597877626,0.147301514408983,
1.14445));
#30921=CARTESIAN_POINT('',(0.156060797133591,0.117265290216009,1.1046));
#30922=CARTESIAN_POINT('Origin',(0.,0.,1.1046));
#30923=CARTESIAN_POINT('Ctrl Pts',(-0.177892626630995,-0.00012009523392913,
1.12223275485995));
#30924=CARTESIAN_POINT('Ctrl Pts',(-0.178130827469488,0.00749489839273535,
1.12192948288029));
#30925=CARTESIAN_POINT('Ctrl Pts',(-0.177867516731744,0.0151409018269471,
1.12162681218094));
#30926=CARTESIAN_POINT('Ctrl Pts',(-0.177119648653777,0.022772046405986,
1.12132408898598));
#30927=CARTESIAN_POINT('Ctrl Pts',(-0.176683933562239,0.0272180241883703,
1.12114771955869));
#30928=CARTESIAN_POINT('Ctrl Pts',(-0.176082727329522,0.0316616978614784,
1.1209712215835));
#30929=CARTESIAN_POINT('Ctrl Pts',(-0.175323410854016,0.0360699258071878,
1.12079542245302));
#30930=CARTESIAN_POINT('Ctrl Pts',(-0.173218074679692,0.0482924997380182,
1.12030798897732));
#30931=CARTESIAN_POINT('Ctrl Pts',(-0.169899117173377,0.060280772698104,
1.11982442300823));
#30932=CARTESIAN_POINT('Ctrl Pts',(-0.165450405286176,0.0718434015054524,
1.11934209182814));
#30933=CARTESIAN_POINT('Ctrl Pts',(-0.163468469691568,0.0769946421750163,
1.11912720955245));
#30934=CARTESIAN_POINT('Ctrl Pts',(-0.161261595477516,0.0820613755489734,
1.11891257235417));
#30935=CARTESIAN_POINT('Ctrl Pts',(-0.158833971908418,0.0870258740589896,
1.11869794744021));
#30936=CARTESIAN_POINT('Ctrl Pts',(-0.157259648823123,0.0902453701582717,
1.11855876237008));
#30937=CARTESIAN_POINT('Ctrl Pts',(-0.155591255289476,0.0934239508703652,
1.11841948892714));
#30938=CARTESIAN_POINT('Ctrl Pts',(-0.153833447558489,0.0965496328988143,
1.11828037128997));
#30939=CARTESIAN_POINT('Ctrl Pts',(-0.14771977559034,0.10742078465325,1.11779651882779));
#30940=CARTESIAN_POINT('Ctrl Pts',(-0.140558745189236,0.117602653899592,
1.11731683957354));
#30941=CARTESIAN_POINT('Ctrl Pts',(-0.132418289468816,0.126903043139938,
1.11683877992991));
#30942=CARTESIAN_POINT('Ctrl Pts',(-0.12909688936255,0.130697709540948,
1.11664372606491));
#30943=CARTESIAN_POINT('Ctrl Pts',(-0.125611892721837,0.134345412680643,
1.11644894182206));
#30944=CARTESIAN_POINT('Ctrl Pts',(-0.121965775424868,0.137831740927343,
1.11625425375315));
#30945=CARTESIAN_POINT('Ctrl Pts',(-0.117995359394073,0.141628155697328,
1.11604224942997));
#30946=CARTESIAN_POINT('Ctrl Pts',(-0.113833879872902,0.145233242900832,
1.11583035914965));
#30947=CARTESIAN_POINT('Ctrl Pts',(-0.109497995542763,0.148643456469952,
1.11561835894421));
#30948=CARTESIAN_POINT('Ctrl Pts',(-0.106528819965926,0.150978740824945,
1.11547318306212));
#30949=CARTESIAN_POINT('Ctrl Pts',(-0.103484861618328,0.153216986140016,
1.11532830099587));
#30950=CARTESIAN_POINT('Ctrl Pts',(-0.100375391374892,0.155356036404444,
1.11518378070706));
#30951=CARTESIAN_POINT('Ctrl Pts',(-0.0901590665073864,0.162383996377836,
1.11470895184398));
#30952=CARTESIAN_POINT('Ctrl Pts',(-0.0792284020877703,0.168351899996775,
1.11423755053895));
#30953=CARTESIAN_POINT('Ctrl Pts',(-0.0677866372531476,0.173236468334987,
1.11376713654095));
#30954=CARTESIAN_POINT('Ctrl Pts',(-0.0629527485252524,0.175300088779209,
1.11356839718953));
#30955=CARTESIAN_POINT('Ctrl Pts',(-0.0580272205709242,0.1771698553942,
1.11336983405985));
#30956=CARTESIAN_POINT('Ctrl Pts',(-0.053024031320765,0.178841703955505,
1.11317126314023));
#30957=CARTESIAN_POINT('Ctrl Pts',(-0.0477983789695303,0.180587890023723,
1.11296386291187));
#30958=CARTESIAN_POINT('Ctrl Pts',(-0.0424815416125505,0.182119285098682,
1.11275621043829));
#30959=CARTESIAN_POINT('Ctrl Pts',(-0.0371242414709178,0.183422331662166,
1.11254943891139));
#30960=CARTESIAN_POINT('Ctrl Pts',(-0.024630778610864,0.18646109436267,
1.11206723848886));
#30961=CARTESIAN_POINT('Ctrl Pts',(-0.0118919597510465,0.188273325293319,
1.11158873863955));
#30962=CARTESIAN_POINT('Ctrl Pts',(0.000886208579909016,0.188815541438236,
1.11111139386139));
#30963=CARTESIAN_POINT('Ctrl Pts',(0.00944159770367764,0.189178572350712,
1.1107917963872));
#30964=CARTESIAN_POINT('Ctrl Pts',(0.018015230692156,0.18897135417352,1.11047271669991));
#30965=CARTESIAN_POINT('Ctrl Pts',(0.0265466554166013,0.188167601942836,
1.11015339081081));
#30966=CARTESIAN_POINT('Ctrl Pts',(0.0302389326862781,0.187819749598396,
1.11001519118297));
#30967=CARTESIAN_POINT('Ctrl Pts',(0.0339178177085591,0.187360375525866,
1.1098771490423));
#30968=CARTESIAN_POINT('Ctrl Pts',(0.0375710017615334,0.186789297951633,
1.1097394835104));
#30969=CARTESIAN_POINT('Ctrl Pts',(0.0423078408099154,0.186048819915471,
1.10956098183688));
#30970=CARTESIAN_POINT('Ctrl Pts',(0.0470053189021468,0.185120233668386,
1.10938296950455));
#30971=CARTESIAN_POINT('Ctrl Pts',(0.0516529562716852,0.184000805096474,
1.10920531719144));
#30972=CARTESIAN_POINT('Ctrl Pts',(0.0618028867738203,0.181556095816553,
1.10881734401536));
#30973=CARTESIAN_POINT('Ctrl Pts',(0.0717155486830652,0.178202889727245,
1.10843108790673));
#30974=CARTESIAN_POINT('Ctrl Pts',(0.0813183120370126,0.174031280266035,
1.10804520187417));
#30975=CARTESIAN_POINT('Ctrl Pts',(0.0859478038432918,0.172020147521446,
1.10785916623421));
#30976=CARTESIAN_POINT('Ctrl Pts',(0.0905051909798001,0.169818426512715,
1.10767321660747));
#30977=CARTESIAN_POINT('Ctrl Pts',(0.0949816305437677,0.167434340091183,
1.10748720206377));
#30978=CARTESIAN_POINT('Ctrl Pts',(0.0983118022353031,0.165660739219842,
1.10734881968224));
#30979=CARTESIAN_POINT('Ctrl Pts',(0.101597049834463,0.16378593049508,1.10721040073536));
#30980=CARTESIAN_POINT('Ctrl Pts',(0.104821419449008,0.161821258958598,
1.10707241581092));
#30981=CARTESIAN_POINT('Ctrl Pts',(0.116000559886905,0.155009589811987,
1.10659401133715));
#30982=CARTESIAN_POINT('Ctrl Pts',(0.126488220095427,0.147101893720343,
1.10611923196118));
#30983=CARTESIAN_POINT('Ctrl Pts',(0.136144216947772,0.138260857674004,
1.10564559537577));
#30984=CARTESIAN_POINT('Ctrl Pts',(0.143255609150872,0.131749663048667,
1.1052967742678));
#30985=CARTESIAN_POINT('Ctrl Pts',(0.149915772834495,0.124730943289562,
1.10494857300279));
#30986=CARTESIAN_POINT('Ctrl Pts',(0.156057659382849,0.117255425406029,
1.1046));
#30987=CARTESIAN_POINT('',(-0.0999999999999999,-1.22464679914735E-17,1.2));
#30988=CARTESIAN_POINT('',(-0.15,-1.83697019872103E-17,1.15));
#30989=CARTESIAN_POINT('Origin',(0.,0.,1.2));
#30990=CARTESIAN_POINT('Ctrl Pts',(0.113509973994371,-0.159049193030953,
-0.0230074082272069));
#30991=CARTESIAN_POINT('Ctrl Pts',(0.166385127640631,-0.121313337847033,
-0.019303686544359));
#30992=CARTESIAN_POINT('Ctrl Pts',(0.230633516687349,0.0103782615975306,
-0.0118962431786632));
#30993=CARTESIAN_POINT('Ctrl Pts',(0.116188988078006,0.199753850566951,
-0.000785078130119459));
#30994=CARTESIAN_POINT('Ctrl Pts',(-0.104655428901899,0.205782953697956,
0.0103260869184242));
#30995=CARTESIAN_POINT('Ctrl Pts',(-0.229698075471667,0.0238333788527267,
0.0214372519669679));
#30996=CARTESIAN_POINT('Ctrl Pts',(-0.144613108848303,-0.180075271725216,
0.0325484170155115));
#30997=CARTESIAN_POINT('Ctrl Pts',(0.0727946961077783,-0.219149774367173,
0.0436595820640553));
#30998=CARTESIAN_POINT('Ctrl Pts',(0.22359411788162,-0.057762978583554,
0.0547707471125989));
#30999=CARTESIAN_POINT('Ctrl Pts',(0.169827668332871,0.156494259322429,
0.0658819121611427));
#31000=CARTESIAN_POINT('Ctrl Pts',(-0.0393188016825179,0.227560800163251,
0.0769930772096863));
#31001=CARTESIAN_POINT('Ctrl Pts',(-0.212490816724285,0.090434536960108,
0.0881042422582301));
#31002=CARTESIAN_POINT('Ctrl Pts',(-0.19125222930514,-0.129434912039326,
0.0992154073067737));
#31003=CARTESIAN_POINT('Ctrl Pts',(0.00496630258143332,-0.230880650358359,
0.110326572355317));
#31004=CARTESIAN_POINT('Ctrl Pts',(0.196640931676781,-0.121090966106477,
0.121437737403861));
#31005=CARTESIAN_POINT('Ctrl Pts',(0.208405785032279,0.0994871990457256,
0.132548902452405));
#31006=CARTESIAN_POINT('Ctrl Pts',(0.0294968904732024,0.229042728261432,
0.143660067500948));
#31007=CARTESIAN_POINT('Ctrl Pts',(-0.176399147035948,0.149043619583305,
0.154771232549492));
#31008=CARTESIAN_POINT('Ctrl Pts',(-0.220904863824581,-0.0673178902258552,
0.165882397598036));
#31009=CARTESIAN_POINT('Ctrl Pts',(-0.0633012670336293,-0.222089176195486,
0.17699356264658));
#31010=CARTESIAN_POINT('Ctrl Pts',(0.152217643594786,-0.173667627565877,
0.188104727695123));
#31011=CARTESIAN_POINT('Ctrl Pts',(0.228470258285089,0.0336451535954383,
0.199215892743667));
#31012=CARTESIAN_POINT('Ctrl Pts',(0.0956918672404541,0.210175453516431,
0.210327057792211));
#31013=CARTESIAN_POINT('Ctrl Pts',(-0.124636506047609,0.194412953698174,
0.221438222840754));
#31014=CARTESIAN_POINT('Ctrl Pts',(-0.230932995110325,0.000779007092406014,
0.232549387889298));
#31015=CARTESIAN_POINT('Ctrl Pts',(-0.12594528285163,-0.193567664513544,
0.243660552937842));
#31016=CARTESIAN_POINT('Ctrl Pts',(0.0942717341349318,-0.21081625941051,
0.254771717986386));
#31017=CARTESIAN_POINT('Ctrl Pts',(0.228238070382781,-0.0351857683462,0.265882883034929));
#31018=CARTESIAN_POINT('Ctrl Pts',(0.153385834111148,0.172636731182735,
0.276994048083473));
#31019=CARTESIAN_POINT('Ctrl Pts',(-0.0618014955343493,0.222511191222357,
0.288105213132016));
#31020=CARTESIAN_POINT('Ctrl Pts',(-0.220445672440028,0.068806689849701,
0.299216378180561));
#31021=CARTESIAN_POINT('Ctrl Pts',(-0.177400663329184,-0.147850125855229,
0.310327543229104));
#31022=CARTESIAN_POINT('Ctrl Pts',(0.0279509811935462,-0.229236554058792,
0.321438708277648));
#31023=CARTESIAN_POINT('Ctrl Pts',(0.207729836817097,-0.100890881459812,
0.332549873326191));
#31024=CARTESIAN_POINT('Ctrl Pts',(0.197453422882556,0.11976143309821,0.343661038374735));
#31025=CARTESIAN_POINT('Ctrl Pts',(0.00652379087403971,0.230842143506323,
0.354772203423278));
#31026=CARTESIAN_POINT('Ctrl Pts',(-0.190374559216213,0.130721774273047,
0.365883368471823));
#31027=CARTESIAN_POINT('Ctrl Pts',(-0.213096254074054,-0.0889979863001003,
0.376994533520366));
#31028=CARTESIAN_POINT('Ctrl Pts',(-0.0408528604769679,-0.227292100295502,
0.38810569856891));
#31029=CARTESIAN_POINT('Ctrl Pts',(0.16876745272456,-0.15763312458598,0.399216863617453));
#31030=CARTESIAN_POINT('Ctrl Pts',(0.223979789625721,0.0562468568463683,
0.410328028665997));
#31031=CARTESIAN_POINT('Ctrl Pts',(0.0742695215461042,0.218665711155622,
0.421439193714541));
#31032=CARTESIAN_POINT('Ctrl Pts',(-0.143391090854028,0.181023893808443,
0.432550358763085));
#31033=CARTESIAN_POINT('Ctrl Pts',(-0.229860956455329,-0.0222395090620434,
0.443661523811628));
#31034=CARTESIAN_POINT('Ctrl Pts',(-0.106027445761331,-0.205155638019547,
0.454772688860172));
#31035=CARTESIAN_POINT('Ctrl Pts',(0.114812229735204,-0.200371672072451,
0.465883853908716));
#31036=CARTESIAN_POINT('Ctrl Pts',(0.230608404475241,-0.0122645363248325,
0.476995018957259));
#31037=CARTESIAN_POINT('Ctrl Pts',(0.135417351061808,0.187063615108022,
0.488106184005803));
#31038=CARTESIAN_POINT('Ctrl Pts',(-0.083669150175529,0.21524434574405,
0.499217349054346));
#31039=CARTESIAN_POINT('Ctrl Pts',(-0.226205440167697,0.0464946653328952,
0.510328514102891));
#31040=CARTESIAN_POINT('Ctrl Pts',(-0.161782842764492,-0.164793709991974,
0.521439679151433));
#31041=CARTESIAN_POINT('Ctrl Pts',(0.0506574022840452,-0.225309748257175,
0.532550844199978));
#31042=CARTESIAN_POINT('Ctrl Pts',(0.21675039941815,-0.0796863816342033,
0.543662009248521));
#31043=CARTESIAN_POINT('Ctrl Pts',(0.184535073495005,0.138843299139974,
0.554773174297065));
#31044=CARTESIAN_POINT('Ctrl Pts',(-0.01651427104253,0.230343078727826,
0.565884339345609));
#31045=CARTESIAN_POINT('Ctrl Pts',(-0.2024544512798,0.11109838082922,0.576995504394152));
#31046=CARTESIAN_POINT('Ctrl Pts',(-0.203165894515671,-0.109791959503082,
0.588106669442697));
#31047=CARTESIAN_POINT('Ctrl Pts',(-0.0179976902307884,-0.230231922661119,
0.599217834491239));
#31048=CARTESIAN_POINT('Ctrl Pts',(0.183636881720094,-0.140029106752845,
0.610328999539785));
#31049=CARTESIAN_POINT('Ctrl Pts',(0.217259204728728,0.0782885242326115,
0.621440164588326));
#31050=CARTESIAN_POINT('Ctrl Pts',(0.0521076907609949,0.224978762618687,
0.632551329636872));
#31051=CARTESIAN_POINT('Ctrl Pts',(-0.160717962682088,0.16583242004264,
0.643662494685413));
#31052=CARTESIAN_POINT('Ctrl Pts',(-0.226500243885858,-0.0450365916286509,
0.65477365973396));
#31053=CARTESIAN_POINT('Ctrl Pts',(-0.0850539171717745,-0.214700922773088,
0.665884824782501));
#31054=CARTESIAN_POINT('Ctrl Pts',(0.134209565723166,-0.187932029027199,
0.676995989831046));
#31055=CARTESIAN_POINT('Ctrl Pts',(0.230682622449346,0.0107788109627418,
0.68810715487959));
#31056=CARTESIAN_POINT('Ctrl Pts',(0.116100547839306,0.199627948587589,
0.699218319928133));
#31057=CARTESIAN_POINT('Ctrl Pts',(-0.104703729866326,0.205834360634882,
0.710329484976677));
#31058=CARTESIAN_POINT('Ctrl Pts',(-0.229712931099768,0.0237197038645086,
0.721440650025221));
#31059=CARTESIAN_POINT('Ctrl Pts',(-0.144554186745893,-0.180096480143545,
0.732551815073763));
#31060=CARTESIAN_POINT('Ctrl Pts',(0.072859438989827,-0.219139583863915,
0.743662980122308));
#31061=CARTESIAN_POINT('Ctrl Pts',(0.223612826941383,-0.0576884623911715,
0.75477414517085));
#31062=CARTESIAN_POINT('Ctrl Pts',(0.16977934979946,0.156542733614398,0.765885310219396));
#31063=CARTESIAN_POINT('Ctrl Pts',(-0.0393879040694563,0.227550539615811,
0.776996475267938));
#31064=CARTESIAN_POINT('Ctrl Pts',(-0.212518549811472,0.0903688057410859,
0.788107640316484));
#31065=CARTESIAN_POINT('Ctrl Pts',(-0.191212657747833,-0.129492758803799,
0.799218805365025));
#31066=CARTESIAN_POINT('Ctrl Pts',(0.00503667898133586,-0.230879377455661,
0.81032997041357));
#31067=CARTESIAN_POINT('Ctrl Pts',(0.196677879493939,-0.121030850518371,
0.821441135462113));
#31068=CARTESIAN_POINT('Ctrl Pts',(0.208375418707704,0.0995506903268707,
0.832552300510658));
#31069=CARTESIAN_POINT('Ctrl Pts',(0.0294270353677539,0.229051751091564,
0.8436634655592));
#31070=CARTESIAN_POINT('Ctrl Pts',(-0.176444601777748,0.14898978999011,
0.854774630607746));
#31071=CARTESIAN_POINT('Ctrl Pts',(-0.22088431932234,-0.0673852547682493,
0.865885795656288));
#31072=CARTESIAN_POINT('Ctrl Pts',(-0.0632335256349382,-0.22210847899434,
0.876996960704833));
#31073=CARTESIAN_POINT('Ctrl Pts',(0.152270606837662,-0.173621188252162,
0.888108125753376));
#31074=CARTESIAN_POINT('Ctrl Pts',(0.228459985995541,0.0337148347205355,
0.899219290801919));
#31075=CARTESIAN_POINT('Ctrl Pts',(0.0956277562497704,0.210204633917866,
0.910330455850463));
#31076=CARTESIAN_POINT('Ctrl Pts',(-0.12469579560031,0.194374924182257,
0.921441620899007));
#31077=CARTESIAN_POINT('Ctrl Pts',(-0.230933226540692,0.000708579792413808,
0.932552785947551));
#31078=CARTESIAN_POINT('Ctrl Pts',(-0.125886228368054,-0.193606087509586,
0.943663950996094));
#31079=CARTESIAN_POINT('Ctrl Pts',(0.0943360139257667,-0.210787462610152,
0.954775116044639));
#31080=CARTESIAN_POINT('Ctrl Pts',(0.228248823506631,-0.0351162152961091,
0.965886281093181));
#31081=CARTESIAN_POINT('Ctrl Pts',(0.153333110744206,0.172683627576032,
0.976997446141726));
#31082=CARTESIAN_POINT('Ctrl Pts',(-0.0618692454411617,0.222492101746939,
0.988108611190268));
#31083=CARTESIAN_POINT('Ctrl Pts',(-0.220466868021367,0.0687398848825245,
0.999219776238814));
#31084=CARTESIAN_POINT('Ctrl Pts',(-0.17735514221838,-0.147905058047522,
1.01033094128735));
#31085=CARTESIAN_POINT('Ctrl Pts',(0.0280201048116106,-0.229226437530741,
1.0214421063359));
#31086=CARTESIAN_POINT('Ctrl Pts',(0.207762111854432,-0.10083052618152,
1.03255327138444));
#31087=CARTESIAN_POINT('Ctrl Pts',(0.197414006873683,0.119827380577986,
1.04366443643299));
#31088=CARTESIAN_POINT('Ctrl Pts',(0.00645886152005097,0.230833217918201,
1.05477560148153));
#31089=CARTESIAN_POINT('Ctrl Pts',(-0.190424854748374,0.130684465150768,
1.06588676653008));
#31090=CARTESIAN_POINT('Ctrl Pts',(-0.213049227679005,-0.0891025387309722,
1.07699793157862));
#31091=CARTESIAN_POINT('Ctrl Pts',(-0.0408214485225542,-0.227228942196666,
1.08810909662716));
#31092=CARTESIAN_POINT('Ctrl Pts',(0.168888461736298,-0.15772814986318,
1.09922026167571));
#31093=CARTESIAN_POINT('Ctrl Pts',(0.223817187934597,0.0566161966084782,
1.11033142672425));
#31094=CARTESIAN_POINT('Ctrl Pts',(0.124300218570944,0.164165746435707,
1.11773887008995));
#31095=CARTESIAN_POINT('Ctrl Pts',(0.0627850911123727,0.1850383536838,1.12144259177279));
#31096=CARTESIAN_POINT('Ctrl Pts',(0.105793541951254,-0.14823699524473,
-0.0153382721514713));
#31097=CARTESIAN_POINT('Ctrl Pts',(0.155074231467859,-0.113066431478549,
-0.0116345504686234));
#31098=CARTESIAN_POINT('Ctrl Pts',(0.214955001436596,0.00967274517879857,
-0.00422710710292769));
#31099=CARTESIAN_POINT('Ctrl Pts',(0.108290436090784,0.186174541551099,
0.00688405794561606));
#31100=CARTESIAN_POINT('Ctrl Pts',(-0.0975409307071879,0.191793784975909,
0.0179952229941597));
#31101=CARTESIAN_POINT('Ctrl Pts',(-0.214083151712633,0.022213180716797,
0.0291063880427034));
#31102=CARTESIAN_POINT('Ctrl Pts',(-0.134782279118508,-0.167833716661673,
0.0402175530912472));
#31103=CARTESIAN_POINT('Ctrl Pts',(0.0678460972679723,-0.204251926348524,
0.0513287181397908));
#31104=CARTESIAN_POINT('Ctrl Pts',(0.208394142450739,-0.0538362390807298,
0.0624398831883346));
#31105=CARTESIAN_POINT('Ctrl Pts',(0.158282747515632,0.145855746470163,
0.0735510482368781));
#31106=CARTESIAN_POINT('Ctrl Pts',(-0.0366459012269607,0.212091168831785,
0.084662213285422));
#31107=CARTESIAN_POINT('Ctrl Pts',(-0.198045646054783,0.0842867780077688,
0.0957733783339656));
#31108=CARTESIAN_POINT('Ctrl Pts',(-0.178250862301028,-0.120635899339281,
0.106884543382509));
#31109=CARTESIAN_POINT('Ctrl Pts',(0.00462869228141735,-0.215185334908375,
0.117995708431053));
#31110=CARTESIAN_POINT('Ctrl Pts',(0.183273239545565,-0.112859176615955,
0.129106873479597));
#31111=CARTESIAN_POINT('Ctrl Pts',(0.194238315681312,0.0927240382098824,
0.14021803852814));
#31112=CARTESIAN_POINT('Ctrl Pts',(0.0274916856192995,0.213472355144377,
0.151329203576684));
#31113=CARTESIAN_POINT('Ctrl Pts',(-0.164407495706399,0.138911602796551,
0.162440368625228));
#31114=CARTESIAN_POINT('Ctrl Pts',(-0.20588770445336,-0.062741605808422,
0.173551533673771));
#31115=CARTESIAN_POINT('Ctrl Pts',(-0.0589980335104445,-0.206991507018771,
0.184662698722315));
#31116=CARTESIAN_POINT('Ctrl Pts',(0.141869855984326,-0.161861665507704,
0.195773863770859));
#31117=CARTESIAN_POINT('Ctrl Pts',(0.21293880179812,0.0313579489369987,
0.206885028819403));
#31118=CARTESIAN_POINT('Ctrl Pts',(0.0891867138635642,0.195887681727571,
0.217996193867946));
#31119=CARTESIAN_POINT('Ctrl Pts',(-0.116163690001897,0.18119671998123,
0.22910735891649));
#31120=CARTESIAN_POINT('Ctrl Pts',(-0.21523412125303,0.00072605002547781,
0.240218523965033));
#31121=CARTESIAN_POINT('Ctrl Pts',(-0.11738349588193,-0.180408893734178,
0.251329689013577));
#31122=CARTESIAN_POINT('Ctrl Pts',(0.0878631217069615,-0.196484925501419,
0.262440854062121));
#31123=CARTESIAN_POINT('Ctrl Pts',(0.212722398078527,-0.0327938323711113,
0.273552019110664));
#31124=CARTESIAN_POINT('Ctrl Pts',(0.142958632662274,0.160900849678758,
0.284663184159209));
#31125=CARTESIAN_POINT('Ctrl Pts',(-0.057600216794938,0.207384833374845,
0.295774349207752));
#31126=CARTESIAN_POINT('Ctrl Pts',(-0.205459728996263,0.0641291965189069,
0.306885514256296));
#31127=CARTESIAN_POINT('Ctrl Pts',(-0.165340928710165,-0.137799243024573,
0.317996679304839));
#31128=CARTESIAN_POINT('Ctrl Pts',(0.0260508675794864,-0.213653004623031,
0.329107844353384));
#31129=CARTESIAN_POINT('Ctrl Pts',(0.193608318568785,-0.0940322979965331,
0.340219009401926));
#31130=CARTESIAN_POINT('Ctrl Pts',(0.184030497427301,0.111620025542831,
0.351330174450471));
#31131=CARTESIAN_POINT('Ctrl Pts',(0.00608030219043116,0.215149445760286,
0.362441339499014));
#31132=CARTESIAN_POINT('Ctrl Pts',(-0.177432856410404,0.121835280406139,
0.373552504547559));
#31133=CARTESIAN_POINT('Ctrl Pts',(-0.198609925645444,-0.0829478843655077,
0.384663669596101));
#31134=CARTESIAN_POINT('Ctrl Pts',(-0.0380756743800589,-0.211840735237885,
0.395774834644646));
#31135=CARTESIAN_POINT('Ctrl Pts',(0.157294605588646,-0.14691719143219,
0.406885999693188));
#31136=CARTESIAN_POINT('Ctrl Pts',(0.208753596148093,0.0524231836199493,
0.417997164741733));
#31137=CARTESIAN_POINT('Ctrl Pts',(0.0692206637610257,0.203800769856489,
0.429108329790276));
#31138=CARTESIAN_POINT('Ctrl Pts',(-0.133643334165982,0.168717851215016,
0.44021949483882));
#31139=CARTESIAN_POINT('Ctrl Pts',(-0.21423496001257,-0.0207276625316418,
0.451330659887364));
#31140=CARTESIAN_POINT('Ctrl Pts',(-0.0988196775702872,-0.191209114350017,
0.462441824935908));
#31141=CARTESIAN_POINT('Ctrl Pts',(0.107007270071357,-0.186750363419964,
0.473552989984451));
#31142=CARTESIAN_POINT('Ctrl Pts',(0.21493159635798,-0.011430790551128,
0.484664155032995));
#31143=CARTESIAN_POINT('Ctrl Pts',(0.126211650891535,0.174346990983058,
0.495775320081538));
#31144=CARTESIAN_POINT('Ctrl Pts',(-0.0779813036479037,0.200611989589323,
0.506886485130082));
#31145=CARTESIAN_POINT('Ctrl Pts',(-0.21082794649543,0.0433339481484583,
0.517997650178626));
#31146=CARTESIAN_POINT('Ctrl Pts',(-0.150784810891129,-0.153590998727594,
0.529108815227169));
#31147=CARTESIAN_POINT('Ctrl Pts',(0.0472137013611209,-0.209993143910453,
0.540219980275713));
#31148=CARTESIAN_POINT('Ctrl Pts',(0.202015661416081,-0.0742692845544967,
0.551331145324257));
#31149=CARTESIAN_POINT('Ctrl Pts',(0.171990340163759,0.129404702294652,
0.562442310372801));
#31150=CARTESIAN_POINT('Ctrl Pts',(-0.0153916274037652,0.214684307510999,
0.573553475421344));
#31151=CARTESIAN_POINT('Ctrl Pts',(-0.188691554856225,0.103545889399597,
0.584664640469888));
#31152=CARTESIAN_POINT('Ctrl Pts',(-0.189354634030427,-0.102328278871562,
0.595775805518432));
#31153=CARTESIAN_POINT('Ctrl Pts',(-0.0167742034418123,-0.21458070785722,
0.606886970566975));
#31154=CARTESIAN_POINT('Ctrl Pts',(0.171153207655705,-0.130509898455162,
0.61799813561552));
#31155=CARTESIAN_POINT('Ctrl Pts',(0.202489878034016,0.0729664537947597,
0.629109300664062));
#31156=CARTESIAN_POINT('Ctrl Pts',(0.0485653989206222,0.209684658745684,
0.640220465712607));
#31157=CARTESIAN_POINT('Ctrl Pts',(-0.149792321581985,0.154559097049293,
0.65133163076115));
#31158=CARTESIAN_POINT('Ctrl Pts',(-0.211102709394471,-0.041974994603061,
0.662442795809694));
#31159=CARTESIAN_POINT('Ctrl Pts',(-0.079271933890819,-0.20010550862688,
0.673553960858237));
#31160=CARTESIAN_POINT('Ctrl Pts',(0.125085971055702,-0.17515636994031,
0.684665125906781));
#31161=CARTESIAN_POINT('Ctrl Pts',(0.215000768978506,0.0100460651134341,
0.695776290955325));
#31162=CARTESIAN_POINT('Ctrl Pts',(0.108208008038219,0.186057198414926,
0.706887456003868));
#31163=CARTESIAN_POINT('Ctrl Pts',(-0.0975859481618359,0.191841697258389,
0.717998621052413));
#31164=CARTESIAN_POINT('Ctrl Pts',(-0.214096997451993,0.0221072333783236,
0.729109786100956));
#31165=CARTESIAN_POINT('Ctrl Pts',(-0.134727362553083,-0.167853483327237,
0.7402209511495));
#31166=CARTESIAN_POINT('Ctrl Pts',(0.0679064389152043,-0.204242428597833,
0.751332116198043));
#31167=CARTESIAN_POINT('Ctrl Pts',(0.208411579664662,-0.0537667885148679,
0.762443281246587));
#31168=CARTESIAN_POINT('Ctrl Pts',(0.158237713686343,0.14590092546951,0.773554446295131));
#31169=CARTESIAN_POINT('Ctrl Pts',(-0.0367103060190181,0.21208160579853,
0.784665611343674));
#31170=CARTESIAN_POINT('Ctrl Pts',(-0.198071493840836,0.0842255152109201,
0.795776776392219));
#31171=CARTESIAN_POINT('Ctrl Pts',(-0.178213980826558,-0.120689813668469,
0.80688794144076));
#31172=CARTESIAN_POINT('Ctrl Pts',(0.00469428447876819,-0.215184148537872,
0.817999106489307));
#31173=CARTESIAN_POINT('Ctrl Pts',(0.183307675642296,-0.112803147698245,
0.829110271537848));
#31174=CARTESIAN_POINT('Ctrl Pts',(0.194210013665906,0.0927832133403047,
0.840221436586394));
#31175=CARTESIAN_POINT('Ctrl Pts',(0.0274265792786954,0.213480764600607,
0.851332601634936));
#31176=CARTESIAN_POINT('Ctrl Pts',(-0.164449860425235,0.138861432550488,
0.86244376668348));
#31177=CARTESIAN_POINT('Ctrl Pts',(-0.205868556570727,-0.0628043908949741,
0.873554931732024));
#31178=CARTESIAN_POINT('Ctrl Pts',(-0.0589348971863656,-0.207009497609277,
0.884666096780567));
#31179=CARTESIAN_POINT('Ctrl Pts',(0.141919218774748,-0.161818383148359,
0.895777261829112));
#31180=CARTESIAN_POINT('Ctrl Pts',(0.212929227820989,0.0314228931244718,
0.906888426877654));
#31181=CARTESIAN_POINT('Ctrl Pts',(0.0891269611515884,0.195914878439144,
0.9179995919262));
#31182=CARTESIAN_POINT('Ctrl Pts',(-0.116218949038264,0.181161275719849,
0.929110756974741));
#31183=CARTESIAN_POINT('Ctrl Pts',(-0.215234336950711,0.000660410388236847,
0.940221922023287));
#31184=CARTESIAN_POINT('Ctrl Pts',(-0.117328455934639,-0.180444704726821,
0.951333087071829));
#31185=CARTESIAN_POINT('Ctrl Pts',(0.0879230317440182,-0.196458086313641,
0.962444252120374));
#31186=CARTESIAN_POINT('Ctrl Pts',(0.212732420202743,-0.0327290075520782,
0.973555417168917));
#31187=CARTESIAN_POINT('Ctrl Pts',(0.142909493440969,0.160944558045319,
0.98466658221746));
#31188=CARTESIAN_POINT('Ctrl Pts',(-0.0576633610487541,0.207367041606005,
0.995777747266004));
#31189=CARTESIAN_POINT('Ctrl Pts',(-0.205479483697499,0.0640669329675303,
1.00688891231455));
#31190=CARTESIAN_POINT('Ctrl Pts',(-0.165298502134104,-0.137850440914814,
1.01800007736309));
#31191=CARTESIAN_POINT('Ctrl Pts',(0.026115292159373,-0.213643575818697,
1.02911124241164));
#31192=CARTESIAN_POINT('Ctrl Pts',(0.193638399542254,-0.0939760456828254,
1.04022240746018));
#31193=CARTESIAN_POINT('Ctrl Pts',(0.183993760927049,0.111681489898982,
1.05133357250872));
#31194=CARTESIAN_POINT('Ctrl Pts',(0.00601978674766102,0.215141126935532,
1.06244473755726));
#31195=CARTESIAN_POINT('Ctrl Pts',(-0.177479732841649,0.121800507565884,
1.07355590260581));
#31196=CARTESIAN_POINT('Ctrl Pts',(-0.198566096114678,-0.0830453293000129,
1.08466706765435));
#31197=CARTESIAN_POINT('Ctrl Pts',(-0.0380463978169507,-0.211781870639967,
1.0957782327029));
#31198=CARTESIAN_POINT('Ctrl Pts',(0.157407388382168,-0.147005756870945,
1.10688939775144));
#31199=CARTESIAN_POINT('Ctrl Pts',(0.208602048154327,0.0527674155869038,
1.11800056279999));
#31200=CARTESIAN_POINT('Ctrl Pts',(0.115850263419028,0.153005724266717,
1.12540800616568));
#31201=CARTESIAN_POINT('Ctrl Pts',(0.0585169473375027,0.172459407258861,
1.12911172784853));
#31202=CARTESIAN_POINT('Ctrl Pts',(0.0980771099081375,-0.137424797458507,
-0.00766913607573581));
#31203=CARTESIAN_POINT('Ctrl Pts',(0.143763335295088,-0.104819525110066,
-0.00396541439288791));
#31204=CARTESIAN_POINT('Ctrl Pts',(0.199276486185844,0.0089672287600667,
0.00344202897280782));
#31205=CARTESIAN_POINT('Ctrl Pts',(0.100391884103562,0.172595232535247,
0.0145531940213516));
#31206=CARTESIAN_POINT('Ctrl Pts',(-0.0904264325124765,0.177804616253862,
0.0256643590698952));
#31207=CARTESIAN_POINT('Ctrl Pts',(-0.198468227953599,0.020592982580867,
0.036775524118439));
#31208=CARTESIAN_POINT('Ctrl Pts',(-0.124951449388714,-0.155592161598129,
0.0478866891669827));
#31209=CARTESIAN_POINT('Ctrl Pts',(0.0628974984281669,-0.189354078329874,
0.0589978542155263));
#31210=CARTESIAN_POINT('Ctrl Pts',(0.193194167019859,-0.0499094995779056,
0.07010901926407));
#31211=CARTESIAN_POINT('Ctrl Pts',(0.146737826698393,0.135217233617898,
0.0812201843126137));
#31212=CARTESIAN_POINT('Ctrl Pts',(-0.0339730007714042,0.196621537500318,
0.0923313493611574));
#31213=CARTESIAN_POINT('Ctrl Pts',(-0.18360047538528,0.07813901905543,0.103442514409701));
#31214=CARTESIAN_POINT('Ctrl Pts',(-0.165249495296916,-0.111836886639236,
0.114553679458245));
#31215=CARTESIAN_POINT('Ctrl Pts',(0.00429108198140191,-0.199490019458391,
0.125664844506789));
#31216=CARTESIAN_POINT('Ctrl Pts',(0.169905547414348,-0.104627387125433,
0.136776009555332));
#31217=CARTESIAN_POINT('Ctrl Pts',(0.180070846330345,0.0859608773740392,
0.147887174603876));
#31218=CARTESIAN_POINT('Ctrl Pts',(0.0254864807653961,0.197901982027321,
0.15899833965242));
#31219=CARTESIAN_POINT('Ctrl Pts',(-0.152415844376849,0.128779586009797,
0.170109504700963));
#31220=CARTESIAN_POINT('Ctrl Pts',(-0.190870545082139,-0.0581653213909888,
0.181220669749507));
#31221=CARTESIAN_POINT('Ctrl Pts',(-0.0546947999872595,-0.191893837842057,
0.192331834798051));
#31222=CARTESIAN_POINT('Ctrl Pts',(0.131522068373867,-0.150055703449532,
0.203442999846594));
#31223=CARTESIAN_POINT('Ctrl Pts',(0.197407345311151,0.0290707442785592,
0.214554164895138));
#31224=CARTESIAN_POINT('Ctrl Pts',(0.0826815604866742,0.181599909938712,
0.225665329943681));
#31225=CARTESIAN_POINT('Ctrl Pts',(-0.107690873956185,0.167980486264285,
0.236776494992226));
#31226=CARTESIAN_POINT('Ctrl Pts',(-0.199535247395734,0.000673092958549589,
0.247887660040769));
#31227=CARTESIAN_POINT('Ctrl Pts',(-0.10882170891223,-0.167250122954812,
0.258998825089313));
#31228=CARTESIAN_POINT('Ctrl Pts',(0.0814545092789914,-0.182153591592328,
0.270109990137857));
#31229=CARTESIAN_POINT('Ctrl Pts',(0.197206725774273,-0.0304018963960226,
0.2812211551864));
#31230=CARTESIAN_POINT('Ctrl Pts',(0.1325314312134,0.149164968174781,0.292332320234944));
#31231=CARTESIAN_POINT('Ctrl Pts',(-0.0533989380555266,0.192258475527334,
0.303443485283487));
#31232=CARTESIAN_POINT('Ctrl Pts',(-0.190473785552499,0.0594517031881129,
0.314554650332031));
#31233=CARTESIAN_POINT('Ctrl Pts',(-0.153281194091147,-0.127748360193918,
0.325665815380575));
#31234=CARTESIAN_POINT('Ctrl Pts',(0.0241507539654265,-0.198069455187271,
0.336776980429119));
#31235=CARTESIAN_POINT('Ctrl Pts',(0.179486800320472,-0.0871737145332536,
0.347888145477662));
#31236=CARTESIAN_POINT('Ctrl Pts',(0.170607571972046,0.103478617987453,
0.358999310526206));
#31237=CARTESIAN_POINT('Ctrl Pts',(0.00563681350682242,0.199456748014249,
0.37011047557475));
#31238=CARTESIAN_POINT('Ctrl Pts',(-0.164491153604594,0.11294878653923,
0.381221640623293));
#31239=CARTESIAN_POINT('Ctrl Pts',(-0.184123597216834,-0.0768977824309152,
0.392332805671837));
#31240=CARTESIAN_POINT('Ctrl Pts',(-0.0352984882831497,-0.196389370180267,
0.403443970720381));
#31241=CARTESIAN_POINT('Ctrl Pts',(0.145821758452731,-0.136201258278399,
0.414555135768924));
#31242=CARTESIAN_POINT('Ctrl Pts',(0.193527402670466,0.0485995103935303,
0.425666300817468));
#31243=CARTESIAN_POINT('Ctrl Pts',(0.0641718059759468,0.188935828557357,
0.436777465866012));
#31244=CARTESIAN_POINT('Ctrl Pts',(-0.123895577477937,0.156411808621589,
0.447888630914555));
#31245=CARTESIAN_POINT('Ctrl Pts',(-0.198608963569812,-0.01921581600124,
0.458999795963099));
#31246=CARTESIAN_POINT('Ctrl Pts',(-0.0916119093792434,-0.177262590680487,
0.470110961011643));
#31247=CARTESIAN_POINT('Ctrl Pts',(0.0992023104075105,-0.173129054767478,
0.481222126060186));
#31248=CARTESIAN_POINT('Ctrl Pts',(0.199254788240719,-0.0105970447774237,
0.49233329110873));
#31249=CARTESIAN_POINT('Ctrl Pts',(0.117005950721263,0.161630366858093,
0.503444456157274));
#31250=CARTESIAN_POINT('Ctrl Pts',(-0.0722934571202785,0.185979633434597,
0.514555621205818));
#31251=CARTESIAN_POINT('Ctrl Pts',(-0.195450452823164,0.0401732309640217,
0.525666786254361));
#31252=CARTESIAN_POINT('Ctrl Pts',(-0.139786779017765,-0.142388287463214,
0.536777951302905));
#31253=CARTESIAN_POINT('Ctrl Pts',(0.0437700004381964,-0.19467653956373,
0.547889116351449));
#31254=CARTESIAN_POINT('Ctrl Pts',(0.187280923414012,-0.0688521874747905,
0.559000281399993));
#31255=CARTESIAN_POINT('Ctrl Pts',(0.159445606832513,0.119966105449332,
0.570111446448536));
#31256=CARTESIAN_POINT('Ctrl Pts',(-0.0142689837650004,0.199025536294172,
0.581222611497081));
#31257=CARTESIAN_POINT('Ctrl Pts',(-0.174928658432651,0.0959933979699734,
0.592333776545623));
#31258=CARTESIAN_POINT('Ctrl Pts',(-0.175543373545183,-0.0948645982400418,
0.603444941594168));
#31259=CARTESIAN_POINT('Ctrl Pts',(-0.0155507166528361,-0.198929493053321,
0.61455610664271));
#31260=CARTESIAN_POINT('Ctrl Pts',(0.158669533591315,-0.120990690157479,
0.625667271691256));
#31261=CARTESIAN_POINT('Ctrl Pts',(0.187720551339304,0.0676443833569079,
0.636778436739797));
#31262=CARTESIAN_POINT('Ctrl Pts',(0.0450231070802491,0.194390554872681,
0.647889601788343));
#31263=CARTESIAN_POINT('Ctrl Pts',(-0.138866680481881,0.143285774055946,
0.659000766836885));
#31264=CARTESIAN_POINT('Ctrl Pts',(-0.195705174903083,-0.038913397577471,
0.67011193188543));
#31265=CARTESIAN_POINT('Ctrl Pts',(-0.0734899506098636,-0.185510094480672,
0.681223096933973));
#31266=CARTESIAN_POINT('Ctrl Pts',(0.115962376388238,-0.162380710853421,
0.692334261982516));
#31267=CARTESIAN_POINT('Ctrl Pts',(0.199318915507666,0.00931331926412601,
0.703445427031061));
#31268=CARTESIAN_POINT('Ctrl Pts',(0.100315468237132,0.172486448242263,
0.714556592079604));
#31269=CARTESIAN_POINT('Ctrl Pts',(-0.0904681664573454,0.177849033881895,
0.725667757128148));
#31270=CARTESIAN_POINT('Ctrl Pts',(-0.198481063804218,0.0204947628921387,
0.736778922176691));
#31271=CARTESIAN_POINT('Ctrl Pts',(-0.124900538360275,-0.155610486510929,
0.747890087225236));
#31272=CARTESIAN_POINT('Ctrl Pts',(0.0629534388405818,-0.189345273331751,
0.759001252273779));
#31273=CARTESIAN_POINT('Ctrl Pts',(0.193210332387941,-0.0498451146385645,
0.770112417322323));
#31274=CARTESIAN_POINT('Ctrl Pts',(0.146696077573226,0.135259117324623,
0.781223582370866));
#31275=CARTESIAN_POINT('Ctrl Pts',(-0.0340327079685797,0.196612671981249,
0.79233474741941));
#31276=CARTESIAN_POINT('Ctrl Pts',(-0.1836244378702,0.0780822246807544,
0.803445912467955));
#31277=CARTESIAN_POINT('Ctrl Pts',(-0.165215303905282,-0.111886868533138,
0.814557077516496));
#31278=CARTESIAN_POINT('Ctrl Pts',(0.00435188997620014,-0.199488919620082,
0.825668242565042));
#31279=CARTESIAN_POINT('Ctrl Pts',(0.169937471790653,-0.104575444878119,
0.836779407613584));
#31280=CARTESIAN_POINT('Ctrl Pts',(0.180044608624107,0.0860157363537389,
0.847890572662129));
#31281=CARTESIAN_POINT('Ctrl Pts',(0.0254261231896373,0.197909778109651,
0.859001737710672));
#31282=CARTESIAN_POINT('Ctrl Pts',(-0.152455119072723,0.128733075110866,
0.870112902759215));
#31283=CARTESIAN_POINT('Ctrl Pts',(-0.190852793819114,-0.058223527021699,
0.88122406780776));
#31284=CARTESIAN_POINT('Ctrl Pts',(-0.0546362687377931,-0.191910516224214,
0.892335232856302));
#31285=CARTESIAN_POINT('Ctrl Pts',(0.131567830711834,-0.150015578044556,
0.903446397904849));
#31286=CARTESIAN_POINT('Ctrl Pts',(0.197398469646436,0.0291309515284085,
0.914557562953389));
#31287=CARTESIAN_POINT('Ctrl Pts',(0.0826261660534066,0.181625122960423,
0.925668728001935));
#31288=CARTESIAN_POINT('Ctrl Pts',(-0.107742102476217,0.167947627257441,
0.936779893050478));
#31289=CARTESIAN_POINT('Ctrl Pts',(-0.199535447360731,0.000612240984059651,
0.947891058099021));
#31290=CARTESIAN_POINT('Ctrl Pts',(-0.108770683501224,-0.167283321944057,
0.959002223147566));
#31291=CARTESIAN_POINT('Ctrl Pts',(0.0815100495622697,-0.182128710017129,
0.970113388196108));
#31292=CARTESIAN_POINT('Ctrl Pts',(0.197216016898856,-0.0303417998080474,
0.981224553244654));
#31293=CARTESIAN_POINT('Ctrl Pts',(0.132485876137733,0.149205488514605,
0.992335718293196));
#31294=CARTESIAN_POINT('Ctrl Pts',(-0.0534574766563464,0.19224198146507,
1.00344688334174));
#31295=CARTESIAN_POINT('Ctrl Pts',(-0.190492099373632,0.0593939810525364,
1.01455804839028));
#31296=CARTESIAN_POINT('Ctrl Pts',(-0.153241862049827,-0.127795823782107,
1.02566921343883));
#31297=CARTESIAN_POINT('Ctrl Pts',(0.0242104795071353,-0.198060714106653,
1.03678037848737));
#31298=CARTESIAN_POINT('Ctrl Pts',(0.179514687230076,-0.0871215651841315,
1.04789154353591));
#31299=CARTESIAN_POINT('Ctrl Pts',(0.170573514980415,0.103535599219979,
1.05900270858446));
#31300=CARTESIAN_POINT('Ctrl Pts',(0.0055807119752709,0.199449035952863,
1.070113873633));
#31301=CARTESIAN_POINT('Ctrl Pts',(-0.164534610934924,0.112916549981001,
1.08122503868155));
#31302=CARTESIAN_POINT('Ctrl Pts',(-0.184082964550351,-0.0769881198690536,
1.09233620373009));
#31303=CARTESIAN_POINT('Ctrl Pts',(-0.0352713471113472,-0.196334799083268,
1.10344736877863));
#31304=CARTESIAN_POINT('Ctrl Pts',(0.145926315028038,-0.136283363878709,
1.11455853382718));
#31305=CARTESIAN_POINT('Ctrl Pts',(0.193386908374058,0.0489186345653294,
1.12566969887572));
#31306=CARTESIAN_POINT('Ctrl Pts',(0.107400308267113,0.141845702097726,
1.13307714224142));
#31307=CARTESIAN_POINT('Ctrl Pts',(0.0542488035626326,0.159880460833922,
1.13678086392426));
#31308=CARTESIAN_POINT('Ctrl Pts',(0.0903606778650208,-0.126612599672284,
-2.77555756156289E-16));
#31309=CARTESIAN_POINT('Ctrl Pts',(0.132452439122316,-0.0965726187415828,
0.00370372168284762));
#31310=CARTESIAN_POINT('Ctrl Pts',(0.183597970935092,0.00826171234133487,
0.0111111650485434));
#31311=CARTESIAN_POINT('Ctrl Pts',(0.0924933321163406,0.159015923519395,
0.0222223300970871));
#31312=CARTESIAN_POINT('Ctrl Pts',(-0.0833119343177651,0.163815447531815,
0.0333334951456308));
#31313=CARTESIAN_POINT('Ctrl Pts',(-0.182853304194564,0.018972784444937,
0.0444446601941745));
#31314=CARTESIAN_POINT('Ctrl Pts',(-0.115120619658919,-0.143350606534586,
0.0555558252427182));
#31315=CARTESIAN_POINT('Ctrl Pts',(0.0579488995883613,-0.174456230311225,
0.0666669902912619));
#31316=CARTESIAN_POINT('Ctrl Pts',(0.177994191588978,-0.0459827600750814,
0.0777781553398056));
#31317=CARTESIAN_POINT('Ctrl Pts',(0.135192905881154,0.124578720765632,
0.0888893203883492));
#31318=CARTESIAN_POINT('Ctrl Pts',(-0.0313001003158473,0.181151906168851,
0.100000485436893));
#31319=CARTESIAN_POINT('Ctrl Pts',(-0.169155304715778,0.0719912601030908,
0.111111650485437));
#31320=CARTESIAN_POINT('Ctrl Pts',(-0.152248128292804,-0.103037873939191,
0.12222281553398));
#31321=CARTESIAN_POINT('Ctrl Pts',(0.00395347168138628,-0.183794704008407,
0.133333980582524));
#31322=CARTESIAN_POINT('Ctrl Pts',(0.156537855283131,-0.0963955976349113,
0.144445145631068));
#31323=CARTESIAN_POINT('Ctrl Pts',(0.165903376979378,0.0791977165381959,
0.155556310679611));
#31324=CARTESIAN_POINT('Ctrl Pts',(0.0234812759114929,0.182331608910266,
0.166667475728155));
#31325=CARTESIAN_POINT('Ctrl Pts',(-0.1404241930473,0.118647569223042,0.177778640776699));
#31326=CARTESIAN_POINT('Ctrl Pts',(-0.175853385710917,-0.0535890369735552,
0.188889805825242));
#31327=CARTESIAN_POINT('Ctrl Pts',(-0.0503915664640746,-0.176796168665343,
0.200000970873786));
#31328=CARTESIAN_POINT('Ctrl Pts',(0.121174280763407,-0.138249741391359,
0.21111213592233));
#31329=CARTESIAN_POINT('Ctrl Pts',(0.181875888824183,0.0267835396201195,
0.222223300970874));
#31330=CARTESIAN_POINT('Ctrl Pts',(0.0761764071097843,0.167312138149853,
0.233334466019417));
#31331=CARTESIAN_POINT('Ctrl Pts',(-0.0992180579104728,0.154764252547341,
0.244445631067961));
#31332=CARTESIAN_POINT('Ctrl Pts',(-0.183836373538439,0.000620135891621234,
0.255556796116504));
#31333=CARTESIAN_POINT('Ctrl Pts',(-0.10025992194253,-0.154091352175446,
0.266667961165049));
#31334=CARTESIAN_POINT('Ctrl Pts',(0.0750458968510211,-0.167822257683237,
0.277779126213592));
#31335=CARTESIAN_POINT('Ctrl Pts',(0.181691053470019,-0.0280099604209337,
0.288890291262136));
#31336=CARTESIAN_POINT('Ctrl Pts',(0.122104229764526,0.137429086670804,
0.30000145631068));
#31337=CARTESIAN_POINT('Ctrl Pts',(-0.0491976593161155,0.177132117679823,
0.311112621359223));
#31338=CARTESIAN_POINT('Ctrl Pts',(-0.175487842108734,0.0547742098573187,
0.322223786407767));
#31339=CARTESIAN_POINT('Ctrl Pts',(-0.141221459472129,-0.117697477363263,
0.33333495145631));
#31340=CARTESIAN_POINT('Ctrl Pts',(0.0222506403513669,-0.18248590575151,
0.344446116504855));
#31341=CARTESIAN_POINT('Ctrl Pts',(0.165365282072159,-0.0803151310699741,
0.355557281553397));
#31342=CARTESIAN_POINT('Ctrl Pts',(0.157184646516792,0.0953372104320743,
0.366668446601942));
#31343=CARTESIAN_POINT('Ctrl Pts',(0.00519332482321354,0.183764050268212,
0.377779611650485));
#31344=CARTESIAN_POINT('Ctrl Pts',(-0.151549450798785,0.104062292672322,
0.388890776699029));
#31345=CARTESIAN_POINT('Ctrl Pts',(-0.169637268788223,-0.0708476804963227,
0.400001941747572));
#31346=CARTESIAN_POINT('Ctrl Pts',(-0.0325213021862407,-0.180938005122649,
0.411113106796117));
#31347=CARTESIAN_POINT('Ctrl Pts',(0.134348911316817,-0.125485325124609,
0.42222427184466));
#31348=CARTESIAN_POINT('Ctrl Pts',(0.178301209192838,0.0447758371671112,
0.433335436893204));
#31349=CARTESIAN_POINT('Ctrl Pts',(0.0591229481908682,0.174070887258225,
0.444446601941748));
#31350=CARTESIAN_POINT('Ctrl Pts',(-0.114147820789891,0.144105766028162,
0.455557766990291));
#31351=CARTESIAN_POINT('Ctrl Pts',(-0.182982967127054,-0.0177039694708382,
0.466668932038835));
#31352=CARTESIAN_POINT('Ctrl Pts',(-0.0844041411881997,-0.163316067010957,
0.477780097087378));
#31353=CARTESIAN_POINT('Ctrl Pts',(0.0913973507436636,-0.159507746114991,
0.488891262135923));
#31354=CARTESIAN_POINT('Ctrl Pts',(0.183577980123458,-0.00976329900371924,
0.500002427184466));
#31355=CARTESIAN_POINT('Ctrl Pts',(0.10780025055099,0.148913742733129,0.51111359223301));
#31356=CARTESIAN_POINT('Ctrl Pts',(-0.0666056105926533,0.17134727727987,
0.522224757281553));
#31357=CARTESIAN_POINT('Ctrl Pts',(-0.180072959150898,0.037012513779585,
0.533335922330097));
#31358=CARTESIAN_POINT('Ctrl Pts',(-0.128788747144402,-0.131185576198834,
0.544447087378641));
#31359=CARTESIAN_POINT('Ctrl Pts',(0.0403262995152723,-0.179359935217008,
0.555558252427184));
#31360=CARTESIAN_POINT('Ctrl Pts',(0.172546185411942,-0.0634350903950841,
0.566669417475728));
#31361=CARTESIAN_POINT('Ctrl Pts',(0.146900873501267,0.11052750860401,0.577780582524271));
#31362=CARTESIAN_POINT('Ctrl Pts',(-0.013146340126236,0.183366765077345,
0.588891747572816));
#31363=CARTESIAN_POINT('Ctrl Pts',(-0.161165762009075,0.0884409065403499,
0.600002912621358));
#31364=CARTESIAN_POINT('Ctrl Pts',(-0.16173211305994,-0.087400917608522,
0.611114077669903));
#31365=CARTESIAN_POINT('Ctrl Pts',(-0.0143272298638598,-0.183278278249422,
0.622225242718446));
#31366=CARTESIAN_POINT('Ctrl Pts',(0.146185859526926,-0.111471481859797,
0.63333640776699));
#31367=CARTESIAN_POINT('Ctrl Pts',(0.172951224644592,0.0623223129190563,
0.644447572815534));
#31368=CARTESIAN_POINT('Ctrl Pts',(0.0414808152398764,0.179096450999678,
0.655558737864077));
#31369=CARTESIAN_POINT('Ctrl Pts',(-0.127941039381778,0.1320124510626,0.666669902912621));
#31370=CARTESIAN_POINT('Ctrl Pts',(-0.180307640411694,-0.0358518005518811,
0.677781067961165));
#31371=CARTESIAN_POINT('Ctrl Pts',(-0.0677079673289082,-0.170914680334463,
0.68889223300971));
#31372=CARTESIAN_POINT('Ctrl Pts',(0.106838781720774,-0.149605051766532,
0.700003398058251));
#31373=CARTESIAN_POINT('Ctrl Pts',(0.183637062036826,0.00858057341481814,
0.711114563106797));
#31374=CARTESIAN_POINT('Ctrl Pts',(0.0924229284360449,0.1589156980696,0.722225728155339));
#31375=CARTESIAN_POINT('Ctrl Pts',(-0.0833503847528551,0.163856370505402,
0.733336893203883));
#31376=CARTESIAN_POINT('Ctrl Pts',(-0.182865130156443,0.0188822924059537,
0.744448058252428));
#31377=CARTESIAN_POINT('Ctrl Pts',(-0.115073714167466,-0.143367489694622,
0.75555922330097));
#31378=CARTESIAN_POINT('Ctrl Pts',(0.0580004387659595,-0.174448118065669,
0.766670388349515));
#31379=CARTESIAN_POINT('Ctrl Pts',(0.17800908511122,-0.0459234407622611,
0.777781553398057));
#31380=CARTESIAN_POINT('Ctrl Pts',(0.135154441460109,0.124617309179735,
0.788892718446602));
#31381=CARTESIAN_POINT('Ctrl Pts',(-0.0313551099181417,0.181143738163968,
0.800003883495145));
#31382=CARTESIAN_POINT('Ctrl Pts',(-0.169177381899564,0.0719389341505889,
0.81111504854369));
#31383=CARTESIAN_POINT('Ctrl Pts',(-0.152216626984007,-0.103083923397808,
0.822226213592232));
#31384=CARTESIAN_POINT('Ctrl Pts',(0.00400949547363229,-0.183793690702293,
0.833337378640777));
#31385=CARTESIAN_POINT('Ctrl Pts',(0.156567267939011,-0.0963477420579929,
0.844448543689319));
#31386=CARTESIAN_POINT('Ctrl Pts',(0.165879203582308,0.0792482593671729,
0.855559708737864));
#31387=CARTESIAN_POINT('Ctrl Pts',(0.0234256671005791,0.182338791618694,
0.866670873786407));
#31388=CARTESIAN_POINT('Ctrl Pts',(-0.140460377720211,0.118604717671243,
0.877782038834952));
#31389=CARTESIAN_POINT('Ctrl Pts',(-0.175837031067501,-0.0536426631484242,
0.888893203883495));
#31390=CARTESIAN_POINT('Ctrl Pts',(-0.0503376402892206,-0.17681153483915,
0.900004368932038));
#31391=CARTESIAN_POINT('Ctrl Pts',(0.12121644264892,-0.138212772940753,
0.911115533980582));
#31392=CARTESIAN_POINT('Ctrl Pts',(0.181867711471885,0.026839009932345,
0.922226699029127));
#31393=CARTESIAN_POINT('Ctrl Pts',(0.0761253709552246,0.167335367481701,
0.933337864077668));
#31394=CARTESIAN_POINT('Ctrl Pts',(-0.099265255914171,0.154733978795034,
0.944449029126215));
#31395=CARTESIAN_POINT('Ctrl Pts',(-0.18383655777075,0.000564071579882353,
0.955560194174756));
#31396=CARTESIAN_POINT('Ctrl Pts',(-0.100212911067809,-0.154121939161292,
0.966671359223301));
#31397=CARTESIAN_POINT('Ctrl Pts',(0.0750970673805211,-0.167799333720618,
0.977782524271844));
#31398=CARTESIAN_POINT('Ctrl Pts',(0.181699613594968,-0.0279545920640164,
0.988893689320389));
#31399=CARTESIAN_POINT('Ctrl Pts',(0.122062258834496,0.137466418983892,
1.00000485436893));
#31400=CARTESIAN_POINT('Ctrl Pts',(-0.0492515922639386,0.177116921324136,
1.01111601941748));
#31401=CARTESIAN_POINT('Ctrl Pts',(-0.175504715049764,0.0547210291375423,
1.02222718446602));
#31402=CARTESIAN_POINT('Ctrl Pts',(-0.14118522196555,-0.1177412066494,1.03333834951456));
#31403=CARTESIAN_POINT('Ctrl Pts',(0.0223056668548975,-0.182477852394609,
1.04444951456311));
#31404=CARTESIAN_POINT('Ctrl Pts',(0.165390974917898,-0.0802670846854376,
1.05556067961165));
#31405=CARTESIAN_POINT('Ctrl Pts',(0.157153269033781,0.0953897085409752,
1.06667184466019));
#31406=CARTESIAN_POINT('Ctrl Pts',(0.00514163720288116,0.183756944970195,
1.07778300970874));
#31407=CARTESIAN_POINT('Ctrl Pts',(-0.151589489028199,0.104032592396117,
1.08889417475728));
#31408=CARTESIAN_POINT('Ctrl Pts',(-0.169599832986023,-0.0709309104380943,
1.10000533980583));
#31409=CARTESIAN_POINT('Ctrl Pts',(-0.0324962964057439,-0.180887727526569,
1.11111650485437));
#31410=CARTESIAN_POINT('Ctrl Pts',(0.134445241673909,-0.125560970886474,
1.12222766990291));
#31411=CARTESIAN_POINT('Ctrl Pts',(0.178171768593789,0.0450698535437549,
1.13333883495146));
#31412=CARTESIAN_POINT('Ctrl Pts',(0.0989503531151977,0.130685679928735,
1.14074627831715));
#31413=CARTESIAN_POINT('Ctrl Pts',(0.0499806597877626,0.147301514408983,
1.14445));
#31414=CARTESIAN_POINT('',(0.0903606778650206,-0.126612599672284,0.));
#31415=CARTESIAN_POINT('Ctrl Pts',(0.0903606778650208,-0.126612599672284,
-2.77555756156289E-16));
#31416=CARTESIAN_POINT('Ctrl Pts',(0.132452439122316,-0.0965726187415828,
0.00370372168284762));
#31417=CARTESIAN_POINT('Ctrl Pts',(0.183597970935092,0.00826171234133487,
0.0111111650485434));
#31418=CARTESIAN_POINT('Ctrl Pts',(0.0924933321163406,0.159015923519395,
0.0222223300970871));
#31419=CARTESIAN_POINT('Ctrl Pts',(-0.0833119343177651,0.163815447531815,
0.0333334951456308));
#31420=CARTESIAN_POINT('Ctrl Pts',(-0.15310616378989,0.0622578531632503,
0.0411241775931451));
#31421=CARTESIAN_POINT('Ctrl Pts',(-0.155772922446558,0.00543356393242454,
0.0452111383578116));
#31422=CARTESIAN_POINT('Ctrl Pts',(-0.155735926886437,0.000101346774827265,
0.0455943774396301));
#31423=CARTESIAN_POINT('Ctrl Pts',(0.0863567639152676,0.175641488315944,
2.2659825404947E-17));
#31424=CARTESIAN_POINT('Ctrl Pts',(0.0902605506355985,0.173244147111074,
2.45989142876686E-17));
#31425=CARTESIAN_POINT('Ctrl Pts',(0.0940681517855526,0.170703362163956,
1.50959816364938E-17));
#31426=CARTESIAN_POINT('Ctrl Pts',(0.0977705169885396,0.168018661523996,
1.10588621593521E-17));
#31427=CARTESIAN_POINT('Ctrl Pts',(0.104919852250204,0.162834455239647,
2.72100915479622E-18));
#31428=CARTESIAN_POINT('Ctrl Pts',(0.111677400716997,0.157113958337607,
-2.16691070983975E-17));
#31429=CARTESIAN_POINT('Ctrl Pts',(0.118012246833275,0.150919901422416,
-3.33934269125535E-17));
#31430=CARTESIAN_POINT('Ctrl Pts',(0.122832506482077,0.146206769948873,
-4.2314601108814E-17));
#31431=CARTESIAN_POINT('Ctrl Pts',(0.127411584310215,0.141213843322959,
-4.34283416288416E-17));
#31432=CARTESIAN_POINT('Ctrl Pts',(0.131710542479305,0.135995360136636,
-4.0766001685455E-17));
#31433=CARTESIAN_POINT('Ctrl Pts',(0.136227531634889,0.130512210258439,
-3.79686353981478E-17));
#31434=CARTESIAN_POINT('Ctrl Pts',(0.140440157604184,0.124776412163605,
1.15313389293564E-17));
#31435=CARTESIAN_POINT('Ctrl Pts',(0.144331170139148,0.11882042578862,3.72965547335014E-17));
#31436=CARTESIAN_POINT('Ctrl Pts',(0.147802837134673,0.113506333084464,
6.02849796064744E-17));
#31437=CARTESIAN_POINT('Ctrl Pts',(0.15101843405387,0.108016870008689,-1.53625880027527E-18));
#31438=CARTESIAN_POINT('Ctrl Pts',(0.153962315598392,0.102374391558266,
-8.67361737988404E-18));
#31439=CARTESIAN_POINT('Ctrl Pts',(0.15571005357274,0.0990245373918854,
-1.29109592829026E-17));
#31440=CARTESIAN_POINT('Ctrl Pts',(0.157357576324963,0.0956291376942575,
-3.44593994380303E-18));
#31441=CARTESIAN_POINT('Ctrl Pts',(0.158902506880511,0.0921936740973187,
-6.07153216591882E-18));
#31442=CARTESIAN_POINT('Ctrl Pts',(0.163908283820673,0.0810623229886477,
-1.45787941606636E-17));
#31443=CARTESIAN_POINT('Ctrl Pts',(0.167841697827597,0.0695089356622268,
-9.75260753403157E-18));
#31444=CARTESIAN_POINT('Ctrl Pts',(0.170598119604662,0.0576980955231356,
-5.20417042793042E-18));
#31445=CARTESIAN_POINT('Ctrl Pts',(0.171984491688748,0.0517577059954232,
-2.91648489207139E-18));
#31446=CARTESIAN_POINT('Ctrl Pts',(0.173072324320188,0.0457521241966622,
1.08654590748341E-17));
#31447=CARTESIAN_POINT('Ctrl Pts',(0.173843127025583,0.0397030009933723,
1.73472347597681E-17));
#31448=CARTESIAN_POINT('Ctrl Pts',(0.174324086814962,0.0359285136940646,
2.13916853648473E-17));
#31449=CARTESIAN_POINT('Ctrl Pts',(0.17468129632341,0.0321360477424029,
-3.73379012875618E-17));
#31450=CARTESIAN_POINT('Ctrl Pts',(0.174909438673913,0.0283479136595781,
-3.46944695195361E-17));
#31451=CARTESIAN_POINT('Ctrl Pts',(0.175317247780942,0.0215765466853118,
-2.99692812919358E-17));
#31452=CARTESIAN_POINT('Ctrl Pts',(0.175315000224248,0.0148063200599795,
-5.50593613673983E-17));
#31453=CARTESIAN_POINT('Ctrl Pts',(0.174882170147482,0.00806701752180915,
-4.68375338513738E-17));
#31454=CARTESIAN_POINT('Ctrl Pts',(0.174454769721774,0.00141225638482493,
-4.0453568795602E-17));
#31455=CARTESIAN_POINT('Ctrl Pts',(0.173607423807277,-0.00521244743448051,
5.53912001912299E-18));
#31456=CARTESIAN_POINT('Ctrl Pts',(0.172357876958299,-0.0117762500451153,
6.93889390390723E-18));
#31457=CARTESIAN_POINT('Ctrl Pts',(0.171266545977134,-0.0175089531839406,
8.16143038450564E-18));
#31458=CARTESIAN_POINT('Ctrl Pts',(0.169868307866471,-0.0231952127882146,
5.24172218001205E-19));
#31459=CARTESIAN_POINT('Ctrl Pts',(0.168172344307035,-0.0288124942050995,
-3.46944695195361E-18));
#31460=CARTESIAN_POINT('Ctrl Pts',(0.167269600009596,-0.0318025164482014,
-5.59521015704244E-18));
#31461=CARTESIAN_POINT('Ctrl Pts',(0.166282932031305,-0.0347708579305845,
-1.1797187803688E-17));
#31462=CARTESIAN_POINT('Ctrl Pts',(0.165217237950495,-0.0377059593473793,
-8.67361737988404E-18));
#31463=CARTESIAN_POINT('Ctrl Pts',(0.161836480623691,-0.047017135789496,
1.23544919580411E-18));
#31464=CARTESIAN_POINT('Ctrl Pts',(0.157654897120342,-0.0560198074489911,
-1.7088045241211E-17));
#31465=CARTESIAN_POINT('Ctrl Pts',(0.152731837788828,-0.0646106508942882,
1.38777878078145E-17));
#31466=CARTESIAN_POINT('Ctrl Pts',(0.14995806869425,-0.0694509370741418,
3.13246770113308E-17));
#31467=CARTESIAN_POINT('Ctrl Pts',(0.146948492244732,-0.074160201986225,
-2.50126624213863E-18));
#31468=CARTESIAN_POINT('Ctrl Pts',(0.143711118647294,-0.0787168991005189,
3.46944695195361E-18));
#31469=CARTESIAN_POINT('Ctrl Pts',(0.141667380230334,-0.0815935201226661,
7.2387295398745E-18));
#31470=CARTESIAN_POINT('Ctrl Pts',(0.139532823645962,-0.0844092886780934,
1.73900611772481E-17));
#31471=CARTESIAN_POINT('Ctrl Pts',(0.137309196652862,-0.08715819230643,
2.08166817117217E-17));
#31472=CARTESIAN_POINT('Ctrl Pts',(0.135173374337891,-0.0897985495827733,
2.41079947894884E-17));
#31473=CARTESIAN_POINT('Ctrl Pts',(0.132961417486925,-0.0923697150592745,
-3.29131307776674E-18));
#31474=CARTESIAN_POINT('Ctrl Pts',(0.130676581353388,-0.0948665968574491,
0.));
#31475=CARTESIAN_POINT('Ctrl Pts',(0.123427275316167,-0.10278867933332,
1.04426463739872E-17));
#31476=CARTESIAN_POINT('Ctrl Pts',(0.115443266551879,-0.109969536302748,
2.37276977285196E-17));
#31477=CARTESIAN_POINT('Ctrl Pts',(0.106786977446893,-0.116251471062968,
2.77555756156289E-17));
#31478=CARTESIAN_POINT('Ctrl Pts',(0.101553949468808,-0.120049119218897,
3.01905679570255E-17));
#31479=CARTESIAN_POINT('Ctrl Pts',(0.0960747579407472,-0.123517461158967,
2.18989005301202E-17));
#31480=CARTESIAN_POINT('Ctrl Pts',(0.0903606778650241,-0.126612599672281,
2.08166817117217E-17));
#31481=CARTESIAN_POINT('Ctrl Pts',(0.188079991776263,-0.0516378774142081,
1.1046));
#31482=CARTESIAN_POINT('Ctrl Pts',(0.179754570390634,-0.0821182550519846,
1.1028067538919));
#31483=CARTESIAN_POINT('Ctrl Pts',(0.164446793279769,-0.110682480125595,
1.1010135077838));
#31484=CARTESIAN_POINT('Ctrl Pts',(0.143091597726206,-0.133587557506818,
1.09922026167571));
#31485=CARTESIAN_POINT('Ctrl Pts',(0.0989851583166799,-0.180895080641009,
1.09551653999286));
#31486=CARTESIAN_POINT('Ctrl Pts',(0.0290818548970629,-0.204062011418838,
1.09181281831001));
#31487=CARTESIAN_POINT('Ctrl Pts',(-0.0345744266721549,-0.19262440956347,
1.08810909662716));
#31488=CARTESIAN_POINT('Ctrl Pts',(-0.0982307082413709,-0.181186807708102,
1.08440537494431));
#31489=CARTESIAN_POINT('Ctrl Pts',(-0.155639967960188,-0.135144673219537,
1.08070165326147));
#31490=CARTESIAN_POINT('Ctrl Pts',(-0.180573868997825,-0.0754924386616321,
1.07699793157862));
#31491=CARTESIAN_POINT('Ctrl Pts',(-0.190472245868201,-0.0518114150655666,
1.07552761078989));
#31492=CARTESIAN_POINT('Ctrl Pts',(-0.195252608806662,-0.0259854826956367,
1.07405729000116));
#31493=CARTESIAN_POINT('Ctrl Pts',(-0.195129684289216,-0.000113636086278679,
1.07258696921242));
#31494=CARTESIAN_POINT('Origin',(0.,0.,-0.129405622560369));
#31495=CARTESIAN_POINT('',(-0.0903606778650173,-0.126612599672286,0.));
#31496=CARTESIAN_POINT('Ctrl Pts',(-0.0905549614304886,-0.126792015305981,
1.24276674021151E-16));
#31497=CARTESIAN_POINT('Ctrl Pts',(-0.0513706458239086,-0.154472437079514,
0.00344950590738082));
#31498=CARTESIAN_POINT('Ctrl Pts',(0.0587535178885047,-0.172169358136003,
0.0106052258091336));
#31499=CARTESIAN_POINT('Ctrl Pts',(0.177508460417327,-0.0479721809770191,
0.0214671597052585));
#31500=CARTESIAN_POINT('Ctrl Pts',(0.13650560094313,0.123222299189869,0.0325858016883748));
#31501=CARTESIAN_POINT('Ctrl Pts',(-0.0295638381403906,0.181478253869214,
0.043704443671491));
#31502=CARTESIAN_POINT('Ctrl Pts',(-0.141307745535963,0.0946781319192958,
0.0526443839621562));
#31503=CARTESIAN_POINT('Ctrl Pts',(-0.155414936746312,0.0214718667413076,
0.0578781102584494));
#31504=CARTESIAN_POINT('Ctrl Pts',(-0.155326046963413,7.29270061605551E-5,
0.0594056225603705));
#31505=CARTESIAN_POINT('Origin',(0.,0.,0.));
#31506=CARTESIAN_POINT('Ctrl Pts',(-0.0685825729128748,0.139614588036674,
-0.0230074082272066));
#31507=CARTESIAN_POINT('Ctrl Pts',(-0.115028016933624,0.116799292759742,
-0.0193011942328345));
#31508=CARTESIAN_POINT('Ctrl Pts',(-0.182555218707277,0.0215691441263552,
-0.0118887662440903));
#31509=CARTESIAN_POINT('Ctrl Pts',(-0.116942936218886,-0.142059634545264,
-0.000770124260974049));
#31510=CARTESIAN_POINT('Ctrl Pts',(0.0559468948314244,-0.175104601534012,
0.0103485177221422));
#31511=CARTESIAN_POINT('Ctrl Pts',(0.177508460417327,-0.0479721809770191,
0.0214671597052585));
#31512=CARTESIAN_POINT('Ctrl Pts',(0.13650560094313,0.123222299189869,0.0325858016883748));
#31513=CARTESIAN_POINT('Ctrl Pts',(-0.0295638381403906,0.181478253869214,
0.043704443671491));
#31514=CARTESIAN_POINT('Ctrl Pts',(-0.168540213790592,0.0735245708832444,
0.0548230856546073));
#31515=CARTESIAN_POINT('Ctrl Pts',(-0.153132379752993,-0.101797781965797,
0.0659417276377235));
#31516=CARTESIAN_POINT('Ctrl Pts',(0.00255447675030308,-0.183860034663711,
0.0770603696208398));
#31517=CARTESIAN_POINT('Ctrl Pts',(0.155899683301632,-0.0975032021788082,
0.0881790116039561));
#31518=CARTESIAN_POINT('Ctrl Pts',(0.166434877052597,0.0781732535368643,
0.0992976535870723));
#31519=CARTESIAN_POINT('Ctrl Pts',(0.0245080507541896,0.182238325373942,
0.110416295570189));
#31520=CARTESIAN_POINT('Ctrl Pts',(-0.139868975820189,0.119365863723167,
0.121534937553305));
#31521=CARTESIAN_POINT('Ctrl Pts',(-0.176120077222934,-0.0528512641939849,
0.132653579536421));
#31522=CARTESIAN_POINT('Ctrl Pts',(-0.0510374815939226,-0.176654153931159,
0.143772221519537));
#31523=CARTESIAN_POINT('Ctrl Pts',(0.120797626960931,-0.138634273102519,
0.154890863502654));
#31524=CARTESIAN_POINT('Ctrl Pts',(0.181976886629041,0.0263806680570579,
0.16600950548577));
#31525=CARTESIAN_POINT('Ctrl Pts',(0.0764574137846417,0.167229745635935,
0.177128147468886));
#31526=CARTESIAN_POINT('Ctrl Pts',(-0.0991003621173195,0.154889135395602,
0.188246789452002));
#31527=CARTESIAN_POINT('Ctrl Pts',(-0.183877909581896,0.000663349951290586,
0.199365431435119));
#31528=CARTESIAN_POINT('Ctrl Pts',(-0.100215313155719,-0.154170088892816,
0.210484073418235));
#31529=CARTESIAN_POINT('Ctrl Pts',(0.0752488571272716,-0.167777039880966,
0.221602715401351));
#31530=CARTESIAN_POINT('Ctrl Pts',(0.181781810074028,-0.0276929424335053,
0.232721357384467));
#31531=CARTESIAN_POINT('Ctrl Pts',(0.121794738393109,0.137759091140133,
0.243839999367584));
#31532=CARTESIAN_POINT('Ctrl Pts',(-0.0497615974795104,0.177017821004958,
0.2549586413507));
#31533=CARTESIAN_POINT('Ctrl Pts',(-0.175734151264734,0.0541205469518692,
0.266077283333817));
#31534=CARTESIAN_POINT('Ctrl Pts',(-0.140726598433086,-0.11835349598584,
0.277195925316932));
#31535=CARTESIAN_POINT('Ctrl Pts',(0.0231926238140432,-0.182410602009977,
0.288314567300049));
#31536=CARTESIAN_POINT('Ctrl Pts',(0.165866396469461,-0.0793716828903688,
0.299433209283165));
#31537=CARTESIAN_POINT('Ctrl Pts',(0.156599354026699,0.096375141196464,
0.310551851266282));
#31538=CARTESIAN_POINT('Ctrl Pts',(0.00388050940998321,0.183838154825996,
0.321670493249398));
#31539=CARTESIAN_POINT('Ctrl Pts',(-0.152393050178991,0.102897443019027,
0.332789135232514));
#31540=CARTESIAN_POINT('Ctrl Pts',(-0.169067964401488,-0.0723017906820314,
0.34390777721563));
#31541=CARTESIAN_POINT('Ctrl Pts',(-0.0308692884081366,-0.181269447386996,
0.355026419198746));
#31542=CARTESIAN_POINT('Ctrl Pts',(0.135606994996762,-0.124186426112907,
0.366145061181863));
#31543=CARTESIAN_POINT('Ctrl Pts',(0.177861387826841,0.0466567491694538,
0.377263703164979));
#31544=CARTESIAN_POINT('Ctrl Pts',(0.0571870330903418,0.174760318061885,
0.388382345148095));
#31545=CARTESIAN_POINT('Ctrl Pts',(-0.115873124952358,0.142775853828764,
0.399500987131212));
#31546=CARTESIAN_POINT('Ctrl Pts',(-0.182788473512851,-0.0199974866820836,
0.410619629114327));
#31547=CARTESIAN_POINT('Ctrl Pts',(-0.0822616502622442,-0.164452261823584,
0.421738271097444));
#31548=CARTESIAN_POINT('Ctrl Pts',(0.0936204134582059,-0.158261630557358,
0.43285691308056));
#31549=CARTESIAN_POINT('Ctrl Pts',(0.183742116834086,-0.00709647969689106,
0.443975555063676));
#31550=CARTESIAN_POINT('Ctrl Pts',(0.10554806974386,0.150569354438759,0.455094197046793));
#31551=CARTESIAN_POINT('Ctrl Pts',(-0.0693325883166112,0.170307127625589,
0.466212839029909));
#31552=CARTESIAN_POINT('Ctrl Pts',(-0.180701587562324,0.0340361833232659,
0.477331481013025));
#31553=CARTESIAN_POINT('Ctrl Pts',(-0.126540093064824,-0.133413381524886,
0.488450122996142));
#31554=CARTESIAN_POINT('Ctrl Pts',(0.0435376164803608,-0.17865050090601,
0.499568764979258));
#31555=CARTESIAN_POINT('Ctrl Pts',(0.173732980498774,-0.0602360109052031,
0.510687406962374));
#31556=CARTESIAN_POINT('Ctrl Pts',(0.144781397169404,0.113357278356683,
0.521806048945491));
#31557=CARTESIAN_POINT('Ctrl Pts',(-0.0167962271460079,0.183110382765203,
0.532924690928607));
#31558=CARTESIAN_POINT('Ctrl Pts',(-0.162987778710162,0.0851264325217889,
0.544043332911723));
#31559=CARTESIAN_POINT('Ctrl Pts',(-0.159875453933454,-0.0908370230265797,
0.555161974894839));
#31560=CARTESIAN_POINT('Ctrl Pts',(-0.0103102773360761,-0.183589824620028,
0.566280616877956));
#31561=CARTESIAN_POINT('Ctrl Pts',(0.14869956060099,-0.108166382022474,
0.577399258861071));
#31562=CARTESIAN_POINT('Ctrl Pts',(0.171494149863546,0.0663421591850832,
0.588517900844189));
#31563=CARTESIAN_POINT('Ctrl Pts',(0.0371926577693494,0.180078404398782,
0.599636542827304));
#31564=CARTESIAN_POINT('Ctrl Pts',(-0.1311789224034,0.128855018683177,0.610755184810421));
#31565=CARTESIAN_POINT('Ctrl Pts',(-0.179384918603911,-0.0404051543769803,
0.621873826793537));
#31566=CARTESIAN_POINT('Ctrl Pts',(-0.0632665469493242,-0.172652453095426,
0.632992468776653));
#31567=CARTESIAN_POINT('Ctrl Pts',(0.110806726459172,-0.146742614445027,
0.644111110759769));
#31568=CARTESIAN_POINT('Ctrl Pts',(0.183376231205259,0.0135898253011021,
0.655229752742886));
#31569=CARTESIAN_POINT('Ctrl Pts',(0.0879651525947856,0.161473395492061,
0.666348394726001));
#31570=CARTESIAN_POINT('Ctrl Pts',(-0.0880258220622017,0.161440330069759,
0.677467036709119));
#31571=CARTESIAN_POINT('Ctrl Pts',(-0.183381324808445,0.013520918395534,
0.688585678692234));
#31572=CARTESIAN_POINT('Ctrl Pts',(-0.11075157823663,-0.146784241118916,
0.699704320675351));
#31573=CARTESIAN_POINT('Ctrl Pts',(0.0633314188332071,-0.172628667698419,
0.710822962658467));
#31574=CARTESIAN_POINT('Ctrl Pts',(0.17940008868909,-0.0403377453646542,
0.721941604641583));
#31575=CARTESIAN_POINT('Ctrl Pts',(0.131130494233742,0.128904301731096,
0.733060246624699));
#31576=CARTESIAN_POINT('Ctrl Pts',(-0.0372603218894873,0.180064416072257,
0.744178888607816));
#31577=CARTESIAN_POINT('Ctrl Pts',(-0.171519066664489,0.0662777133981789,
0.755297530590932));
#31578=CARTESIAN_POINT('Ctrl Pts',(-0.148658905212271,-0.108222250133236,
0.766416172574049));
#31579=CARTESIAN_POINT('Ctrl Pts',(0.0103792628149562,-0.18358593744105,
0.777534814557165));
#31580=CARTESIAN_POINT('Ctrl Pts',(0.159909575810308,-0.0907769413831382,
0.78865345654028));
#31581=CARTESIAN_POINT('Ctrl Pts',(0.162955779866738,0.0851876712390422,
0.799772098523398));
#31582=CARTESIAN_POINT('Ctrl Pts',(0.0167274199086701,0.183116681231986,
0.810890740506512));
#31583=CARTESIAN_POINT('Ctrl Pts',(-0.144823982381472,0.11330286690894,
0.82200938248963));
#31584=CARTESIAN_POINT('Ctrl Pts',(-0.173710333792674,-0.0603012890298399,
0.833128024472746));
#31585=CARTESIAN_POINT('Ctrl Pts',(-0.0434704832044991,-0.178666848096071,
0.844246666455862));
#31586=CARTESIAN_POINT('Ctrl Pts',(0.126590215885116,-0.133365823077974,
0.855365308438979));
#31587=CARTESIAN_POINT('Ctrl Pts',(0.18068878531032,0.0341040818691465,
0.866483950422094));
#31588=CARTESIAN_POINT('Ctrl Pts',(0.069268588294083,0.170333168137465,
0.877602592405212));
#31589=CARTESIAN_POINT('Ctrl Pts',(-0.105604640517969,0.15052968290502,
0.888721234388326));
#31590=CARTESIAN_POINT('Ctrl Pts',(-0.183739437498563,-0.00716552286239433,
0.899839876371444));
#31591=CARTESIAN_POINT('Ctrl Pts',(-0.0935609375970031,-0.15829679799695,
0.91095851835456));
#31592=CARTESIAN_POINT('Ctrl Pts',(0.0823234386500799,-0.164421340203127,
0.922077160337675));
#31593=CARTESIAN_POINT('Ctrl Pts',(0.182795976495949,-0.0199287985657338,
0.933195802320793));
#31594=CARTESIAN_POINT('Ctrl Pts',(0.115819463928053,0.142819381470141,
0.944314444303908));
#31595=CARTESIAN_POINT('Ctrl Pts',(-0.0572526917402423,0.174738822826618,
0.955433086287024));
#31596=CARTESIAN_POINT('Ctrl Pts',(-0.177878918025408,0.046589901053406,
0.966551728270142));
#31597=CARTESIAN_POINT('Ctrl Pts',(-0.135560300066214,-0.124237352171324,
0.977670370253256));
#31598=CARTESIAN_POINT('Ctrl Pts',(0.0309373610575528,-0.181257875466721,
0.988789012236375));
#31599=CARTESIAN_POINT('Ctrl Pts',(0.169095195914933,-0.0722381792257861,
0.999907654219489));
#31600=CARTESIAN_POINT('Ctrl Pts',(0.152354231364944,0.102954552944809,
1.01102629620261));
#31601=CARTESIAN_POINT('Ctrl Pts',(-0.00394931635484403,0.183836962465064,
1.02214493818572));
#31602=CARTESIAN_POINT('Ctrl Pts',(-0.156636075542215,0.0963157594965877,
1.03326358016884));
#31603=CARTESIAN_POINT('Ctrl Pts',(-0.165835572967195,-0.0794329933758677,
1.04438222215196));
#31604=CARTESIAN_POINT('Ctrl Pts',(-0.0231259578302998,-0.182421227428175,
1.05550086413507));
#31605=CARTESIAN_POINT('Ctrl Pts',(0.140774638007895,-0.11829694620695,
1.06661950611819));
#31606=CARTESIAN_POINT('Ctrl Pts',(0.175706993010233,0.0541796064983141,
1.07773814810131));
#31607=CARTESIAN_POINT('Ctrl Pts',(0.0497080432048737,0.177049779856472,
1.08885679008442));
#31608=CARTESIAN_POINT('Ctrl Pts',(-0.121871201614337,0.137688031013954,
1.09997543206754));
#31609=CARTESIAN_POINT('Ctrl Pts',(-0.181724153253684,-0.027712968875509,
1.11109407405065));
#31610=CARTESIAN_POINT('Ctrl Pts',(-0.075277483453787,-0.167898453189698,
1.12221271603377));
#31611=CARTESIAN_POINT('Ctrl Pts',(0.100462758039806,-0.153944373403644,
1.13333135801688));
#31612=CARTESIAN_POINT('Ctrl Pts',(0.155754888396286,-0.0511266487217653,
1.14074378600563));
#31613=CARTESIAN_POINT('Ctrl Pts',(0.155548765964692,0.000619602180124784,
1.14445));
#31614=CARTESIAN_POINT('Ctrl Pts',(-0.074439243930934,0.151537102412034,
-0.0153382721514711));
#31615=CARTESIAN_POINT('Ctrl Pts',(-0.124850938769699,0.126773474301532,
-0.011632058157099));
#31616=CARTESIAN_POINT('Ctrl Pts',(-0.198144687185762,0.0234110607521693,
-0.0042196301683548));
#31617=CARTESIAN_POINT('Ctrl Pts',(-0.126929384324154,-0.154190945884872,
0.00689901181476148));
#31618=CARTESIAN_POINT('Ctrl Pts',(0.0607245306591998,-0.190057817801302,
0.0180176537978778));
#31619=CARTESIAN_POINT('Ctrl Pts',(0.192666956394248,-0.0520688088821623,
0.029136295780994));
#31620=CARTESIAN_POINT('Ctrl Pts',(0.148162620545796,0.133744979191402,
0.0402549377641103));
#31621=CARTESIAN_POINT('Ctrl Pts',(-0.0320884689126903,0.19697575395855,
0.0513735797472264));
#31622=CARTESIAN_POINT('Ctrl Pts',(-0.182932858212653,0.0798032683003624,
0.0624922217303428));
#31623=CARTESIAN_POINT('Ctrl Pts',(-0.166209258212561,-0.110490895887015,
0.0736108637134591));
#31624=CARTESIAN_POINT('Ctrl Pts',(0.00277261860929502,-0.199560929084259,
0.0847295056965753));
#31625=CARTESIAN_POINT('Ctrl Pts',(0.169212878157669,-0.10582957656395,
0.0958481476796916));
#31626=CARTESIAN_POINT('Ctrl Pts',(0.180647734334385,0.0848489294255244,
0.106966789662808));
#31627=CARTESIAN_POINT('Ctrl Pts',(0.0266009379770665,0.197800732458805,
0.118085431645924));
#31628=CARTESIAN_POINT('Ctrl Pts',(-0.151813213871049,0.12955921992025,
0.129204073629041));
#31629=CARTESIAN_POINT('Ctrl Pts',(-0.191160010957712,-0.0573645458357494,
0.140322715612156));
#31630=CARTESIAN_POINT('Ctrl Pts',(-0.0553958736254638,-0.191739695630841,
0.151441357595273));
#31631=CARTESIAN_POINT('Ctrl Pts',(0.131113249878304,-0.150473072594935,
0.162559999578389));
#31632=CARTESIAN_POINT('Ctrl Pts',(0.19751696791516,0.0286334691329668,
0.173678641561505));
#31633=CARTESIAN_POINT('Ctrl Pts',(0.0829865639814035,0.181510481441338,
0.184797283544622));
#31634=CARTESIAN_POINT('Ctrl Pts',(-0.107563127424026,0.168116033596642,
0.195915925527738));
#31635=CARTESIAN_POINT('Ctrl Pts',(-0.199580330447296,0.000719997322039096,
0.207034567510854));
#31636=CARTESIAN_POINT('Ctrl Pts',(-0.108773290717609,-0.167335583465575,
0.218153209493971));
#31637=CARTESIAN_POINT('Ctrl Pts',(0.0816748015321165,-0.182104512374819,
0.229271851477087));
#31638=CARTESIAN_POINT('Ctrl Pts',(0.197305232620797,-0.0300578063700233,
0.240390493460203));
#31639=CARTESIAN_POINT('Ctrl Pts',(0.132195510545613,0.149523153675082,
0.251509135443319));
#31640=CARTESIAN_POINT('Ctrl Pts',(-0.054011034229875,0.192134418384253,
0.262627777426435));
#31641=CARTESIAN_POINT('Ctrl Pts',(-0.190741128502276,0.0587422201459823,
0.273746419409552));
#31642=CARTESIAN_POINT('Ctrl Pts',(-0.152744073944838,-0.128460400121777,
0.284865061392668));
#31643=CARTESIAN_POINT('Ctrl Pts',(0.0251731789602741,-0.19798772081443,
0.295983703375785));
#31644=CARTESIAN_POINT('Ctrl Pts',(0.180030707836241,-0.0861496997406464,
0.3071023453589));
#31645=CARTESIAN_POINT('Ctrl Pts',(0.169972297898904,0.104605183790867,
0.318220987342017));
#31646=CARTESIAN_POINT('Ctrl Pts',(0.00421188903066005,0.199537180797957,
0.329339629325133));
#31647=CARTESIAN_POINT('Ctrl Pts',(-0.165406792919015,0.111684463493277,
0.34045827130825));
#31648=CARTESIAN_POINT('Ctrl Pts',(-0.183505676565636,-0.0784760676748057,
0.351576913291366));
#31649=CARTESIAN_POINT('Ctrl Pts',(-0.0335053992900935,-0.196749116257395,
0.362695555274482));
#31650=CARTESIAN_POINT('Ctrl Pts',(0.147187277329603,-0.134791438607496,
0.373814197257599));
#31651=CARTESIAN_POINT('Ctrl Pts',(0.193050022360002,0.0506410445822938,
0.384932839240714));
#31652=CARTESIAN_POINT('Ctrl Pts',(0.0620705716495424,0.189684133929807,
0.396051481223831));
#31653=CARTESIAN_POINT('Ctrl Pts',(-0.125768215554202,0.154968327363698,
0.407170123206947));
#31654=CARTESIAN_POINT('Ctrl Pts',(-0.19839786099702,-0.0217051901949521,
0.418288765190064));
#31655=CARTESIAN_POINT('Ctrl Pts',(-0.0892864584974339,-0.178495811879663,
0.429407407173179));
#31656=CARTESIAN_POINT('Ctrl Pts',(0.101615213578872,-0.171776526041577,
0.440526049156296));
#31657=CARTESIAN_POINT('Ctrl Pts',(0.199432941554622,-0.00770249001709277,
0.451644691139412));
#31658=CARTESIAN_POINT('Ctrl Pts',(0.114561442891388,0.16342736102696,0.462763333122529));
#31659=CARTESIAN_POINT('Ctrl Pts',(-0.0752533075803338,0.184850659257176,
0.473881975105645));
#31660=CARTESIAN_POINT('Ctrl Pts',(-0.196132763527948,0.0369427340688636,
0.485000617088761));
#31661=CARTESIAN_POINT('Ctrl Pts',(-0.13734609908354,-0.144806338245697,
0.496119259071877));
#31662=CARTESIAN_POINT('Ctrl Pts',(0.0472555507281729,-0.19390652246629,
0.507237901054994));
#31663=CARTESIAN_POINT('Ctrl Pts',(0.188569065943703,-0.0653799196903168,
0.51835654303811));
#31664=CARTESIAN_POINT('Ctrl Pts',(0.157145135896933,0.123037525956625,
0.529475185021226));
#31665=CARTESIAN_POINT('Ctrl Pts',(-0.0182305561972616,0.198747259981946,
0.540593827004342));
#31666=CARTESIAN_POINT('Ctrl Pts',(-0.176906267902489,0.0923958814363803,
0.551712468987459));
#31667=CARTESIAN_POINT('Ctrl Pts',(-0.173528163328608,-0.0985941329968107,
0.562831110970574));
#31668=CARTESIAN_POINT('Ctrl Pts',(-0.0111907328205795,-0.199267644208816,
0.573949752953692));
#31669=CARTESIAN_POINT('Ctrl Pts',(0.161397894448518,-0.117403348321834,
0.585068394936807));
#31670=CARTESIAN_POINT('Ctrl Pts',(0.186139048335769,0.0720075080408093,
0.596187036919923));
#31671=CARTESIAN_POINT('Ctrl Pts',(0.0403687585131819,0.19545636307293,
0.60730567890304));
#31672=CARTESIAN_POINT('Ctrl Pts',(-0.142381065460884,0.139858709874703,
0.618424320886156));
#31673=CARTESIAN_POINT('Ctrl Pts',(-0.194703656429618,-0.0438555891823412,
0.629542962869273));
#31674=CARTESIAN_POINT('Ctrl Pts',(-0.0686692511086116,-0.187396265922711,
0.640661604852388));
#31675=CARTESIAN_POINT('Ctrl Pts',(0.120269167366484,-0.159273833100625,
0.651780246835506));
#31676=CARTESIAN_POINT('Ctrl Pts',(0.199035810790665,0.0147503407586138,
0.662898888818621));
#31677=CARTESIAN_POINT('Ctrl Pts',(0.0954770165847204,0.175262562555938,
0.674017530801738));
#31678=CARTESIAN_POINT('Ctrl Pts',(-0.09554286697633,0.17522667348191,0.685136172784854));
#31679=CARTESIAN_POINT('Ctrl Pts',(-0.199041339366714,0.0146755494853507,
0.69625481476797));
#31680=CARTESIAN_POINT('Ctrl Pts',(-0.120209309711463,-0.159319014522084,
0.707373456751086));
#31681=CARTESIAN_POINT('Ctrl Pts',(0.0687396627858533,-0.187370449350155,
0.718492098734203));
#31682=CARTESIAN_POINT('Ctrl Pts',(0.194720121977979,-0.0437824237162718,
0.729610740717318));
#31683=CARTESIAN_POINT('Ctrl Pts',(0.142328501723757,0.139912201493195,
0.740729382700435));
#31684=CARTESIAN_POINT('Ctrl Pts',(-0.0404422008722263,0.195441180200575,
0.751848024683551));
#31685=CARTESIAN_POINT('Ctrl Pts',(-0.186166092929526,0.0719375588474842,
0.762966666666667));
#31686=CARTESIAN_POINT('Ctrl Pts',(-0.161353767256008,-0.117463987340584,
0.774085308649784));
#31687=CARTESIAN_POINT('Ctrl Pts',(0.0112656093769942,-0.199263425080664,
0.7852039506329));
#31688=CARTESIAN_POINT('Ctrl Pts',(0.173565199074082,-0.0985289206269375,
0.796322592616017));
#31689=CARTESIAN_POINT('Ctrl Pts',(0.176871536488809,0.0924623496894334,
0.807441234599133));
#31690=CARTESIAN_POINT('Ctrl Pts',(0.0181558731034875,0.198754096312013,
0.818559876582249));
#31691=CARTESIAN_POINT('Ctrl Pts',(-0.157191357711808,0.122978467993954,
0.829678518565365));
#31692=CARTESIAN_POINT('Ctrl Pts',(-0.188544485301595,-0.06545077229961,
0.840797160548482));
#31693=CARTESIAN_POINT('Ctrl Pts',(-0.0471826845453332,-0.193924265639472,
0.851915802531597));
#31694=CARTESIAN_POINT('Ctrl Pts',(0.137400502187529,-0.144754718502077,
0.863034444514714));
#31695=CARTESIAN_POINT('Ctrl Pts',(0.196118868016023,0.0370164308726493,
0.87415308649783));
#31696=CARTESIAN_POINT('Ctrl Pts',(0.0751838422178375,0.184878923522181,
0.885271728480947));
#31697=CARTESIAN_POINT('Ctrl Pts',(-0.114622844578058,0.163384301706618,
0.896390370464062));
#31698=CARTESIAN_POINT('Ctrl Pts',(-0.199430033414812,-0.0077774291863319,
0.90750901244718));
#31699=CARTESIAN_POINT('Ctrl Pts',(-0.101550658722561,-0.171814696636568,
0.918627654430294));
#31700=CARTESIAN_POINT('Ctrl Pts',(0.0893535233606871,-0.178462249679383,
0.929746296413413));
#31701=CARTESIAN_POINT('Ctrl Pts',(0.198406004704164,-0.0216306363946107,
0.940864938396527));
#31702=CARTESIAN_POINT('Ctrl Pts',(0.12570997209806,0.155015572087487,0.951983580379645));
#31703=CARTESIAN_POINT('Ctrl Pts',(-0.0621418372793996,0.18966080308943,
0.963102222362759));
#31704=CARTESIAN_POINT('Ctrl Pts',(-0.193069049565776,0.050568487910749,
0.974220864345877));
#31705=CARTESIAN_POINT('Ctrl Pts',(-0.147136594843111,-0.134846713542859,
0.985339506328992));
#31706=CARTESIAN_POINT('Ctrl Pts',(0.0335792850651442,-0.196736556142493,
0.99645814831211));
#31707=CARTESIAN_POINT('Ctrl Pts',(0.183535233538869,-0.0784070240605622,
1.00757679029522));
#31708=CARTESIAN_POINT('Ctrl Pts',(0.165364659137136,0.111746450372967,
1.01869543227834));
#31709=CARTESIAN_POINT('Ctrl Pts',(-0.00428657180698079,0.199535886614283,
1.02981407426146));
#31710=CARTESIAN_POINT('Ctrl Pts',(-0.170012155281541,0.104540731136874,
1.04093271624457));
#31711=CARTESIAN_POINT('Ctrl Pts',(-0.179997252133044,-0.0862162458906591,
1.05205135822769));
#31712=CARTESIAN_POINT('Ctrl Pts',(-0.0251008199743871,-0.197999253599851,
1.06317000021081));
#31713=CARTESIAN_POINT('Ctrl Pts',(0.152796215902707,-0.128399021223231,
1.07428864219392));
#31714=CARTESIAN_POINT('Ctrl Pts',(0.190711651044001,0.0588063231359589,
1.08540728417704));
#31715=CARTESIAN_POINT('Ctrl Pts',(0.0539529066393858,0.192169106390877,
1.09652592616015));
#31716=CARTESIAN_POINT('Ctrl Pts',(-0.132278503412967,0.149446025304978,
1.10764456814327));
#31717=CARTESIAN_POINT('Ctrl Pts',(-0.197242652143987,-0.0300795429882017,
1.11876321012639));
#31718=CARTESIAN_POINT('Ctrl Pts',(-0.0817058724297523,-0.182236293883171,
1.12988185210951));
#31719=CARTESIAN_POINT('Ctrl Pts',(0.109041866382002,-0.167090592797485,
1.14100049409262));
#31720=CARTESIAN_POINT('Ctrl Pts',(0.169055718360052,-0.0554926552610627,
1.14841292208137));
#31721=CARTESIAN_POINT('Ctrl Pts',(0.16883199391646,0.000672513670271936,
1.15211913607574));
#31722=CARTESIAN_POINT('Ctrl Pts',(-0.0802959149489932,0.163459616787394,
-0.00766913607573554));
#31723=CARTESIAN_POINT('Ctrl Pts',(-0.134673860605774,0.136747655843322,
-0.00396292208136346));
#31724=CARTESIAN_POINT('Ctrl Pts',(-0.213734155664247,0.0252529773779836,
0.00344950590738073));
#31725=CARTESIAN_POINT('Ctrl Pts',(-0.136915832429422,-0.166322257224481,
0.014568147890497));
#31726=CARTESIAN_POINT('Ctrl Pts',(0.0655021664869751,-0.205011034068591,
0.0256867898736133));
#31727=CARTESIAN_POINT('Ctrl Pts',(0.20782545237117,-0.0561654367873057,
0.0368054318567295));
#31728=CARTESIAN_POINT('Ctrl Pts',(0.159819640148463,0.144267659192936,
0.0479240738398458));
#31729=CARTESIAN_POINT('Ctrl Pts',(-0.0346130996849898,0.212473254047885,
0.0590427158229621));
#31730=CARTESIAN_POINT('Ctrl Pts',(-0.197325502634714,0.0860819657174806,
0.0701613578060782));
#31731=CARTESIAN_POINT('Ctrl Pts',(-0.179286136672128,-0.119184009808233,
0.0812799997891947));
#31732=CARTESIAN_POINT('Ctrl Pts',(0.00299076046828686,-0.215261823504807,
0.0923986417723108));
#31733=CARTESIAN_POINT('Ctrl Pts',(0.182526073013706,-0.114155950949091,
0.103517283755427));
#31734=CARTESIAN_POINT('Ctrl Pts',(0.194860591616173,0.0915246053141843,
0.114635925738543));
#31735=CARTESIAN_POINT('Ctrl Pts',(0.0286938251999433,0.213363139543668,
0.12575456772166));
#31736=CARTESIAN_POINT('Ctrl Pts',(-0.163757451921909,0.139752576117334,
0.136873209704776));
#31737=CARTESIAN_POINT('Ctrl Pts',(-0.20619994469249,-0.0618778274775138,
0.147991851687892));
#31738=CARTESIAN_POINT('Ctrl Pts',(-0.0597542656570052,-0.206825237330522,
0.159110493671008));
#31739=CARTESIAN_POINT('Ctrl Pts',(0.141428872795678,-0.162311872087351,
0.170229135654125));
#31740=CARTESIAN_POINT('Ctrl Pts',(0.213057049201279,0.0308862702088754,
0.181347777637241));
#31741=CARTESIAN_POINT('Ctrl Pts',(0.0895157141781652,0.195791217246742,
0.192466419620357));
#31742=CARTESIAN_POINT('Ctrl Pts',(-0.116025892730732,0.181342931797682,
0.203585061603473));
#31743=CARTESIAN_POINT('Ctrl Pts',(-0.215282751312695,0.000776644692787891,
0.21470370358659));
#31744=CARTESIAN_POINT('Ctrl Pts',(-0.1173312682795,-0.180501078038335,
0.225822345569706));
#31745=CARTESIAN_POINT('Ctrl Pts',(0.0881007459369614,-0.196431984868673,
0.236940987552822));
#31746=CARTESIAN_POINT('Ctrl Pts',(0.212828655167567,-0.0324226703065412,
0.248059629535939));
#31747=CARTESIAN_POINT('Ctrl Pts',(0.142596282698117,0.16128721621003,0.259178271519055));
#31748=CARTESIAN_POINT('Ctrl Pts',(-0.0582604709802392,0.207251015763547,
0.270296913502171));
#31749=CARTESIAN_POINT('Ctrl Pts',(-0.205748105739819,0.0633638933400953,
0.281415555485287));
#31750=CARTESIAN_POINT('Ctrl Pts',(-0.16476154945659,-0.138567304257714,
0.292534197468403));
#31751=CARTESIAN_POINT('Ctrl Pts',(0.0271537341065049,-0.213564839618882,
0.30365283945152));
#31752=CARTESIAN_POINT('Ctrl Pts',(0.19419501920302,-0.092927716590924,
0.314771481434636));
#31753=CARTESIAN_POINT('Ctrl Pts',(0.183345241771109,0.11283522638527,0.325890123417753));
#31754=CARTESIAN_POINT('Ctrl Pts',(0.0045432686513366,0.215236206769919,
0.337008765400868));
#31755=CARTESIAN_POINT('Ctrl Pts',(-0.178420535659039,0.120471483967528,
0.348127407383985));
#31756=CARTESIAN_POINT('Ctrl Pts',(-0.197943388729784,-0.08465034466758,
0.359246049367101));
#31757=CARTESIAN_POINT('Ctrl Pts',(-0.0361415101720502,-0.212228785127794,
0.370364691350217));
#31758=CARTESIAN_POINT('Ctrl Pts',(0.158767559662444,-0.145396451102085,
0.381483333333334));
#31759=CARTESIAN_POINT('Ctrl Pts',(0.208238656893164,0.0546253399951339,
0.39260197531645));
#31760=CARTESIAN_POINT('Ctrl Pts',(0.0669541102087431,0.204607949797729,
0.403720617299566));
#31761=CARTESIAN_POINT('Ctrl Pts',(-0.135663306156047,0.167160800898631,
0.414839259282683));
#31762=CARTESIAN_POINT('Ctrl Pts',(-0.214007248481188,-0.0234128937078206,
0.425957901265799));
#31763=CARTESIAN_POINT('Ctrl Pts',(-0.0963112667326238,-0.192539361935742,
0.437076543248915));
#31764=CARTESIAN_POINT('Ctrl Pts',(0.109610013699538,-0.185291421525797,
0.448195185232032));
#31765=CARTESIAN_POINT('Ctrl Pts',(0.215123766275159,-0.00830850033729405,
0.459313827215147));
#31766=CARTESIAN_POINT('Ctrl Pts',(0.123574816038915,0.176285367615161,
0.470432469198265));
#31767=CARTESIAN_POINT('Ctrl Pts',(-0.0811740268440561,0.199394190888763,
0.48155111118138));
#31768=CARTESIAN_POINT('Ctrl Pts',(-0.211563939493572,0.0398492848144611,
0.492669753164497));
#31769=CARTESIAN_POINT('Ctrl Pts',(-0.148152105102257,-0.156199294966507,
0.503788395147612));
#31770=CARTESIAN_POINT('Ctrl Pts',(0.0509734849759847,-0.20916254402657,
0.51490703713073));
#31771=CARTESIAN_POINT('Ctrl Pts',(0.203405151388631,-0.0705238284754304,
0.526025679113844));
#31772=CARTESIAN_POINT('Ctrl Pts',(0.169508874624462,0.132717773556567,
0.537144321096963));
#31773=CARTESIAN_POINT('Ctrl Pts',(-0.019664885248515,0.21438413719869,
0.548262963080077));
#31774=CARTESIAN_POINT('Ctrl Pts',(-0.190824757094816,0.0996653303509719,
0.559381605063195));
#31775=CARTESIAN_POINT('Ctrl Pts',(-0.187180872723762,-0.106351242967042,
0.570500247046309));
#31776=CARTESIAN_POINT('Ctrl Pts',(-0.012071188305083,-0.214945463797604,
0.581618889029427));
#31777=CARTESIAN_POINT('Ctrl Pts',(0.174096228296046,-0.126640314621194,
0.592737531012542));
#31778=CARTESIAN_POINT('Ctrl Pts',(0.200783946807991,0.0776728568965356,
0.60385617299566));
#31779=CARTESIAN_POINT('Ctrl Pts',(0.0435448592570146,0.210834321747079,
0.614974814978775));
#31780=CARTESIAN_POINT('Ctrl Pts',(-0.153583208518367,0.150862401066228,
0.626093456961893));
#31781=CARTESIAN_POINT('Ctrl Pts',(-0.210022394255324,-0.0473060239877022,
0.637212098945007));
#31782=CARTESIAN_POINT('Ctrl Pts',(-0.074071955267899,-0.202140078749996,
0.648330740928124));
#31783=CARTESIAN_POINT('Ctrl Pts',(0.129731608273796,-0.171805051756223,
0.65944938291124));
#31784=CARTESIAN_POINT('Ctrl Pts',(0.214695390376071,0.015910856216126,
0.670568024894357));
#31785=CARTESIAN_POINT('Ctrl Pts',(0.102988880574655,0.189051729619815,
0.681686666877473));
#31786=CARTESIAN_POINT('Ctrl Pts',(-0.103059911890458,0.189013016894061,
0.692805308860589));
#31787=CARTESIAN_POINT('Ctrl Pts',(-0.214701353924984,0.0158301805751674,
0.703923950843705));
#31788=CARTESIAN_POINT('Ctrl Pts',(-0.129667041186295,-0.171853787925252,
0.715042592826822));
#31789=CARTESIAN_POINT('Ctrl Pts',(0.0741479067384996,-0.20211223100189,
0.726161234809938));
#31790=CARTESIAN_POINT('Ctrl Pts',(0.210040155266868,-0.0472271020678894,
0.737279876793055));
#31791=CARTESIAN_POINT('Ctrl Pts',(0.153526509213771,0.150920101255294,
0.748398518776171));
#31792=CARTESIAN_POINT('Ctrl Pts',(-0.0436240798549652,0.210817944328893,
0.759517160759286));
#31793=CARTESIAN_POINT('Ctrl Pts',(-0.200813119194563,0.0775974042967894,
0.770635802742404));
#31794=CARTESIAN_POINT('Ctrl Pts',(-0.174048629299744,-0.126705724547931,
0.781754444725519));
#31795=CARTESIAN_POINT('Ctrl Pts',(0.0121519559390324,-0.214940912720278,
0.792873086708636));
#31796=CARTESIAN_POINT('Ctrl Pts',(0.187220822337856,-0.106280899870737,
0.803991728691751));
#31797=CARTESIAN_POINT('Ctrl Pts',(0.190787293110882,0.0997370281398245,
0.815110370674869));
#31798=CARTESIAN_POINT('Ctrl Pts',(0.0195843262983046,0.21439151139204,
0.826229012657984));
#31799=CARTESIAN_POINT('Ctrl Pts',(-0.169558733042143,0.132654069078969,
0.837347654641101));
#31800=CARTESIAN_POINT('Ctrl Pts',(-0.203378636810517,-0.0706002555693802,
0.848466296624217));
#31801=CARTESIAN_POINT('Ctrl Pts',(-0.0508948858861673,-0.209181683182873,
0.859584938607333));
#31802=CARTESIAN_POINT('Ctrl Pts',(0.148210788489943,-0.156143613926181,
0.870703580590451));
#31803=CARTESIAN_POINT('Ctrl Pts',(0.211548950721726,0.0399287798761521,
0.881822222573564));
#31804=CARTESIAN_POINT('Ctrl Pts',(0.0810990961415922,0.199424678906897,
0.892940864556684));
#31805=CARTESIAN_POINT('Ctrl Pts',(-0.123641048638147,0.176238920508216,
0.904059506539796));
#31806=CARTESIAN_POINT('Ctrl Pts',(-0.215120629331062,-0.00838933551026959,
0.915178148522916));
#31807=CARTESIAN_POINT('Ctrl Pts',(-0.109540379848118,-0.185332595276186,
0.926296790506031));
#31808=CARTESIAN_POINT('Ctrl Pts',(0.0963836080712942,-0.19250315915564,
0.937415432489146));
#31809=CARTESIAN_POINT('Ctrl Pts',(0.214016032912378,-0.0233324742234878,
0.948534074472264));
#31810=CARTESIAN_POINT('Ctrl Pts',(0.135600480268067,0.167211762704833,
0.95965271645538));
#31811=CARTESIAN_POINT('Ctrl Pts',(-0.0670309828185569,0.204582783352242,
0.970771358438496));
#31812=CARTESIAN_POINT('Ctrl Pts',(-0.208259181106143,0.0545470747680921,
0.981890000421612));
#31813=CARTESIAN_POINT('Ctrl Pts',(-0.158712889620009,-0.145456074914393,
0.993008642404728));
#31814=CARTESIAN_POINT('Ctrl Pts',(0.0362212090727357,-0.212215236818265,
1.00412728438785));
#31815=CARTESIAN_POINT('Ctrl Pts',(0.197975271162805,-0.0845758688953388,
1.01524592637096));
#31816=CARTESIAN_POINT('Ctrl Pts',(0.178375086909329,0.120538347801125,
1.02636456835408));
#31817=CARTESIAN_POINT('Ctrl Pts',(-0.00462382725911752,0.215234810763501,
1.03748321033719));
#31818=CARTESIAN_POINT('Ctrl Pts',(-0.183388235020868,0.112765702777161,
1.04860185232031));
#31819=CARTESIAN_POINT('Ctrl Pts',(-0.194158931298892,-0.0929994984054507,
1.05972049430343));
#31820=CARTESIAN_POINT('Ctrl Pts',(-0.0270756821184746,-0.213577279771527,
1.07083913628654));
#31821=CARTESIAN_POINT('Ctrl Pts',(0.164817793797518,-0.138501096239512,
1.08195777826966));
#31822=CARTESIAN_POINT('Ctrl Pts',(0.20571630907777,0.0634330397736036,
1.09307642025277));
#31823=CARTESIAN_POINT('Ctrl Pts',(0.058197770073898,0.207288432925282,
1.10419506223589));
#31824=CARTESIAN_POINT('Ctrl Pts',(-0.142685805211597,0.161204019596003,
1.11531370421901));
#31825=CARTESIAN_POINT('Ctrl Pts',(-0.212761151034289,-0.0324461171008946,
1.12643234620212));
#31826=CARTESIAN_POINT('Ctrl Pts',(-0.0881342614057178,-0.196574134576644,
1.13755098818524));
#31827=CARTESIAN_POINT('Ctrl Pts',(0.117620974724197,-0.180236812191326,
1.14866963016836));
#31828=CARTESIAN_POINT('Ctrl Pts',(0.182356548323819,-0.0598586618003602,
1.1560820581571));
#31829=CARTESIAN_POINT('Ctrl Pts',(0.182115221868229,0.000725425160419088,
1.15978827215147));
#31830=CARTESIAN_POINT('Ctrl Pts',(-0.0861525859670525,0.175382131162755,
-1.38777878078145E-17));
#31831=CARTESIAN_POINT('Ctrl Pts',(-0.144496782441849,0.146721837385112,
0.00370621399437207));
#31832=CARTESIAN_POINT('Ctrl Pts',(-0.229323624142731,0.0270948940037977,
0.0111186419831162));
#31833=CARTESIAN_POINT('Ctrl Pts',(-0.14690228053469,-0.178453568564088,
0.0222372839662325));
#31834=CARTESIAN_POINT('Ctrl Pts',(0.0702798023147504,-0.219964250335881,
0.0333559259493488));
#31835=CARTESIAN_POINT('Ctrl Pts',(0.222983948348091,-0.0602620646924488,
0.044474567932465));
#31836=CARTESIAN_POINT('Ctrl Pts',(0.171476659751129,0.154790339194469,
0.0555932099155814));
#31837=CARTESIAN_POINT('Ctrl Pts',(-0.0371377304572895,0.22797075413722,
0.0667118518986976));
#31838=CARTESIAN_POINT('Ctrl Pts',(-0.211718147056775,0.0923606631345987,
0.0778304938818138));
#31839=CARTESIAN_POINT('Ctrl Pts',(-0.192363015131696,-0.12787712372945,
0.0889491358649302));
#31840=CARTESIAN_POINT('Ctrl Pts',(0.00320890232727887,-0.230962717925356,
0.100067777848046));
#31841=CARTESIAN_POINT('Ctrl Pts',(0.195839267869742,-0.122482325334233,
0.111186419831163));
#31842=CARTESIAN_POINT('Ctrl Pts',(0.209073448897961,0.0982002812028443,
0.122305061814279));
#31843=CARTESIAN_POINT('Ctrl Pts',(0.0307867124228199,0.228925546628532,
0.133423703797395));
#31844=CARTESIAN_POINT('Ctrl Pts',(-0.175701689972769,0.149945932314417,
0.144542345780511));
#31845=CARTESIAN_POINT('Ctrl Pts',(-0.221239878427269,-0.0663911091192784,
0.155660987763628));
#31846=CARTESIAN_POINT('Ctrl Pts',(-0.0641126576885465,-0.221910779030204,
0.166779629746744));
#31847=CARTESIAN_POINT('Ctrl Pts',(0.151744495713052,-0.174150671579767,
0.17789827172986));
#31848=CARTESIAN_POINT('Ctrl Pts',(0.228597130487397,0.0331390712847842,
0.189016913712977));
#31849=CARTESIAN_POINT('Ctrl Pts',(0.0960448643749269,0.210071953052146,
0.200135555696093));
#31850=CARTESIAN_POINT('Ctrl Pts',(-0.124488658037438,0.194569829998722,
0.211254197679209));
#31851=CARTESIAN_POINT('Ctrl Pts',(-0.230985172178094,0.000833292063536468,
0.222372839662325));
#31852=CARTESIAN_POINT('Ctrl Pts',(-0.12588924584139,-0.193666572611094,
0.233491481645442));
#31853=CARTESIAN_POINT('Ctrl Pts',(0.0945266903418065,-0.210759457362527,
0.244610123628558));
#31854=CARTESIAN_POINT('Ctrl Pts',(0.228352077714336,-0.0347875342430591,
0.255728765611674));
#31855=CARTESIAN_POINT('Ctrl Pts',(0.152997054850621,0.173051278744978,
0.26684740759479));
#31856=CARTESIAN_POINT('Ctrl Pts',(-0.0625099077306038,0.222367613142842,
0.277966049577907));
#31857=CARTESIAN_POINT('Ctrl Pts',(-0.220755082977362,0.0679855665342084,
0.289084691561023));
#31858=CARTESIAN_POINT('Ctrl Pts',(-0.176779024968342,-0.148674208393651,
0.300203333544139));
#31859=CARTESIAN_POINT('Ctrl Pts',(0.0291342892527361,-0.229141958423335,
0.311321975527256));
#31860=CARTESIAN_POINT('Ctrl Pts',(0.208359330569799,-0.0997057334412016,
0.322440617510372));
#31861=CARTESIAN_POINT('Ctrl Pts',(0.196718185643314,0.121065268979674,
0.333559259493488));
#31862=CARTESIAN_POINT('Ctrl Pts',(0.00487464827201324,0.230935232741881,
0.344677901476604));
#31863=CARTESIAN_POINT('Ctrl Pts',(-0.191434278399063,0.129258504441778,
0.355796543459721));
#31864=CARTESIAN_POINT('Ctrl Pts',(-0.212381100893932,-0.0908246216603541,
0.366915185442837));
#31865=CARTESIAN_POINT('Ctrl Pts',(-0.038777621054007,-0.227708453998192,
0.378033827425954));
#31866=CARTESIAN_POINT('Ctrl Pts',(0.170347841995286,-0.156001463596674,
0.389152469409069));
#31867=CARTESIAN_POINT('Ctrl Pts',(0.223427291426326,0.058609635407974,
0.400271111392186));
#31868=CARTESIAN_POINT('Ctrl Pts',(0.0718376487679439,0.219531765665651,
0.411389753375301));
#31869=CARTESIAN_POINT('Ctrl Pts',(-0.145558396757891,0.179353274433565,
0.422508395358419));
#31870=CARTESIAN_POINT('Ctrl Pts',(-0.229616635965357,-0.0251205972206891,
0.433627037341534));
#31871=CARTESIAN_POINT('Ctrl Pts',(-0.103336074967814,-0.206582911991821,
0.444745679324651));
#31872=CARTESIAN_POINT('Ctrl Pts',(0.117604813820203,-0.198806317010017,
0.455864321307767));
#31873=CARTESIAN_POINT('Ctrl Pts',(0.230814590995695,-0.00891451065749571,
0.466982963290884));
#31874=CARTESIAN_POINT('Ctrl Pts',(0.132588189186442,0.189143374203362,
0.478101605273999));
#31875=CARTESIAN_POINT('Ctrl Pts',(-0.0870947461077786,0.21393772252035,
0.489220247257116));
#31876=CARTESIAN_POINT('Ctrl Pts',(-0.226995115459196,0.0427558355600586,
0.500338889240232));
#31877=CARTESIAN_POINT('Ctrl Pts',(-0.158958111120973,-0.167592251687317,
0.511457531223348));
#31878=CARTESIAN_POINT('Ctrl Pts',(0.0546914192237968,-0.224418565586851,
0.522576173206465));
#31879=CARTESIAN_POINT('Ctrl Pts',(0.21824123683356,-0.0756677372605439,
0.533694815189581));
#31880=CARTESIAN_POINT('Ctrl Pts',(0.181872613351991,0.14239802115651,0.544813457172697));
#31881=CARTESIAN_POINT('Ctrl Pts',(-0.0210992142997687,0.230021014415434,
0.555932099155813));
#31882=CARTESIAN_POINT('Ctrl Pts',(-0.204743246287144,0.106934779265563,
0.567050741138931));
#31883=CARTESIAN_POINT('Ctrl Pts',(-0.200833582118916,-0.114108352937273,
0.578169383122044));
#31884=CARTESIAN_POINT('Ctrl Pts',(-0.0129516437895867,-0.230623283386393,
0.589288025105164));
#31885=CARTESIAN_POINT('Ctrl Pts',(0.186794562143574,-0.135877280920554,
0.600406667088277));
#31886=CARTESIAN_POINT('Ctrl Pts',(0.215428845280213,0.083338205752262,
0.611525309071395));
#31887=CARTESIAN_POINT('Ctrl Pts',(0.0467209600008474,0.226212280421227,
0.622643951054511));
#31888=CARTESIAN_POINT('Ctrl Pts',(-0.164785351575852,0.161866092257753,
0.633762593037627));
#31889=CARTESIAN_POINT('Ctrl Pts',(-0.225341132081031,-0.0507564587930634,
0.644881235020743));
#31890=CARTESIAN_POINT('Ctrl Pts',(-0.0794746594271866,-0.21688389157728,
0.655999877003859));
#31891=CARTESIAN_POINT('Ctrl Pts',(0.139194049181108,-0.184336270411821,
0.667118518986976));
#31892=CARTESIAN_POINT('Ctrl Pts',(0.230354969961477,0.0170713716736379,
0.678237160970093));
#31893=CARTESIAN_POINT('Ctrl Pts',(0.11050074456459,0.202840896683692,0.689355802953208));
#31894=CARTESIAN_POINT('Ctrl Pts',(-0.110576956804586,0.202799360306213,
0.700474444936325));
#31895=CARTESIAN_POINT('Ctrl Pts',(-0.230361368483253,0.0169848116649841,
0.711593086919441));
#31896=CARTESIAN_POINT('Ctrl Pts',(-0.139124772661127,-0.184388561328419,
0.722711728902557));
#31897=CARTESIAN_POINT('Ctrl Pts',(0.0795561506911461,-0.216854012653626,
0.733830370885674));
#31898=CARTESIAN_POINT('Ctrl Pts',(0.225360188555757,-0.0506717804195071,
0.744949012868789));
#31899=CARTESIAN_POINT('Ctrl Pts',(0.164724516703786,0.161928001017393,
0.756067654851907));
#31900=CARTESIAN_POINT('Ctrl Pts',(-0.0468059588377044,0.226194708457211,
0.767186296835021));
#31901=CARTESIAN_POINT('Ctrl Pts',(-0.2154601454596,0.0832572497460946,
0.778304938818139));
#31902=CARTESIAN_POINT('Ctrl Pts',(-0.18674349134348,-0.135947461755279,
0.789423580801255));
#31903=CARTESIAN_POINT('Ctrl Pts',(0.0130383025010703,-0.230618400359892,
0.800542222784371));
#31904=CARTESIAN_POINT('Ctrl Pts',(0.200876445601631,-0.114032879114536,
0.811660864767487));
#31905=CARTESIAN_POINT('Ctrl Pts',(0.204703049732954,0.107011706590215,
0.822779506750604));
#31906=CARTESIAN_POINT('Ctrl Pts',(0.0210127794931219,0.230028926472067,
0.83389814873372));
#31907=CARTESIAN_POINT('Ctrl Pts',(-0.181926108372479,0.142329670163983,
0.845016790716836));
#31908=CARTESIAN_POINT('Ctrl Pts',(-0.218212788319439,-0.0757497388391501,
0.856135432699953));
#31909=CARTESIAN_POINT('Ctrl Pts',(-0.0546070872270015,-0.224439100726275,
0.867254074683069));
#31910=CARTESIAN_POINT('Ctrl Pts',(0.159021074792356,-0.167532509350284,
0.878372716666185));
#31911=CARTESIAN_POINT('Ctrl Pts',(0.226979033427429,0.0428411288796547,
0.889491358649301));
#31912=CARTESIAN_POINT('Ctrl Pts',(0.0870143500653468,0.213970434291613,
0.900610000632417));
#31913=CARTESIAN_POINT('Ctrl Pts',(-0.132659252698235,0.189093539309814,
0.911728642615534));
#31914=CARTESIAN_POINT('Ctrl Pts',(-0.230811225247311,-0.00900124183420705,
0.92284728459865));
#31915=CARTESIAN_POINT('Ctrl Pts',(-0.117530100973675,-0.198850493915805,
0.933965926581767));
#31916=CARTESIAN_POINT('Ctrl Pts',(0.103413692781901,-0.206544068631896,
0.945084568564882));
#31917=CARTESIAN_POINT('Ctrl Pts',(0.229626061120593,-0.0250343120523647,
0.956203210547999));
#31918=CARTESIAN_POINT('Ctrl Pts',(0.145490988438074,0.179407953322179,
0.967321852531115));
#31919=CARTESIAN_POINT('Ctrl Pts',(-0.0719201283577143,0.219504763615053,
0.978440494514231));
#31920=CARTESIAN_POINT('Ctrl Pts',(-0.22344931264651,0.0585256616254353,
0.989559136497349));
#31921=CARTESIAN_POINT('Ctrl Pts',(-0.170289184396906,-0.156065436285928,
1.00067777848046));
#31922=CARTESIAN_POINT('Ctrl Pts',(0.0388631330803271,-0.227693917494037,
1.01179642046358));
#31923=CARTESIAN_POINT('Ctrl Pts',(0.21241530878674,-0.0907447137301155,
1.0229150624467));
#31924=CARTESIAN_POINT('Ctrl Pts',(0.191385514681521,0.129330245229283,
1.03403370442981));
#31925=CARTESIAN_POINT('Ctrl Pts',(-0.00496108271125438,0.230933734912719,
1.04515234641293));
#31926=CARTESIAN_POINT('Ctrl Pts',(-0.196764314760194,0.120990674417448,
1.05627098839605));
#31927=CARTESIAN_POINT('Ctrl Pts',(-0.208320610464741,-0.0997827509202423,
1.06738963037916));
#31928=CARTESIAN_POINT('Ctrl Pts',(-0.0290505442625618,-0.229155305943203,
1.07850827236228));
#31929=CARTESIAN_POINT('Ctrl Pts',(0.17683937169233,-0.148603171255794,
1.08962691434539));
#31930=CARTESIAN_POINT('Ctrl Pts',(0.220720967111538,0.0680597564112484,
1.10074555632851));
#31931=CARTESIAN_POINT('Ctrl Pts',(0.0624426335084105,0.222407759459687,
1.11186419831163));
#31932=CARTESIAN_POINT('Ctrl Pts',(-0.153093107010227,0.172962013887028,
1.12298284029474));
#31933=CARTESIAN_POINT('Ctrl Pts',(-0.228279649924591,-0.0348126912135875,
1.13410148227786));
#31934=CARTESIAN_POINT('Ctrl Pts',(-0.0945626503816835,-0.210911975270116,
1.14522012426097));
#31935=CARTESIAN_POINT('Ctrl Pts',(0.126200083066393,-0.193383031585166,
1.15633876624409));
#31936=CARTESIAN_POINT('Ctrl Pts',(0.195657378287586,-0.0642246683396576,
1.16375119423284));
#31937=CARTESIAN_POINT('Ctrl Pts',(0.195398449819998,0.00077833665056624,
1.16745740822721));
#31938=CARTESIAN_POINT('Ctrl Pts',(-0.195093054978418,-5.50606481354719E-5,
1.06241303078758));
#31939=CARTESIAN_POINT('Ctrl Pts',(-0.195166977968097,-0.0292567552961119,
1.0640718973181));
#31940=CARTESIAN_POINT('Ctrl Pts',(-0.189027401228485,-0.0584289311968449,
1.06573076384863));
#31941=CARTESIAN_POINT('Ctrl Pts',(-0.17651621681362,-0.0845492725344543,
1.06738963037916));
#31942=CARTESIAN_POINT('Ctrl Pts',(-0.148563921730681,-0.142906935927896,
1.07109584437353));
#31943=CARTESIAN_POINT('Ctrl Pts',(-0.0888072329966215,-0.18603112093555,
1.07480205836791));
#31944=CARTESIAN_POINT('Ctrl Pts',(-0.0246139026371096,-0.194167857658142,
1.07850827236228));
#31945=CARTESIAN_POINT('Ctrl Pts',(0.0395794277224022,-0.202304594380734,
1.08221448635665));
#31946=CARTESIAN_POINT('Ctrl Pts',(0.108209399707366,-0.175453882818264,
1.08592070035102));
#31947=CARTESIAN_POINT('Ctrl Pts',(0.149837984936383,-0.125918039092522,
1.08962691434539));
#31948=CARTESIAN_POINT('Ctrl Pts',(0.191466570165399,-0.0763821953667804,
1.09333312833977));
#31949=CARTESIAN_POINT('Ctrl Pts',(0.206093768638468,-0.0041612194777677,
1.09703934233414));
#31950=CARTESIAN_POINT('Ctrl Pts',(0.187027645607817,0.0576739356414784,
1.10074555632851));
#31951=CARTESIAN_POINT('Ctrl Pts',(0.180418088670294,0.0791100177355746,
1.10203037088567));
#31952=CARTESIAN_POINT('Ctrl Pts',(0.169759382901609,0.0992979671982257,
1.10331518544284));
#31953=CARTESIAN_POINT('Ctrl Pts',(0.156057659382855,0.117255425406022,
1.1046));
#31954=CARTESIAN_POINT('Ctrl Pts',(-0.09055496143049,-0.12679201530598,
5.09575021068187E-18));
#31955=CARTESIAN_POINT('Ctrl Pts',(-0.0937460871048188,-0.125085822491965,
4.58984227758833E-18));
#31956=CARTESIAN_POINT('Ctrl Pts',(-0.0968677330061127,-0.123263760516135,
2.50662287286079E-17));
#31957=CARTESIAN_POINT('Ctrl Pts',(-0.0999128467894991,-0.121327242330634,
2.00577401909818E-17));
#31958=CARTESIAN_POINT('Ctrl Pts',(-0.107335152566795,-0.11660708041271,
6.42545598945985E-18));
#31959=CARTESIAN_POINT('Ctrl Pts',(-0.11430344392066,-0.111208610599775,
9.99023806675092E-18));
#31960=CARTESIAN_POINT('Ctrl Pts',(-0.120790707516777,-0.105232728283189,
2.60208521396521E-17));
#31961=CARTESIAN_POINT('Ctrl Pts',(-0.123891078118351,-0.102376755255687,
3.36821478247169E-17));
#31962=CARTESIAN_POINT('Ctrl Pts',(-0.126881418116351,-0.099388034385428,
-1.92452104322545E-17));
#31963=CARTESIAN_POINT('Ctrl Pts',(-0.129748204847616,-0.0962880923092239,
-1.51788304147971E-17));
#31964=CARTESIAN_POINT('Ctrl Pts',(-0.135037647654988,-0.0905684598931024,
-7.67604539740766E-18));
#31965=CARTESIAN_POINT('Ctrl Pts',(-0.139916189540312,-0.0844627163539483,
6.65058155921973E-18));
#31966=CARTESIAN_POINT('Ctrl Pts',(-0.144364609008094,-0.0780350740853688,
-6.07153216591882E-18));
#31967=CARTESIAN_POINT('Ctrl Pts',(-0.146693883418799,-0.0746694421422029,
-1.2733065360948E-17));
#31968=CARTESIAN_POINT('Ctrl Pts',(-0.148905919766188,-0.0712140221787596,
5.51914947350105E-18));
#31969=CARTESIAN_POINT('Ctrl Pts',(-0.150994732263837,-0.0676811328914676,
3.46944695195361E-18));
#31970=CARTESIAN_POINT('Ctrl Pts',(-0.156930492501974,-0.0576417522477531,
-2.35517480854577E-18));
#31971=CARTESIAN_POINT('Ctrl Pts',(-0.161837586723136,-0.04704232833817,
1.0498384979768E-17));
#31972=CARTESIAN_POINT('Ctrl Pts',(-0.165656700638674,-0.0360824270657778,
6.93889390390723E-18));
#31973=CARTESIAN_POINT('Ctrl Pts',(-0.168566598677898,-0.0277317478433351,
4.22681033390876E-18));
#31974=CARTESIAN_POINT('Ctrl Pts',(-0.17084455406887,-0.0191704748820838,
-1.37633633951559E-17));
#31975=CARTESIAN_POINT('Ctrl Pts',(-0.172449224480544,-0.0104741012692795,
-1.56125112837913E-17));
#31976=CARTESIAN_POINT('Ctrl Pts',(-0.173092222694612,-0.00698942761839798,
-1.63534726558537E-17));
#31977=CARTESIAN_POINT('Ctrl Pts',(-0.173626618765139,-0.00348302750915761,
-1.21488779396688E-17));
#31978=CARTESIAN_POINT('Ctrl Pts',(-0.174048178602262,2.59546856150664E-5,
-1.38777878078145E-17));
#31979=CARTESIAN_POINT('Ctrl Pts',(-0.174866886128293,0.00684071709555691,
-1.72354879401115E-17));
#31980=CARTESIAN_POINT('Ctrl Pts',(-0.175263001859704,0.0136781916586682,
-1.47570089434246E-17));
#31981=CARTESIAN_POINT('Ctrl Pts',(-0.175222496230419,0.020502014676713,
-1.73472347597681E-17));
#31982=CARTESIAN_POINT('Ctrl Pts',(-0.175176789703203,0.0282020123806742,
-2.02700439806174E-17));
#31983=CARTESIAN_POINT('Ctrl Pts',(-0.174575488437737,0.0358847565960055,
-4.14656083691159E-17));
#31984=CARTESIAN_POINT('Ctrl Pts',(-0.173454133268089,0.0435109284941294,
-3.81639164714898E-17));
#31985=CARTESIAN_POINT('Ctrl Pts',(-0.172772227559337,0.0481484691182048,
-3.61561292739328E-17));
#31986=CARTESIAN_POINT('Ctrl Pts',(-0.171897804056446,0.0527651363053484,
-4.88916554017709E-17));
#31987=CARTESIAN_POINT('Ctrl Pts',(-0.170837068741884,0.0573521982187067,
-5.03069808033274E-17));
#31988=CARTESIAN_POINT('Ctrl Pts',(-0.170031029630167,0.0608378475218587,
-5.1382468357856E-17));
#31989=CARTESIAN_POINT('Ctrl Pts',(-0.169117246541092,0.0643057763689402,
-8.52354934901958E-18));
#31990=CARTESIAN_POINT('Ctrl Pts',(-0.168102750715484,0.0677391082731898,
-8.67361737988404E-18));
#31991=CARTESIAN_POINT('Ctrl Pts',(-0.164848133533702,0.0787536247692379,
-9.1550525709997E-18));
#31992=CARTESIAN_POINT('Ctrl Pts',(-0.160552714845615,0.0894467883889295,
-1.4615508474092E-17));
#31993=CARTESIAN_POINT('Ctrl Pts',(-0.155326482610649,0.0996955319262882,
-3.12250225675825E-17));
#31994=CARTESIAN_POINT('Ctrl Pts',(-0.152120282364142,0.105982953261303,
-4.14146631703528E-17));
#31995=CARTESIAN_POINT('Ctrl Pts',(-0.148562901683281,0.112103241720107,
-3.61201279282247E-17));
#31996=CARTESIAN_POINT('Ctrl Pts',(-0.144672442230625,0.118026999364952,
-4.16333634234434E-17));
#31997=CARTESIAN_POINT('Ctrl Pts',(-0.141744976772053,0.122484466690154,
-4.57819239401724E-17));
#31998=CARTESIAN_POINT('Ctrl Pts',(-0.138624730042886,0.126835138052646,
-6.23512024481927E-18));
#31999=CARTESIAN_POINT('Ctrl Pts',(-0.135339728450536,0.131039395408961,
-6.93889390390723E-18));
#32000=CARTESIAN_POINT('Ctrl Pts',(-0.127443588741529,0.141145144987709,
-8.63055065945266E-18));
#32001=CARTESIAN_POINT('Ctrl Pts',(-0.118584883784043,0.150432575075823,
-5.34207396488032E-18));
#32002=CARTESIAN_POINT('Ctrl Pts',(-0.108881311648901,0.158738497602418,
0.));
#32003=CARTESIAN_POINT('Ctrl Pts',(-0.101751737768341,0.16484116654483,
3.92501961933201E-18));
#32004=CARTESIAN_POINT('Ctrl Pts',(-0.0941648935161059,0.170414009123921,
-1.10648570806265E-17));
#32005=CARTESIAN_POINT('Ctrl Pts',(-0.0861525859670525,0.175382131162755,
-1.38777878078145E-17));
#32006=CARTESIAN_POINT('Origin',(0.,0.,0.));
#32007=CARTESIAN_POINT('Origin',(-0.0866025403784439,-0.15,-0.4));
#32008=CARTESIAN_POINT('',(-0.0866025403784439,-0.15,-0.4));
#32009=CARTESIAN_POINT('',(0.0866025403784439,-0.15,-0.4));
#32010=CARTESIAN_POINT('',(-0.043301270189222,-0.15,-0.4));
#32011=CARTESIAN_POINT('',(-0.0866025403784439,-0.15,-0.2));
#32012=CARTESIAN_POINT('',(-0.0866025403784439,-0.15,-0.4));
#32013=CARTESIAN_POINT('',(0.0866025403784439,-0.15,-0.2));
#32014=CARTESIAN_POINT('',(-0.0866025403784439,-0.15,-0.2));
#32015=CARTESIAN_POINT('',(0.0866025403784439,-0.15,-0.4));
#32016=CARTESIAN_POINT('Origin',(-0.173205080756888,2.12115047744981E-17,
-0.4));
#32017=CARTESIAN_POINT('',(-0.173205080756888,2.12115047744981E-17,-0.4));
#32018=CARTESIAN_POINT('',(-0.151554445662277,-0.0375,-0.4));
#32019=CARTESIAN_POINT('',(-0.173205080756888,2.77555756156289E-17,-0.2));
#32020=CARTESIAN_POINT('',(-0.173205080756888,2.12115047744981E-17,-0.4));
#32021=CARTESIAN_POINT('',(-0.173205080756888,2.12115047744981E-17,-0.2));
#32022=CARTESIAN_POINT('Origin',(-0.0866025403784438,0.15,-0.4));
#32023=CARTESIAN_POINT('',(-0.0866025403784438,0.15,-0.4));
#32024=CARTESIAN_POINT('',(-0.108253175473055,0.1125,-0.4));
#32025=CARTESIAN_POINT('',(-0.0866025403784438,0.15,-0.2));
#32026=CARTESIAN_POINT('',(-0.0866025403784438,0.15,-0.4));
#32027=CARTESIAN_POINT('',(-0.0866025403784438,0.15,-0.2));
#32028=CARTESIAN_POINT('Origin',(0.0866025403784439,0.15,-0.4));
#32029=CARTESIAN_POINT('',(0.0866025403784439,0.15,-0.4));
#32030=CARTESIAN_POINT('',(0.043301270189222,0.15,-0.4));
#32031=CARTESIAN_POINT('',(0.0866025403784439,0.15,-0.2));
#32032=CARTESIAN_POINT('',(0.0866025403784439,0.15,-0.4));
#32033=CARTESIAN_POINT('',(0.0866025403784439,0.15,-0.2));
#32034=CARTESIAN_POINT('Origin',(0.173205080756888,0.,-0.4));
#32035=CARTESIAN_POINT('',(0.173205080756888,0.,-0.4));
#32036=CARTESIAN_POINT('',(0.151554445662277,0.0375,-0.4));
#32037=CARTESIAN_POINT('',(0.173205080756888,0.,-0.2));
#32038=CARTESIAN_POINT('',(0.173205080756888,0.,-0.4));
#32039=CARTESIAN_POINT('',(0.173205080756888,0.,-0.2));
#32040=CARTESIAN_POINT('Origin',(0.0866025403784439,-0.15,-0.4));
#32041=CARTESIAN_POINT('',(0.108253175473055,-0.1125,-0.4));
#32042=CARTESIAN_POINT('',(0.0866025403784439,-0.15,-0.2));
#32043=CARTESIAN_POINT('Origin',(0.,2.77555756156289E-17,-0.2));
#32044=CARTESIAN_POINT('Origin',(0.,0.,0.));
#32045=CARTESIAN_POINT('',(-0.35,-4.28626379701574E-17,0.));
#32046=CARTESIAN_POINT('Origin',(0.,0.,0.));
#32047=CARTESIAN_POINT('Origin',(0.,0.,-0.4));
#32048=CARTESIAN_POINT('',(-0.35,-4.28626379701574E-17,-0.4));
#32049=CARTESIAN_POINT('',(-0.35,-4.28626379701574E-17,-0.4));
#32050=CARTESIAN_POINT('Origin',(0.,0.,-0.4));
#32051=CARTESIAN_POINT('Origin',(0.,0.,-0.4));
#32052=CARTESIAN_POINT('Origin',(0.,0.,1.2));
#32053=CARTESIAN_POINT('',(0.,0.,0.));
#32054=CARTESIAN_POINT('Origin',(0.,0.,0.));
#32055=CARTESIAN_POINT('',(-0.146530139441781,9.2983754875535E-5,0.0160655045842905));
#32056=CARTESIAN_POINT('',(-0.146482381647069,0.000161727750000726,0.00893449541570906));
#32057=CARTESIAN_POINT('',(-0.14635,-1.79227059055215E-17,0.));
#32058=CARTESIAN_POINT('',(0.0634007094575212,0.131904027763685,0.));
#32059=CARTESIAN_POINT('Ctrl Pts',(-0.146530139441781,9.2983754875535E-5,
0.0160655045842905));
#32060=CARTESIAN_POINT('Ctrl Pts',(-0.146562770122328,0.00491041321584185,
0.015802617364053));
#32061=CARTESIAN_POINT('Ctrl Pts',(-0.146345876989778,0.00972466734833348,
0.0155397301438155));
#32062=CARTESIAN_POINT('Ctrl Pts',(-0.145869825450435,0.0145129075872385,
0.015276842923578));
#32063=CARTESIAN_POINT('Ctrl Pts',(-0.141074879536054,0.0627416203906926,
0.0126289573514387));
#32064=CARTESIAN_POINT('Ctrl Pts',(-0.109987863649871,0.10833117855941,
0.00998107177929941));
#32065=CARTESIAN_POINT('Ctrl Pts',(-0.0668435938445389,0.130448755664999,
0.00733318620716011));
#32066=CARTESIAN_POINT('Ctrl Pts',(-0.0270149638383408,0.150866595604039,
0.00488879080477341));
#32067=CARTESIAN_POINT('Ctrl Pts',(0.0230889279919825,0.151281476944728,
0.00244439540238672));
#32068=CARTESIAN_POINT('Ctrl Pts',(0.0635548502597316,0.132093933345895,
1.98375346423187E-17));
#32069=CARTESIAN_POINT('',(-0.0634007094575231,0.131904027763684,0.));
#32070=CARTESIAN_POINT('Origin',(0.,0.,0.));
#32071=CARTESIAN_POINT('Ctrl Pts',(-0.063400709457523,0.131904027763684,
7.63278329429795E-17));
#32072=CARTESIAN_POINT('Ctrl Pts',(-0.107339749959442,0.110784382003545,
0.00265083470503432));
#32073=CARTESIAN_POINT('Ctrl Pts',(-0.139511904869873,0.0661645412785542,
0.00530166941006857));
#32074=CARTESIAN_POINT('Ctrl Pts',(-0.145460797893518,0.0180856147189845,
0.00795250411510281));
#32075=CARTESIAN_POINT('Ctrl Pts',(-0.146195379242097,0.0121487315761866,
0.00827983454863823));
#32076=CARTESIAN_POINT('Ctrl Pts',(-0.146530113272026,0.00615910494930538,
0.00860716498217364));
#32077=CARTESIAN_POINT('Ctrl Pts',(-0.146482381647069,0.000161727750000726,
0.00893449541570906));
#32078=CARTESIAN_POINT('Origin',(0.,0.,0.));
#32079=CARTESIAN_POINT('',(-0.146153148300412,8.02585168747302E-5,0.0660655045842906));
#32080=CARTESIAN_POINT('',(-0.146138869890956,7.0051777900314E-5,0.058934495415709));
#32081=CARTESIAN_POINT('',(-0.14635,-1.79227059055215E-17,0.));
#32082=CARTESIAN_POINT('Ctrl Pts',(-0.146153148300412,8.02585168747302E-5,
0.0660655045842906));
#32083=CARTESIAN_POINT('Ctrl Pts',(-0.146248563607689,0.0193075654691076,
0.0650232641302222));
#32084=CARTESIAN_POINT('Ctrl Pts',(-0.142725320554989,0.0385012587497889,
0.0639810236761539));
#32085=CARTESIAN_POINT('Ctrl Pts',(-0.135419901199499,0.0561272788093185,
0.0629387832220855));
#32086=CARTESIAN_POINT('Ctrl Pts',(-0.116859966748363,0.100907429136131,
0.0602908976499462));
#32087=CARTESIAN_POINT('Ctrl Pts',(-0.0738879770866151,0.13556903337647,
0.0576430120778069));
#32088=CARTESIAN_POINT('Ctrl Pts',(-0.0261938646990992,0.144231038496032,
0.0549951265056676));
#32089=CARTESIAN_POINT('Ctrl Pts',(0.0215002476884163,0.152893043615593,
0.0523472409335283));
#32090=CARTESIAN_POINT('Ctrl Pts',(0.0739164828016995,0.135555449614377,
0.049699355361389));
#32091=CARTESIAN_POINT('Ctrl Pts',(0.107036887564708,0.100160226311824,
0.0470514697892497));
#32092=CARTESIAN_POINT('Ctrl Pts',(0.140157292327717,0.0647650030092702,
0.0444035842171104));
#32093=CARTESIAN_POINT('Ctrl Pts',(0.153981866740452,0.0113121504053791,
0.0417556986449711));
#32094=CARTESIAN_POINT('Ctrl Pts',(0.142176802105062,-0.0357014716925755,
0.0391078130728318));
#32095=CARTESIAN_POINT('Ctrl Pts',(0.130371737469673,-0.0827150937905301,
0.0364599275006924));
#32096=CARTESIAN_POINT('Ctrl Pts',(0.0929370337861598,-0.123289485382548,
0.0338120419285532));
#32097=CARTESIAN_POINT('Ctrl Pts',(0.047024206385633,-0.138841291698229,
0.0311641563564138));
#32098=CARTESIAN_POINT('Ctrl Pts',(0.0011113789851062,-0.15439309801391,
0.0285162707842745));
#32099=CARTESIAN_POINT('Ctrl Pts',(-0.0532795721324345,-0.144922319053254,
0.0258683852121352));
#32100=CARTESIAN_POINT('Ctrl Pts',(-0.091223609719915,-0.11475299585383,
0.0232204996399959));
#32101=CARTESIAN_POINT('Ctrl Pts',(-0.125400489590719,-0.0875789416327165,
0.0208355012880941));
#32102=CARTESIAN_POINT('Ctrl Pts',(-0.146234103296486,-0.0436123029244358,
0.0184505029361923));
#32103=CARTESIAN_POINT('Ctrl Pts',(-0.146530139441781,9.2983754875535E-5,
0.0160655045842905));
#32104=CARTESIAN_POINT('Ctrl Pts',(-0.146482381647069,0.000161727750000726,
0.00893449541570906));
#32105=CARTESIAN_POINT('Ctrl Pts',(-0.146143566116611,-0.0424097233364945,
0.0112579996872079));
#32106=CARTESIAN_POINT('Ctrl Pts',(-0.126533645440834,-0.0853716986287587,
0.0135815039587068));
#32107=CARTESIAN_POINT('Ctrl Pts',(-0.0938693583126354,-0.112632000129883,
0.0159050082302056));
#32108=CARTESIAN_POINT('Ctrl Pts',(-0.0566033945712489,-0.143732676025031,
0.0185558429352399));
#32109=CARTESIAN_POINT('Ctrl Pts',(-0.00234583595161722,-0.154396015421179,
0.0212066776402742));
#32110=CARTESIAN_POINT('Ctrl Pts',(0.0439541262059228,-0.139833200290426,
0.0238575123453084));
#32111=CARTESIAN_POINT('Ctrl Pts',(0.0902540883634627,-0.125270385159674,
0.0265083470503427));
#32112=CARTESIAN_POINT('Ctrl Pts',(0.128596454058911,-0.0854814155020214,
0.029159181755377));
#32113=CARTESIAN_POINT('Ctrl Pts',(0.141395806078876,-0.0386806767328055,
0.0318100164604112));
#32114=CARTESIAN_POINT('Ctrl Pts',(0.154195158098842,0.00812006203641059,
0.0344608511654455));
#32115=CARTESIAN_POINT('Ctrl Pts',(0.141451496443324,0.0619325699171903,
0.0371116858704798));
#32116=CARTESIAN_POINT('Ctrl Pts',(0.109005912554766,0.0980207644158424,
0.0397625205755141));
#32117=CARTESIAN_POINT('Ctrl Pts',(0.0765603286662091,0.134108958914494,
0.0424133552805484));
#32118=CARTESIAN_POINT('Ctrl Pts',(0.0244128225446121,0.152472840031019,
0.0450641899855826));
#32119=CARTESIAN_POINT('Ctrl Pts',(-0.0234881253671046,0.144695681732891,
0.0477150246906169));
#32120=CARTESIAN_POINT('Ctrl Pts',(-0.0713890732788212,0.136918523434763,
0.0503658593956511));
#32121=CARTESIAN_POINT('Ctrl Pts',(-0.115043462980658,0.103000325721984,
0.0530166941006854));
#32122=CARTESIAN_POINT('Ctrl Pts',(-0.134410456092164,0.0585065536587812,
0.0556675288057197));
#32123=CARTESIAN_POINT('Ctrl Pts',(-0.142366606622288,0.0402280761403725,
0.0567565176757161));
#32124=CARTESIAN_POINT('Ctrl Pts',(-0.14622390219053,0.0201648150927879,
0.0578455065457126));
#32125=CARTESIAN_POINT('Ctrl Pts',(-0.146138869890956,7.0051777900314E-5,
0.058934495415709));
#32126=CARTESIAN_POINT('Origin',(0.,0.,0.));
#32127=CARTESIAN_POINT('',(-0.146239229308481,-0.000121680145597616,0.116065504584291));
#32128=CARTESIAN_POINT('',(-0.146251911109041,-0.00012571917928438,0.108934495415709));
#32129=CARTESIAN_POINT('',(-0.14635,-1.79227059055215E-17,0.));
#32130=CARTESIAN_POINT('Ctrl Pts',(-0.146239229308481,-0.000121680145597616,
0.116065504584291));
#32131=CARTESIAN_POINT('Ctrl Pts',(-0.145975985392548,0.0334333989639988,
0.114243910896391));
#32132=CARTESIAN_POINT('Ctrl Pts',(-0.134505001919181,0.0671510842014817,
0.112422317208492));
#32133=CARTESIAN_POINT('Ctrl Pts',(-0.113362446108109,0.09293957845923,
0.110600723520593));
#32134=CARTESIAN_POINT('Ctrl Pts',(-0.0826294298146382,0.130425974204838,
0.107952837948454));
#32135=CARTESIAN_POINT('Ctrl Pts',(-0.0314605739124977,0.151158147427946,
0.105304952376314));
#32136=CARTESIAN_POINT('Ctrl Pts',(0.0166981167953111,0.145636463652384,
0.102657066804175));
#32137=CARTESIAN_POINT('Ctrl Pts',(0.0648568075031199,0.140114779876822,
0.100009181232036));
#32138=CARTESIAN_POINT('Ctrl Pts',(0.110005333016597,0.10833923910259,0.0973612956598965));
#32139=CARTESIAN_POINT('Ctrl Pts',(0.1314562431614,0.0648696188566969,0.0947134100877572));
#32140=CARTESIAN_POINT('Ctrl Pts',(0.152907153306203,0.0213999986108032,
0.0920655245156179));
#32141=CARTESIAN_POINT('Ctrl Pts',(0.150660448082332,-0.0337637011067522,
0.0894176389434786));
#32142=CARTESIAN_POINT('Ctrl Pts',(0.125745602608234,-0.075344908113871,
0.0867697533713393));
#32143=CARTESIAN_POINT('Ctrl Pts',(0.100830757134136,-0.11692611512099,
0.0841218677992));
#32144=CARTESIAN_POINT('Ctrl Pts',(0.053247771409812,-0.144924829417672,
0.0814739822270607));
#32145=CARTESIAN_POINT('Ctrl Pts',(0.00479954857812182,-0.146511973337632,
0.0788260966549214));
#32146=CARTESIAN_POINT('Ctrl Pts',(-0.0436486742535683,-0.148099117257592,
0.0761782110827821));
#32147=CARTESIAN_POINT('Ctrl Pts',(-0.0929621341926243,-0.123274690800829,
0.0735303255106428));
#32148=CARTESIAN_POINT('Ctrl Pts',(-0.120544924541891,-0.0834131293658051,
0.0708824399385034));
#32149=CARTESIAN_POINT('Ctrl Pts',(-0.137270788050899,-0.059241570673742,
0.0692767948204325));
#32150=CARTESIAN_POINT('Ctrl Pts',(-0.146006154272575,-0.0295407674383123,
0.0676711497023615));
#32151=CARTESIAN_POINT('Ctrl Pts',(-0.146153148300412,8.02585168747302E-5,
0.0660655045842906));
#32152=CARTESIAN_POINT('Ctrl Pts',(-0.146138869890956,7.0051777900314E-5,
0.058934495415709));
#32153=CARTESIAN_POINT('Ctrl Pts',(-0.14601691516158,-0.0287501898739087,
0.0604963412507468));
#32154=CARTESIAN_POINT('Ctrl Pts',(-0.137785682499354,-0.0576352309664648,
0.0620581870857847));
#32155=CARTESIAN_POINT('Ctrl Pts',(-0.121906950385236,-0.0814126279516829,
0.0636200329208225));
#32156=CARTESIAN_POINT('Ctrl Pts',(-0.0949568550456235,-0.121768691085319,
0.0662708676258568));
#32157=CARTESIAN_POINT('Ctrl Pts',(-0.0459770678452217,-0.147411470938967,
0.068921702330891));
#32158=CARTESIAN_POINT('Ctrl Pts',(0.00254289383979588,-0.146569427669784,
0.0715725370359253));
#32159=CARTESIAN_POINT('Ctrl Pts',(0.0510628555248136,-0.145727384400601,
0.0742233717409596));
#32160=CARTESIAN_POINT('Ctrl Pts',(0.0991229916944473,-0.118400518008588,
0.0768742064459939));
#32161=CARTESIAN_POINT('Ctrl Pts',(0.124657213858417,-0.0771346353870958,
0.0795250411510281));
#32162=CARTESIAN_POINT('Ctrl Pts',(0.150191436022387,-0.0358687527656039,
0.0821758758560624));
#32163=CARTESIAN_POINT('Ctrl Pts',(0.153199744180694,0.0193361460853669,
0.0848267105610966));
#32164=CARTESIAN_POINT('Ctrl Pts',(0.132300679968259,0.0631324945868766,
0.0874775452661308));
#32165=CARTESIAN_POINT('Ctrl Pts',(0.111401615755824,0.106928843088387,
0.0901283799711651));
#32166=CARTESIAN_POINT('Ctrl Pts',(0.0665951791726482,0.139316641240435,
0.0927792146761994));
#32167=CARTESIAN_POINT('Ctrl Pts',(0.0184540622028837,0.145425561817519,
0.0954300493812337));
#32168=CARTESIAN_POINT('Ctrl Pts',(-0.0296870547668806,0.151534482394603,
0.098080884086268));
#32169=CARTESIAN_POINT('Ctrl Pts',(-0.0811628521232332,0.131364525396722,
0.100731718791302));
#32170=CARTESIAN_POINT('Ctrl Pts',(-0.11233861635763,0.0941764269143644,
0.103382553496337));
#32171=CARTESIAN_POINT('Ctrl Pts',(-0.134103588725605,0.0682140181085839,
0.105233200802794));
#32172=CARTESIAN_POINT('Ctrl Pts',(-0.145974404722175,0.0339570340187871,
0.107083848109252));
#32173=CARTESIAN_POINT('Ctrl Pts',(-0.146251911109041,-0.00012571917928438,
0.108934495415709));
#32174=CARTESIAN_POINT('Origin',(0.,0.,0.));
#32175=CARTESIAN_POINT('',(-0.146588437557148,-1.60561805771647E-5,0.166065504584291));
#32176=CARTESIAN_POINT('',(-0.146590338660816,-1.32548991986104E-5,0.158934495415709));
#32177=CARTESIAN_POINT('',(-0.14635,-1.79227059055215E-17,0.));
#32178=CARTESIAN_POINT('Ctrl Pts',(-0.146588437557148,-1.60561805771647E-5,
0.166065504584291));
#32179=CARTESIAN_POINT('Ctrl Pts',(-0.146514434076835,0.0476007616257437,
0.163464557662561));
#32180=CARTESIAN_POINT('Ctrl Pts',(-0.121147481081461,0.0952852365283555,
0.160863610740831));
#32181=CARTESIAN_POINT('Ctrl Pts',(-0.0815892695913163,0.121786698620987,
0.158262663819101));
#32182=CARTESIAN_POINT('Ctrl Pts',(-0.0413171607723027,0.148766426092319,
0.155614778246961));
#32183=CARTESIAN_POINT('Ctrl Pts',(0.0136630407409267,0.153791672495834,
0.152966892674822));
#32184=CARTESIAN_POINT('Ctrl Pts',(0.0581589346640781,0.134559827321239,
0.150319007102683));
#32185=CARTESIAN_POINT('Ctrl Pts',(0.10265482858723,0.115327982146644,0.147671121530543));
#32186=CARTESIAN_POINT('Ctrl Pts',(0.136666414920303,0.0718390453939375,
0.145023235958404));
#32187=CARTESIAN_POINT('Ctrl Pts',(0.144609292620067,0.0240200202446034,
0.142375350386265));
#32188=CARTESIAN_POINT('Ctrl Pts',(0.152552170319831,-0.0237990049047303,
0.139727464814125));
#32189=CARTESIAN_POINT('Ctrl Pts',(0.134426339386286,-0.0759481184506919,
0.137079579241986));
#32190=CARTESIAN_POINT('Ctrl Pts',(0.0985372115045479,-0.108532146892156,
0.134431693669847));
#32191=CARTESIAN_POINT('Ctrl Pts',(0.06264808362281,-0.141116175333621,
0.131783808097708));
#32192=CARTESIAN_POINT('Ctrl Pts',(0.00899565879287956,-0.154135118670589,
0.129135922525568));
#32193=CARTESIAN_POINT('Ctrl Pts',(-0.0378360619111076,-0.141623588974912,
0.126488036953429));
#32194=CARTESIAN_POINT('Ctrl Pts',(-0.0846677826150948,-0.129112059279235,
0.12384015138129));
#32195=CARTESIAN_POINT('Ctrl Pts',(-0.124678799193139,-0.0910700565509135,
0.12119226580915));
#32196=CARTESIAN_POINT('Ctrl Pts',(-0.13953571913976,-0.0449287460526992,
0.118544380237011));
#32197=CARTESIAN_POINT('Ctrl Pts',(-0.144171928689699,-0.0305300156868414,
0.117718088352771));
#32198=CARTESIAN_POINT('Ctrl Pts',(-0.146358639203649,-0.0153425769501271,
0.116891796468531));
#32199=CARTESIAN_POINT('Ctrl Pts',(-0.146239229308481,-0.000121680145597616,
0.116065504584291));
#32200=CARTESIAN_POINT('Ctrl Pts',(-0.146251911109041,-0.00012571917928438,
0.108934495415709));
#32201=CARTESIAN_POINT('Ctrl Pts',(-0.146371899997805,-0.01486250318061,
0.109734682814286));
#32202=CARTESIAN_POINT('Ctrl Pts',(-0.144324466618943,-0.0295667139196708,
0.110534870212863));
#32203=CARTESIAN_POINT('Ctrl Pts',(-0.139972258433256,-0.0435537680369422,
0.111335057611439));
#32204=CARTESIAN_POINT('Ctrl Pts',(-0.125554405162046,-0.0898896245390587,
0.113985892316474));
#32205=CARTESIAN_POINT('Ctrl Pts',(-0.0858429675071836,-0.128355097576459,
0.116636727021508));
#32206=CARTESIAN_POINT('Ctrl Pts',(-0.0390712063381835,-0.141289065177804,
0.119287561726542));
#32207=CARTESIAN_POINT('Ctrl Pts',(0.00770055483081633,-0.15422303277915,
0.121938396431576));
#32208=CARTESIAN_POINT('Ctrl Pts',(0.061532639513954,-0.141625494944442,
0.124589231136611));
#32209=CARTESIAN_POINT('Ctrl Pts',(0.0977084099269336,-0.109280503770194,
0.127240065841645));
#32210=CARTESIAN_POINT('Ctrl Pts',(0.133884180339913,-0.0769355125959451,
0.129890900546679));
#32211=CARTESIAN_POINT('Ctrl Pts',(0.152403636482735,-0.024843068082156,
0.132541735251714));
#32212=CARTESIAN_POINT('Ctrl Pts',(0.144763687764892,0.0230789149168219,
0.135192569956748));
#32213=CARTESIAN_POINT('Ctrl Pts',(0.137123739047049,0.0710008979157997,
0.137843404661782));
#32214=CARTESIAN_POINT('Ctrl Pts',(0.103324385468542,0.114752419399967,
0.140494239366816));
#32215=CARTESIAN_POINT('Ctrl Pts',(0.058884379534592,0.134245263752326,
0.143145074071851));
#32216=CARTESIAN_POINT('Ctrl Pts',(0.0144443736006417,0.153738108104685,
0.145795908776885));
#32217=CARTESIAN_POINT('Ctrl Pts',(-0.0406362846887521,0.148972275325237,
0.148446743481919));
#32218=CARTESIAN_POINT('Ctrl Pts',(-0.0810676758629916,0.122135962547369,
0.151097578186953));
#32219=CARTESIAN_POINT('Ctrl Pts',(-0.120911410803562,0.0956897062586433,
0.153709883929872));
#32220=CARTESIAN_POINT('Ctrl Pts',(-0.146528627904579,0.0478098809758598,
0.15632218967279));
#32221=CARTESIAN_POINT('Ctrl Pts',(-0.146590338660816,-1.32548991986104E-5,
0.158934495415709));
#32222=CARTESIAN_POINT('Origin',(0.,0.,0.));
#32223=CARTESIAN_POINT('',(-0.146286659309134,0.000131086592791319,0.21606550458429));
#32224=CARTESIAN_POINT('',(-0.146291727422766,0.000132510687651112,0.208934495415709));
#32225=CARTESIAN_POINT('',(-0.14635,-1.79227059055215E-17,0.));
#32226=CARTESIAN_POINT('Ctrl Pts',(-0.146286659309134,0.000131086592791319,
0.21606550458429));
#32227=CARTESIAN_POINT('Ctrl Pts',(-0.146403448836959,0.0136116234039521,
0.215333090000869));
#32228=CARTESIAN_POINT('Ctrl Pts',(-0.144693388849564,0.0270630787330369,
0.214600675417447));
#32229=CARTESIAN_POINT('Ctrl Pts',(-0.141038079685752,0.0399633448807191,
0.213868260834026));
#32230=CARTESIAN_POINT('Ctrl Pts',(-0.127823104703478,0.0866014503777888,
0.211220375261887));
#32231=CARTESIAN_POINT('Ctrl Pts',(-0.0891832035626152,0.126035366094718,
0.208572489689747));
#32232=CARTESIAN_POINT('Ctrl Pts',(-0.0428235107164534,0.140196133277333,
0.205924604117608));
#32233=CARTESIAN_POINT('Ctrl Pts',(0.00353618212970767,0.154356900459949,
0.203276718545469));
#32234=CARTESIAN_POINT('Ctrl Pts',(0.0576156666811676,0.143244519108251,
0.200628832973329));
#32235=CARTESIAN_POINT('Ctrl Pts',(0.0946352588096336,0.111950777776248,
0.19798094740119));
#32236=CARTESIAN_POINT('Ctrl Pts',(0.1316548509381,0.0806570364442455,0.195333061829051));
#32237=CARTESIAN_POINT('Ctrl Pts',(0.151614550643572,0.0291819351319375,
0.192685176256911));
#32238=CARTESIAN_POINT('Ctrl Pts',(0.145368652149886,-0.0188881928126718,
0.190037290684772));
#32239=CARTESIAN_POINT('Ctrl Pts',(0.1391227536562,-0.0669583207572802,
0.187389405112633));
#32240=CARTESIAN_POINT('Ctrl Pts',(0.106671256963357,-0.11162347533419,
0.184741519540494));
#32241=CARTESIAN_POINT('Ctrl Pts',(0.06288371648092,-0.132417699194711,
0.182093633968354));
#32242=CARTESIAN_POINT('Ctrl Pts',(0.0190961759984827,-0.153211923055232,
0.179445748396215));
#32243=CARTESIAN_POINT('Ctrl Pts',(-0.0360274082735484,-0.150135216199364,
0.176797862824076));
#32244=CARTESIAN_POINT('Ctrl Pts',(-0.0772289367619549,-0.124597352202288,
0.174149977251936));
#32245=CARTESIAN_POINT('Ctrl Pts',(-0.118430465250361,-0.0990594882052125,
0.171502091679797));
#32246=CARTESIAN_POINT('Ctrl Pts',(-0.145709937955143,-0.0510604670669293,
0.168854206107658));
#32247=CARTESIAN_POINT('Ctrl Pts',(-0.146567666245136,-0.00259385222821292,
0.166206320535519));
#32248=CARTESIAN_POINT('Ctrl Pts',(-0.146582871059412,-0.00173469218203314,
0.166159381885109));
#32249=CARTESIAN_POINT('Ctrl Pts',(-0.146589773079785,-0.000875385198767554,
0.1661124432347));
#32250=CARTESIAN_POINT('Ctrl Pts',(-0.146588437557148,-1.60561805771647E-5,
0.166065504584291));
#32251=CARTESIAN_POINT('Ctrl Pts',(-0.146590338660816,-1.32548991986104E-5,
0.158934495415709));
#32252=CARTESIAN_POINT('Ctrl Pts',(-0.146591248834288,-0.000718599514920206,
0.158973024377825));
#32253=CARTESIAN_POINT('Ctrl Pts',(-0.146586599823099,-0.0014239317987834,
0.15901155333994));
#32254=CARTESIAN_POINT('Ctrl Pts',(-0.146576355279203,-0.00212918280121965,
0.159050082302056));
#32255=CARTESIAN_POINT('Ctrl Pts',(-0.14587151946209,-0.0506512225956504,
0.16170091700709));
#32256=CARTESIAN_POINT('Ctrl Pts',(-0.118679723768778,-0.0987885094082227,
0.164351751712125));
#32257=CARTESIAN_POINT('Ctrl Pts',(-0.0774859020747837,-0.12443912668017,
0.167002586417159));
#32258=CARTESIAN_POINT('Ctrl Pts',(-0.0362920803807891,-0.150089743952118,
0.169653421122193));
#32259=CARTESIAN_POINT('Ctrl Pts',(0.0189037673138887,-0.153253691683441,
0.172304255827227));
#32260=CARTESIAN_POINT('Ctrl Pts',(0.0627588320121262,-0.132478263640569,
0.174955090532262));
#32261=CARTESIAN_POINT('Ctrl Pts',(0.106613896710364,-0.111702835597697,
0.177605925237296));
#32262=CARTESIAN_POINT('Ctrl Pts',(0.139128178412161,-0.0669880317806311,
0.18025675994233));
#32263=CARTESIAN_POINT('Ctrl Pts',(0.14537295917033,-0.0188643595177345,
0.182907594647365));
#32264=CARTESIAN_POINT('Ctrl Pts',(0.151617739928498,0.0292593127451622,
0.185558429352399));
#32265=CARTESIAN_POINT('Ctrl Pts',(0.131593019743037,0.0807918534538889,
0.188209264057433));
#32266=CARTESIAN_POINT('Ctrl Pts',(0.0944930167757219,0.11207243679613,
0.190860098762467));
#32267=CARTESIAN_POINT('Ctrl Pts',(0.0573930138084077,0.143353020138371,
0.193510933467502));
#32268=CARTESIAN_POINT('Ctrl Pts',(0.00321772805924021,0.154381646114126,
0.196161768172536));
#32269=CARTESIAN_POINT('Ctrl Pts',(-0.0431586156002514,0.14009459381994,
0.19881260287757));
#32270=CARTESIAN_POINT('Ctrl Pts',(-0.0895349592597434,0.125807541525753,
0.201463437582605));
#32271=CARTESIAN_POINT('Ctrl Pts',(-0.12811236082956,0.086204810961624,
0.204114272287639));
#32272=CARTESIAN_POINT('Ctrl Pts',(-0.141178260973432,0.0394697345298879,
0.206765106992673));
#32273=CARTESIAN_POINT('Ctrl Pts',(-0.144742548661738,0.0267207271363346,
0.207488236467018));
#32274=CARTESIAN_POINT('Ctrl Pts',(-0.146408370233879,0.0134409584703521,
0.208211365941364));
#32275=CARTESIAN_POINT('Ctrl Pts',(-0.146291727422766,0.000132510687651112,
0.208934495415709));
#32276=CARTESIAN_POINT('Origin',(0.,0.,0.));
#32277=CARTESIAN_POINT('',(-0.146128981728208,-5.54263297282837E-5,0.26606550458429));
#32278=CARTESIAN_POINT('',(-0.146122305401386,-4.76483376818115E-5,0.258934495415709));
#32279=CARTESIAN_POINT('',(-0.14635,-1.79227059055215E-17,0.));
#32280=CARTESIAN_POINT('Ctrl Pts',(-0.146128981728208,-5.54263297282837E-5,
0.26606550458429));
#32281=CARTESIAN_POINT('Ctrl Pts',(-0.146034100463789,0.0278452262029135,
0.264553736767038));
#32282=CARTESIAN_POINT('Ctrl Pts',(-0.138353701663978,0.055794258172635,
0.263041968949786));
#32283=CARTESIAN_POINT('Ctrl Pts',(-0.123420870545114,0.0790954965178402,
0.261530201132533));
#32284=CARTESIAN_POINT('Ctrl Pts',(-0.0972657774021095,0.119907989099794,
0.258882315560394));
#32285=CARTESIAN_POINT('Ctrl Pts',(-0.0488616113353708,0.146461941272529,
0.256234429988255));
#32286=CARTESIAN_POINT('Ctrl Pts',(-0.000387576818673938,0.146590104167151,
0.253586544416116));
#32287=CARTESIAN_POINT('Ctrl Pts',(0.0480864576980232,0.146718267061773,
0.250938658843976));
#32288=CARTESIAN_POINT('Ctrl Pts',(0.0966303606646785,0.120420640678281,
0.248290773271837));
#32289=CARTESIAN_POINT('Ctrl Pts',(0.123000898959779,0.0797470232084743,
0.245642887699697));
#32290=CARTESIAN_POINT('Ctrl Pts',(0.149371437254879,0.0390734057386676,
0.242995002127558));
#32291=CARTESIAN_POINT('Ctrl Pts',(0.153568610878424,-0.0159762028174541,
0.240347116555419));
#32292=CARTESIAN_POINT('Ctrl Pts',(0.133669238840564,-0.0601775991819374,
0.23769923098328));
#32293=CARTESIAN_POINT('Ctrl Pts',(0.113769866802704,-0.104378995546421,
0.235051345411141));
#32294=CARTESIAN_POINT('Ctrl Pts',(0.0697739491034383,-0.137732179719266,
0.232403459839001));
#32295=CARTESIAN_POINT('Ctrl Pts',(0.0218407929672104,-0.144954436352131,
0.229755574266862));
#32296=CARTESIAN_POINT('Ctrl Pts',(-0.0260923631690164,-0.152176692984997,
0.227107688694722));
#32297=CARTESIAN_POINT('Ctrl Pts',(-0.0779627577422058,-0.133268022077883,
0.224459803122583));
#32298=CARTESIAN_POINT('Ctrl Pts',(-0.110002930616958,-0.0968925389857218,
0.221811917550444));
#32299=CARTESIAN_POINT('Ctrl Pts',(-0.133180677518425,-0.0705786441192844,
0.219896446561726));
#32300=CARTESIAN_POINT('Ctrl Pts',(-0.145981221709449,-0.0351243244252332,
0.217980975573008));
#32301=CARTESIAN_POINT('Ctrl Pts',(-0.146286659309134,0.000131086592791319,
0.21606550458429));
#32302=CARTESIAN_POINT('Ctrl Pts',(-0.146291727422766,0.000132510687651112,
0.208934495415709));
#32303=CARTESIAN_POINT('Ctrl Pts',(-0.14598078316578,-0.035344904233501,
0.210862200646398));
#32304=CARTESIAN_POINT('Ctrl Pts',(-0.13300294931328,-0.0710261241835679,
0.212789905877087));
#32305=CARTESIAN_POINT('Ctrl Pts',(-0.109555772823034,-0.0973996609618648,
0.214717611107776));
#32306=CARTESIAN_POINT('Ctrl Pts',(-0.0773129858108336,-0.133666557722538,
0.21736844581281));
#32307=CARTESIAN_POINT('Ctrl Pts',(-0.0252730130685043,-0.152332928944543,
0.220019280517844));
#32308=CARTESIAN_POINT('Ctrl Pts',(0.0226703353838526,-0.144828233467297,
0.222670115222879));
#32309=CARTESIAN_POINT('Ctrl Pts',(0.0706136838362102,-0.137323537990051,
0.225320949927913));
#32310=CARTESIAN_POINT('Ctrl Pts',(0.114460407998596,-0.103647775813554,
0.227971784632947));
#32311=CARTESIAN_POINT('Ctrl Pts',(0.134078573855527,-0.0592629508888991,
0.230622619337982));
#32312=CARTESIAN_POINT('Ctrl Pts',(0.153696739712459,-0.014878125964245,
0.233273454043016));
#32313=CARTESIAN_POINT('Ctrl Pts',(0.149086347263938,0.0402157617085659,
0.23592428874805));
#32314=CARTESIAN_POINT('Ctrl Pts',(0.122364227775469,0.080722717223899,
0.238575123453084));
#32315=CARTESIAN_POINT('Ctrl Pts',(0.0956421082870006,0.121229672739232,
0.241225958158119));
#32316=CARTESIAN_POINT('Ctrl Pts',(0.0468082617585844,0.147149696097087,
0.243876792863153));
#32317=CARTESIAN_POINT('Ctrl Pts',(-0.00171557347725478,0.146581779641701,
0.246527627568187));
#32318=CARTESIAN_POINT('Ctrl Pts',(-0.050239408713094,0.146013863186315,
0.249178462273221));
#32319=CARTESIAN_POINT('Ctrl Pts',(-0.0984532326563563,0.118958006917689,
0.251829296978256));
#32320=CARTESIAN_POINT('Ctrl Pts',(-0.124219986251493,0.0778367286753789,
0.25448013168329));
#32321=CARTESIAN_POINT('Ctrl Pts',(-0.13865248336877,0.054803841451165,
0.255964919594096));
#32322=CARTESIAN_POINT('Ctrl Pts',(-0.146042539478052,0.0273581331787701,
0.257449707504903));
#32323=CARTESIAN_POINT('Ctrl Pts',(-0.146122305401386,-4.76483376818114E-5,
0.258934495415709));
#32324=CARTESIAN_POINT('Origin',(0.,0.,0.));
#32325=CARTESIAN_POINT('',(-0.146489966325848,-0.000104789085069334,0.31606550458429));
#32326=CARTESIAN_POINT('',(-0.146466968003471,-0.000114397412080779,0.308934495415709));
#32327=CARTESIAN_POINT('',(-0.14635,-1.79227059055215E-17,0.));
#32328=CARTESIAN_POINT('Ctrl Pts',(-0.146489966325848,-0.000104789085069334,
0.31606550458429));
#32329=CARTESIAN_POINT('Ctrl Pts',(-0.146149966214897,0.0419143941805715,
0.313774383533207));
#32330=CARTESIAN_POINT('Ctrl Pts',(-0.127114021003857,0.084202434124342,
0.311483262482124));
#32331=CARTESIAN_POINT('Ctrl Pts',(-0.09522591597141,0.111448794443947,
0.309192141431041));
#32332=CARTESIAN_POINT('Ctrl Pts',(-0.0583723183850411,0.142937852758646,
0.306544255858902));
#32333=CARTESIAN_POINT('Ctrl Pts',(-0.00435235065556675,0.154336043577878,
0.303896370286762));
#32334=CARTESIAN_POINT('Ctrl Pts',(0.0420815742217502,0.140420618022043,
0.301248484714623));
#32335=CARTESIAN_POINT('Ctrl Pts',(0.0885154990990669,0.126505192466209,
0.298600599142484));
#32336=CARTESIAN_POINT('Ctrl Pts',(0.127363381124227,0.0872761505353081,
0.295952713570344));
#32337=CARTESIAN_POINT('Ctrl Pts',(0.140824787209621,0.0407085760419468,
0.293304827998205));
#32338=CARTESIAN_POINT('Ctrl Pts',(0.154286193295015,-0.00585899845141487,
0.290656942426066));
#32339=CARTESIAN_POINT('Ctrl Pts',(0.142361123440642,-0.0597651055072374,
0.288009056853927));
#32340=CARTESIAN_POINT('Ctrl Pts',(0.110513747042986,-0.0963095040482439,
0.285361171281788));
#32341=CARTESIAN_POINT('Ctrl Pts',(0.07866637064533,-0.13285390258925,0.282713285709648));
#32342=CARTESIAN_POINT('Ctrl Pts',(0.0268966877043911,-0.152036592615441,
0.280065400137508));
#32343=CARTESIAN_POINT('Ctrl Pts',(-0.0210739885810971,-0.145067900862674,
0.277417514565369));
#32344=CARTESIAN_POINT('Ctrl Pts',(-0.0690446648665853,-0.138099209109907,
0.27476962899323));
#32345=CARTESIAN_POINT('Ctrl Pts',(-0.113216334496623,-0.104979135578184,
0.272121743421091));
#32346=CARTESIAN_POINT('Ctrl Pts',(-0.133349159202006,-0.0608835823167352,
0.269473857848951));
#32347=CARTESIAN_POINT('Ctrl Pts',(-0.141987470405663,-0.0419636782623391,
0.268337740094064));
#32348=CARTESIAN_POINT('Ctrl Pts',(-0.146200286519779,-0.0210232140769756,
0.267201622339177));
#32349=CARTESIAN_POINT('Ctrl Pts',(-0.146128981728208,-5.54263297282837E-5,
0.26606550458429));
#32350=CARTESIAN_POINT('Ctrl Pts',(-0.146122305401386,-4.76483376818114E-5,
0.258934495415709));
#32351=CARTESIAN_POINT('Ctrl Pts',(-0.146184947882857,-0.0215701994360498,
0.260100542209937));
#32352=CARTESIAN_POINT('Ctrl Pts',(-0.141739031650533,-0.0430681260504587,
0.261266589004165));
#32353=CARTESIAN_POINT('Ctrl Pts',(-0.132654825339554,-0.0623847627977247,
0.262432635798393));
#32354=CARTESIAN_POINT('Ctrl Pts',(-0.112003227585469,-0.106298275812525,
0.265083470503427));
#32355=CARTESIAN_POINT('Ctrl Pts',(-0.0673803488302883,-0.138938601626132,
0.267734305208461));
#32356=CARTESIAN_POINT('Ctrl Pts',(-0.019274489346019,-0.145319150065199,
0.270385139913496));
#32357=CARTESIAN_POINT('Ctrl Pts',(0.02883137013825,-0.151699698504265,
0.27303597461853));
#32358=CARTESIAN_POINT('Ctrl Pts',(0.0804202103516079,-0.131820469568792,
0.275686809323564));
#32359=CARTESIAN_POINT('Ctrl Pts',(0.11180535579315,-0.0948088800228575,
0.278337644028599));
#32360=CARTESIAN_POINT('Ctrl Pts',(0.143190501234693,-0.0577972904769225,
0.280988478733633));
#32361=CARTESIAN_POINT('Ctrl Pts',(0.154371951904419,-0.00365334032052542,
0.283639313438667));
#32362=CARTESIAN_POINT('Ctrl Pts',(0.14021581852446,0.0427631330787578,
0.286290148143701));
#32363=CARTESIAN_POINT('Ctrl Pts',(0.126059685144501,0.0891796064780407,
0.288940982848735));
#32364=CARTESIAN_POINT('Ctrl Pts',(0.0865659677148572,0.12786860312021,
0.29159181755377));
#32365=CARTESIAN_POINT('Ctrl Pts',(0.0398679459367864,0.141066325542232,
0.294242652258804));
#32366=CARTESIAN_POINT('Ctrl Pts',(-0.00683007584128473,0.154264047964254,
0.296893486963838));
#32367=CARTESIAN_POINT('Ctrl Pts',(-0.0607324019677826,0.141970496166129,
0.299544321668873));
#32368=CARTESIAN_POINT('Ctrl Pts',(-0.0970901351530201,0.109830173318867,
0.302195156373907));
#32369=CARTESIAN_POINT('Ctrl Pts',(-0.127901447813816,0.0825928994431667,
0.304441602721174));
#32370=CARTESIAN_POINT('Ctrl Pts',(-0.14611277332701,0.0411022848956265,
0.306688049068442));
#32371=CARTESIAN_POINT('Ctrl Pts',(-0.146466968003471,-0.000114397412080779,
0.308934495415709));
#32372=CARTESIAN_POINT('Origin',(0.,0.,0.));
#32373=CARTESIAN_POINT('',(-0.146456696168336,0.00011684297731019,0.36606550458429));
#32374=CARTESIAN_POINT('',(-0.146490622007778,0.000105425447882283,0.358934495415709));
#32375=CARTESIAN_POINT('',(-0.14635,-1.79227059055215E-17,0.));
#32376=CARTESIAN_POINT('Ctrl Pts',(-0.146456696168336,0.00011684297731019,
0.36606550458429));
#32377=CARTESIAN_POINT('Ctrl Pts',(-0.146524266643172,0.00787170677865199,
0.365642915871516));
#32378=CARTESIAN_POINT('Ctrl Pts',(-0.145961554618594,0.0156167466990778,
0.365220327158741));
#32379=CARTESIAN_POINT('Ctrl Pts',(-0.14473428578122,0.0232550097723626,
0.364797738445966));
#32380=CARTESIAN_POINT('Ctrl Pts',(-0.137044379852877,0.0711153666076302,
0.362149852873827));
#32381=CARTESIAN_POINT('Ctrl Pts',(-0.103263231798211,0.11478354525948,
0.359501967301688));
#32382=CARTESIAN_POINT('Ctrl Pts',(-0.0588696551343872,0.134250410014218,
0.356854081729549));
#32383=CARTESIAN_POINT('Ctrl Pts',(-0.0144760784705634,0.153717274768956,
0.354206196157409));
#32384=CARTESIAN_POINT('Ctrl Pts',(0.040529926802418,0.148982825626583,
0.35155831058527));
#32385=CARTESIAN_POINT('Ctrl Pts',(0.0809441375650951,0.122216428534895,
0.34891042501313));
#32386=CARTESIAN_POINT('Ctrl Pts',(0.121358348327771,0.0954500314432082,
0.346262539440991));
#32387=CARTESIAN_POINT('Ctrl Pts',(0.147180764580144,0.0466516864022081,
0.343614653868852));
#32388=CARTESIAN_POINT('Ctrl Pts',(0.146579333092572,-0.00181878629327471,
0.340966768296713));
#32389=CARTESIAN_POINT('Ctrl Pts',(0.145977901604999,-0.0502892589887582,
0.338318882724573));
#32390=CARTESIAN_POINT('Ctrl Pts',(0.11895262237748,-0.0984318593387246,
0.335670997152434));
#32391=CARTESIAN_POINT('Ctrl Pts',(0.0778867105927371,-0.124187234331756,
0.333023111580295));
#32392=CARTESIAN_POINT('Ctrl Pts',(0.036820798807994,-0.149942609324788,
0.330375226008155));
#32393=CARTESIAN_POINT('Ctrl Pts',(-0.0182857455339734,-0.153310758960884,
0.327727340436016));
#32394=CARTESIAN_POINT('Ctrl Pts',(-0.062182630799685,-0.132748368261283,
0.325079454863877));
#32395=CARTESIAN_POINT('Ctrl Pts',(-0.106079516065397,-0.112185977561681,
0.322431569291738));
#32396=CARTESIAN_POINT('Ctrl Pts',(-0.138766742254852,-0.0676930465263806,
0.319783683719598));
#32397=CARTESIAN_POINT('Ctrl Pts',(-0.145266741627948,-0.0196566181036479,
0.317135798147459));
#32398=CARTESIAN_POINT('Ctrl Pts',(-0.146142523114734,-0.0131843998326608,
0.316779033626403));
#32399=CARTESIAN_POINT('Ctrl Pts',(-0.14654290982994,-0.00664785401210523,
0.316422269105347));
#32400=CARTESIAN_POINT('Ctrl Pts',(-0.146489966325848,-0.000104789085069334,
0.31606550458429));
#32401=CARTESIAN_POINT('Ctrl Pts',(-0.146466968003471,-0.000114397412080779,
0.308934495415709));
#32402=CARTESIAN_POINT('Ctrl Pts',(-0.146530727462368,-0.00753391423752658,
0.309338883773476));
#32403=CARTESIAN_POINT('Ctrl Pts',(-0.146015835709215,-0.0149445544285316,
0.309743272131243));
#32404=CARTESIAN_POINT('Ctrl Pts',(-0.144891626709003,-0.0222615773186769,
0.31014766048901));
#32405=CARTESIAN_POINT('Ctrl Pts',(-0.137522244835771,-0.0702259112125575,
0.312798495194044));
#32406=CARTESIAN_POINT('Ctrl Pts',(-0.103970340845329,-0.114167485103918,
0.315449329899078));
#32407=CARTESIAN_POINT('Ctrl Pts',(-0.0596410500115333,-0.133910815353779,
0.318100164604112));
#32408=CARTESIAN_POINT('Ctrl Pts',(-0.015311759177738,-0.15365414560364,
0.320750999309147));
#32409=CARTESIAN_POINT('Ctrl Pts',(0.0397949184994109,-0.149199232212,0.323401834014181));
#32410=CARTESIAN_POINT('Ctrl Pts',(0.0803771156598139,-0.122591519257586,
0.326052668719215));
#32411=CARTESIAN_POINT('Ctrl Pts',(0.120959312820217,-0.0959838063031723,
0.32870350342425));
#32412=CARTESIAN_POINT('Ctrl Pts',(0.147017029463874,-0.0472232937859833,
0.331354338129284));
#32413=CARTESIAN_POINT('Ctrl Pts',(0.146586036983397,0.00130195078264539,
0.334005172834318));
#32414=CARTESIAN_POINT('Ctrl Pts',(0.146155044502921,0.0498271953512744,
0.336656007539352));
#32415=CARTESIAN_POINT('Ctrl Pts',(0.119235342898311,0.0981171719713431,
0.339306842244386));
#32416=CARTESIAN_POINT('Ctrl Pts',(0.0781869354735432,0.123999856599104,
0.341957676949421));
#32417=CARTESIAN_POINT('Ctrl Pts',(0.0371385280487761,0.149882541226865,
0.344608511654455));
#32418=CARTESIAN_POINT('Ctrl Pts',(-0.0180385851961482,0.153357933862318,
0.347259346359489));
#32419=CARTESIAN_POINT('Ctrl Pts',(-0.0620101968435835,0.132830330894432,
0.349910181064524));
#32420=CARTESIAN_POINT('Ctrl Pts',(-0.105981808491019,0.112302727926544,
0.352561015769558));
#32421=CARTESIAN_POINT('Ctrl Pts',(-0.138747918540966,0.0677721293553162,
0.355211850474592));
#32422=CARTESIAN_POINT('Ctrl Pts',(-0.145264183888347,0.0196844656531965,
0.357862685179626));
#32423=CARTESIAN_POINT('Ctrl Pts',(-0.146142422968675,0.0132033812753397,
0.358219955258321));
#32424=CARTESIAN_POINT('Ctrl Pts',(-0.146543841751789,0.00665768391130569,
0.358577225337015));
#32425=CARTESIAN_POINT('Ctrl Pts',(-0.146490622007778,0.000105425447882283,
0.358934495415709));
#32426=CARTESIAN_POINT('Origin',(0.,0.,0.));
#32427=CARTESIAN_POINT('',(-0.146117527463381,3.66422859593568E-5,0.416065504584291));
#32428=CARTESIAN_POINT('',(-0.146131941026353,6.08514395597815E-5,0.408934495415709));
#32429=CARTESIAN_POINT('',(-0.14635,-1.79227059055215E-17,0.));
#32430=CARTESIAN_POINT('Ctrl Pts',(-0.146117527463381,3.66422859593568E-5,
0.416065504584291));
#32431=CARTESIAN_POINT('Ctrl Pts',(-0.146167164015074,0.0222235765819606,
0.414863562637685));
#32432=CARTESIAN_POINT('Ctrl Pts',(-0.141430069804178,0.0443904018142415,
0.413661620691079));
#32433=CARTESIAN_POINT('Ctrl Pts',(-0.131797444393702,0.0641735569006793,
0.412459678744474));
#32434=CARTESIAN_POINT('Ctrl Pts',(-0.11057671079816,0.107755970404684,
0.409811793172335));
#32435=CARTESIAN_POINT('Ctrl Pts',(-0.0655968071821861,0.139769869286095,
0.407163907600195));
#32436=CARTESIAN_POINT('Ctrl Pts',(-0.0174679796227892,0.145546147336919,
0.404516022028056));
#32437=CARTESIAN_POINT('Ctrl Pts',(0.0306608479366084,0.151322425387742,
0.401868136455917));
#32438=CARTESIAN_POINT('Ctrl Pts',(0.0819385994394289,0.130861082607978,
0.399220250883777));
#32439=CARTESIAN_POINT('Ctrl Pts',(0.112869404704651,0.0935377150207321,
0.396572365311638));
#32440=CARTESIAN_POINT('Ctrl Pts',(0.143800209969873,0.0562143474334866,
0.393924479739499));
#32441=CARTESIAN_POINT('Ctrl Pts',(0.154384068997497,0.00202895503876042,
0.391276594167359));
#32442=CARTESIAN_POINT('Ctrl Pts',(0.139771347867625,-0.0441902675604103,
0.38862870859522));
#32443=CARTESIAN_POINT('Ctrl Pts',(0.125158626737753,-0.0904094901595803,
0.385980823023081));
#32444=CARTESIAN_POINT('Ctrl Pts',(0.0853493254503865,-0.128662542963195,
0.383332937450942));
#32445=CARTESIAN_POINT('Ctrl Pts',(0.0385844175605987,-0.141421539587247,
0.380685051878802));
#32446=CARTESIAN_POINT('Ctrl Pts',(-0.00818049032918902,-0.154180536211298,
0.378037166306663));
#32447=CARTESIAN_POINT('Ctrl Pts',(-0.0619010048213979,-0.141445476655787,
0.375389280734523));
#32448=CARTESIAN_POINT('Ctrl Pts',(-0.0979619301664915,-0.109051679368689,
0.372741395162384));
#32449=CARTESIAN_POINT('Ctrl Pts',(-0.128267720099621,-0.081827763001475,
0.370516098303019));
#32450=CARTESIAN_POINT('Ctrl Pts',(-0.146100878890467,-0.0407192549596569,
0.368290801443655));
#32451=CARTESIAN_POINT('Ctrl Pts',(-0.146456696168336,0.00011684297731019,
0.36606550458429));
#32452=CARTESIAN_POINT('Ctrl Pts',(-0.146490622007778,0.000105425447882283,
0.358934495415709));
#32453=CARTESIAN_POINT('Ctrl Pts',(-0.146148967529651,-0.0419580697355662,
0.361228060042049));
#32454=CARTESIAN_POINT('Ctrl Pts',(-0.12707053516474,-0.0842919640484707,
0.363521624668389));
#32455=CARTESIAN_POINT('Ctrl Pts',(-0.0951239884102214,-0.111537384525928,
0.365815189294729));
#32456=CARTESIAN_POINT('Ctrl Pts',(-0.0582011069398996,-0.143026842169921,
0.368466023999764));
#32457=CARTESIAN_POINT('Ctrl Pts',(-0.00408892335444046,-0.154361028624896,
0.371116858704798));
#32458=CARTESIAN_POINT('Ctrl Pts',(0.0423673101370894,-0.140335926848737,
0.373767693409832));
#32459=CARTESIAN_POINT('Ctrl Pts',(0.0888235436286192,-0.126310825072579,
0.376418528114866));
#32460=CARTESIAN_POINT('Ctrl Pts',(0.12762382702622,-0.0869264350652862,
0.379069362819901));
#32461=CARTESIAN_POINT('Ctrl Pts',(0.140953266768128,-0.0402658398230972,
0.381720197524935));
#32462=CARTESIAN_POINT('Ctrl Pts',(0.154282706510036,0.00639475541909176,
0.384371032229969));
#32463=CARTESIAN_POINT('Ctrl Pts',(0.142141302596253,0.0603315558961778,
0.387021866935004));
#32464=CARTESIAN_POINT('Ctrl Pts',(0.110103699587577,0.0967798361409283,
0.389672701640038));
#32465=CARTESIAN_POINT('Ctrl Pts',(0.0780660965789003,0.133228116385679,
0.392323536345072));
#32466=CARTESIAN_POINT('Ctrl Pts',(0.0261322944753315,0.152187876398094,
0.394974371050106));
#32467=CARTESIAN_POINT('Ctrl Pts',(-0.0218526425106493,0.144953866566232,
0.397625205755141));
#32468=CARTESIAN_POINT('Ctrl Pts',(-0.0698375794966294,0.13771985673437,
0.400276040460175));
#32469=CARTESIAN_POINT('Ctrl Pts',(-0.113873651365021,0.104292077058233,
0.402926875165209));
#32470=CARTESIAN_POINT('Ctrl Pts',(-0.133741989653421,0.0600186737328441,
0.405577709870243));
#32471=CARTESIAN_POINT('Ctrl Pts',(-0.142128499086628,0.0413306833614836,
0.406696638385399));
#32472=CARTESIAN_POINT('Ctrl Pts',(-0.14620899575881,0.0207103068323409,
0.407815566900554));
#32473=CARTESIAN_POINT('Ctrl Pts',(-0.146131941026353,6.08514395597814E-5,
0.408934495415709));
#32474=CARTESIAN_POINT('Origin',(0.,0.,0.));
#32475=CARTESIAN_POINT('',(-0.146320034481408,-0.000132042578932776,0.466065504584291));
#32476=CARTESIAN_POINT('',(-0.146267142220666,-0.000128791573925899,0.458934495415709));
#32477=CARTESIAN_POINT('',(-0.14635,-1.79227059055215E-17,0.));
#32478=CARTESIAN_POINT('Ctrl Pts',(-0.146320034481408,-0.000132042578932776,
0.466065504584291));
#32479=CARTESIAN_POINT('Ctrl Pts',(-0.145990955376697,0.0363120653110472,
0.464084209403854));
#32480=CARTESIAN_POINT('Ctrl Pts',(-0.132207444595406,0.0729769481781354,
0.462102914223418));
#32481=CARTESIAN_POINT('Ctrl Pts',(-0.107565849799547,0.0995912952759384,
0.460121619042982));
#32482=CARTESIAN_POINT('Ctrl Pts',(-0.074633794052009,0.135159819536245,
0.457473733470842));
#32483=CARTESIAN_POINT('Ctrl Pts',(-0.0223083694375825,0.15277731788608,
0.454825847898703));
#32484=CARTESIAN_POINT('Ctrl Pts',(0.0254312589463019,0.144368338990174,
0.452177962326564));
#32485=CARTESIAN_POINT('Ctrl Pts',(0.0731708873301868,0.135959360094269,
0.449530076754424));
#32486=CARTESIAN_POINT('Ctrl Pts',(0.116324719483529,0.101523903952622,
0.446882191182285));
#32487=CARTESIAN_POINT('Ctrl Pts',(0.13512098610947,0.0568421509649556,
0.444234305610146));
#32488=CARTESIAN_POINT('Ctrl Pts',(0.153917252735412,0.0121603979772891,
0.441586420038006));
#32489=CARTESIAN_POINT('Ctrl Pts',(0.148355953833953,-0.0427676518563976,
0.438938534465867));
#32490=CARTESIAN_POINT('Ctrl Pts',(0.120984436568095,-0.0827743147100686,
0.436290648893728));
#32491=CARTESIAN_POINT('Ctrl Pts',(0.0936129193022383,-0.122780977563739,
0.433642763321588));
#32492=CARTESIAN_POINT('Ctrl Pts',(0.044431183671984,-0.147866253437395,
0.430994877749449));
#32493=CARTESIAN_POINT('Ctrl Pts',(-0.0040248096733416,-0.146535421965135,
0.42834699217731));
#32494=CARTESIAN_POINT('Ctrl Pts',(-0.0524808030186669,-0.145204590492875,
0.425699106605171));
#32495=CARTESIAN_POINT('Ctrl Pts',(-0.100211054079063,-0.117457651674699,
0.423051221033031));
#32496=CARTESIAN_POINT('Ctrl Pts',(-0.125345397821707,-0.0760087182023128,
0.420403335460892));
#32497=CARTESIAN_POINT('Ctrl Pts',(-0.139070629946179,-0.0533744994995956,
0.418957391835358));
#32498=CARTESIAN_POINT('Ctrl Pts',(-0.146057814383464,-0.0266543774475973,
0.417511448209824));
#32499=CARTESIAN_POINT('Ctrl Pts',(-0.146117527463381,3.66422859593568E-5,
0.416065504584291));
#32500=CARTESIAN_POINT('Ctrl Pts',(-0.146131941026353,6.08514395597814E-5,
0.408934495415709));
#32501=CARTESIAN_POINT('Ctrl Pts',(-0.146026446689573,-0.0282099702486701,
0.410466401605588));
#32502=CARTESIAN_POINT('Ctrl Pts',(-0.138128084958642,-0.0565352970304639,
0.411998307795467));
#32503=CARTESIAN_POINT('Ctrl Pts',(-0.122817836477901,-0.0800308731172956,
0.413530213985346));
#32504=CARTESIAN_POINT('Ctrl Pts',(-0.0963247403055724,-0.120687989667408,
0.41618104869038));
#32505=CARTESIAN_POINT('Ctrl Pts',(-0.0476379432525075,-0.146883195792991,
0.418831883395415));
#32506=CARTESIAN_POINT('Ctrl Pts',(0.000888321221429993,-0.146589129065305,
0.421482718100449));
#32507=CARTESIAN_POINT('Ctrl Pts',(0.0494145856953668,-0.146295062337618,
0.424133552805483));
#32508=CARTESIAN_POINT('Ctrl Pts',(0.097780317590176,-0.119511722756663,
0.426784387510517));
#32509=CARTESIAN_POINT('Ctrl Pts',(0.123778732978107,-0.0785365161302261,
0.429435222215552));
#32510=CARTESIAN_POINT('Ctrl Pts',(0.149777148366038,-0.0375613095037888,
0.432086056920586));
#32511=CARTESIAN_POINT('Ctrl Pts',(0.15340824724709,0.0176057641681304,
0.43473689162562));
#32512=CARTESIAN_POINT('Ctrl Pts',(0.13300479146532,0.0616351303104708,
0.437387726330655));
#32513=CARTESIAN_POINT('Ctrl Pts',(0.112601335683551,0.105664496452811,
0.440038561035689));
#32514=CARTESIAN_POINT('Ctrl Pts',(0.0681633252389606,0.138556155065572,
0.442689395740723));
#32515=CARTESIAN_POINT('Ctrl Pts',(0.0200942611983476,0.145208074081285,
0.445340230445757));
#32516=CARTESIAN_POINT('Ctrl Pts',(-0.0279748028422658,0.151859993096997,
0.447991065150791));
#32517=CARTESIAN_POINT('Ctrl Pts',(-0.0796749204789013,0.132272172515661,
0.450641899855826));
#32518=CARTESIAN_POINT('Ctrl Pts',(-0.111268479500082,0.095438314693151,
0.45329273456086));
#32519=CARTESIAN_POINT('Ctrl Pts',(-0.133681961086661,0.0693071974766942,
0.455173321512477));
#32520=CARTESIAN_POINT('Ctrl Pts',(-0.145975937294016,0.0344962574238126,
0.457053908464093));
#32521=CARTESIAN_POINT('Ctrl Pts',(-0.146267142220666,-0.000128791573925899,
0.458934495415709));
#32522=CARTESIAN_POINT('Origin',(0.,0.,-0.0924367114736154));
#32523=CARTESIAN_POINT('',(-0.117750885282186,-0.00010626111879085,0.482563288526385));
#32524=CARTESIAN_POINT('',(-0.117972864089022,-5.93608753193428E-7,0.492436711473616));
#32525=CARTESIAN_POINT('',(-0.117775,-8.88924268665971E-15,-0.0924367114736154));
#32526=CARTESIAN_POINT('',(-0.117668597464311,0.00500517689817391,0.532225000000001));
#32527=CARTESIAN_POINT('Ctrl Pts',(-0.117750885282186,-0.000106261118790843,
0.482563288526385));
#32528=CARTESIAN_POINT('Ctrl Pts',(-0.117839983816431,-0.00997354393438475,
0.483229878918088));
#32529=CARTESIAN_POINT('Ctrl Pts',(-0.112189023051801,-0.0589364681957879,
0.486544354881929));
#32530=CARTESIAN_POINT('Ctrl Pts',(-0.0439766578214066,-0.132120623957634,
0.492506716417911));
#32531=CARTESIAN_POINT('Ctrl Pts',(0.087240331747497,-0.108512430051717,
0.500450373134329));
#32532=CARTESIAN_POINT('Ctrl Pts',(0.138438921804208,0.0144739368962113,
0.508394029850746));
#32533=CARTESIAN_POINT('Ctrl Pts',(0.0629040591690992,0.12431971381125,
0.516337686567165));
#32534=CARTESIAN_POINT('Ctrl Pts',(-0.0705459363093062,0.119993110375402,
0.524281343283582));
#32535=CARTESIAN_POINT('Ctrl Pts',(-0.116003159314893,0.0441585924901374,
0.529577114427861));
#32536=CARTESIAN_POINT('Ctrl Pts',(-0.117668597464311,0.00500517689817385,
0.532225));
#32537=CARTESIAN_POINT('',(-0.0334019664626897,0.112939183906319,0.532225000000001));
#32538=CARTESIAN_POINT('Origin',(0.,0.,0.532225));
#32539=CARTESIAN_POINT('Ctrl Pts',(-0.117972864533492,-5.93610086620396E-7,
0.492436711473617));
#32540=CARTESIAN_POINT('Ctrl Pts',(-0.117972892941239,-0.000127136793190444,
0.492445300790573));
#32541=CARTESIAN_POINT('Ctrl Pts',(-0.117912463615216,-0.0393074137896712,
0.495104724812564));
#32542=CARTESIAN_POINT('Ctrl Pts',(-0.0749307309976486,-0.117412744486246,
0.500414983539588));
#32543=CARTESIAN_POINT('Ctrl Pts',(0.0581614397283287,-0.126517333775439,
0.508367487654693));
#32544=CARTESIAN_POINT('Ctrl Pts',(0.138005962114904,-0.01953005209576,
0.516319991769794));
#32545=CARTESIAN_POINT('Ctrl Pts',(0.0908022345067483,0.105567300931769,
0.524272495884898));
#32546=CARTESIAN_POINT('Ctrl Pts',(0.00421962447768953,0.124065836989857,
0.529574165294966));
#32547=CARTESIAN_POINT('Ctrl Pts',(-0.0334019664626881,0.11293918390632,
0.532225));
#32548=CARTESIAN_POINT('Origin',(0.,0.,-0.0924367114736154));
#32549=CARTESIAN_POINT('',(-0.117587917984282,2.94878389348885E-5,0.432563288526385));
#32550=CARTESIAN_POINT('',(-0.117708320294082,-0.000103644876124687,0.442436711473616));
#32551=CARTESIAN_POINT('',(-0.117775,-8.88924268665971E-15,-0.0924367114736154));
#32552=CARTESIAN_POINT('Ctrl Pts',(-0.117587917984282,2.94878389348868E-5,
0.432563288526385));
#32553=CARTESIAN_POINT('Ctrl Pts',(-0.117539863949521,-0.0214500806552194,
0.434009232151918));
#32554=CARTESIAN_POINT('Ctrl Pts',(-0.101619941365326,-0.082330436444606,
0.438103061349591));
#32555=CARTESIAN_POINT('Ctrl Pts',(-0.00382300141363195,-0.139182551176009,
0.444844776119403));
#32556=CARTESIAN_POINT('Ctrl Pts',(0.11491384000461,-0.0786205074584852,
0.452788432835821));
#32557=CARTESIAN_POINT('Ctrl Pts',(0.128340187352459,0.0539893538840985,
0.460732089552239));
#32558=CARTESIAN_POINT('Ctrl Pts',(0.024156191824071,0.137125039167645,
0.468675746268657));
#32559=CARTESIAN_POINT('Ctrl Pts',(-0.0915696283436722,0.0981611996792526,
0.475952812593373));
#32560=CARTESIAN_POINT('Ctrl Pts',(-0.117486059238065,0.0292220942398885,
0.480581993345948));
#32561=CARTESIAN_POINT('Ctrl Pts',(-0.117750885282186,-0.000106261118790843,
0.482563288526385));
#32562=CARTESIAN_POINT('Ctrl Pts',(-0.117708320294082,-0.000103644876124676,
0.442436711473616));
#32563=CARTESIAN_POINT('Ctrl Pts',(-0.117804303693274,-0.0115163291952777,
0.443206959227034));
#32564=CARTESIAN_POINT('Ctrl Pts',(-0.111033657777347,-0.0620947057757177,
0.446628041685486));
#32565=CARTESIAN_POINT('Ctrl Pts',(-0.038636663810782,-0.133821400192823,
0.452699958848972));
#32566=CARTESIAN_POINT('Ctrl Pts',(0.0916608011058181,-0.104875817685159,
0.460652462964076));
#32567=CARTESIAN_POINT('Ctrl Pts',(0.137790741908166,0.0203740232160909,
0.468604967079177));
#32568=CARTESIAN_POINT('Ctrl Pts',(0.0573828398023632,0.126918127906013,
0.476557471194281));
#32569=CARTESIAN_POINT('Ctrl Pts',(-0.0755630108222985,0.116919225220885,
0.484501385992427));
#32570=CARTESIAN_POINT('Ctrl Pts',(-0.117964125743295,0.0389266160426656,
0.489794466085539));
#32571=CARTESIAN_POINT('Ctrl Pts',(-0.117972864533492,-5.93610086620396E-7,
0.492436711473617));
#32572=CARTESIAN_POINT('Origin',(0.,0.,-0.0924367114736154));
#32573=CARTESIAN_POINT('',(-0.117860863622998,9.40292562467743E-5,0.382563288526384));
#32574=CARTESIAN_POINT('',(-0.11759951728308,4.89701284099239E-5,0.392436711473616));
#32575=CARTESIAN_POINT('',(-0.117775,-8.88924268665971E-15,-0.0924367114736154));
#32576=CARTESIAN_POINT('Ctrl Pts',(-0.117860863622998,9.40292562467788E-5,
0.382563288526384));
#32577=CARTESIAN_POINT('Ctrl Pts',(-0.117574520063714,-0.0327687752160871,
0.384788585385749));
#32578=CARTESIAN_POINT('Ctrl Pts',(-0.0861467637051906,-0.105215176336211,
0.389661767817253));
#32579=CARTESIAN_POINT('Ctrl Pts',(0.0366482838797405,-0.134325140358292,
0.397182835820896));
#32580=CARTESIAN_POINT('Ctrl Pts',(0.132757756905765,-0.0419728350502109,
0.405126492537314));
#32581=CARTESIAN_POINT('Ctrl Pts',(0.107205710503746,0.0888440680441954,
0.413070149253731));
#32582=CARTESIAN_POINT('Ctrl Pts',(-0.0165914302528927,0.138242796692368,
0.42101380597015));
#32583=CARTESIAN_POINT('Ctrl Pts',(-0.105417454577164,0.0750219551131263,
0.427511519061034));
#32584=CARTESIAN_POINT('Ctrl Pts',(-0.117627862944144,0.0178843985783384,
0.431361346579779));
#32585=CARTESIAN_POINT('Ctrl Pts',(-0.117587917984282,2.94878389348868E-5,
0.432563288526385));
#32586=CARTESIAN_POINT('Ctrl Pts',(-0.11759951728308,4.89701284099274E-5,
0.392436711473616));
#32587=CARTESIAN_POINT('Ctrl Pts',(-0.11751462083269,-0.0227019422346301,
0.393968617663495));
#32588=CARTESIAN_POINT('Ctrl Pts',(-0.100159557717256,-0.0849411572528722,
0.398151358558408));
#32589=CARTESIAN_POINT('Ctrl Pts',(0.000844063931402275,-0.139284651766041,
0.404984934158356));
#32590=CARTESIAN_POINT('Ctrl Pts',(0.117610871049501,-0.0746230633995127,
0.412937438273457));
#32591=CARTESIAN_POINT('Ctrl Pts',(0.126377239427685,0.0585638604483229,
0.420889942388562));
#32592=CARTESIAN_POINT('Ctrl Pts',(0.0190929207373193,0.137972437690235,
0.428842446503664));
#32593=CARTESIAN_POINT('Ctrl Pts',(-0.0936346562739906,0.0952629110198009,
0.436024702865349));
#32594=CARTESIAN_POINT('Ctrl Pts',(-0.117473973452704,0.0277608248588199,
0.440556124522));
#32595=CARTESIAN_POINT('Ctrl Pts',(-0.117708320294082,-0.000103644876124676,
0.442436711473616));
#32596=CARTESIAN_POINT('Origin',(0.,0.,-0.0924367114736154));
#32597=CARTESIAN_POINT('',(-0.117887637745315,-8.43288998643762E-5,0.332563288526385));
#32598=CARTESIAN_POINT('',(-0.11788816540462,8.48410121138156E-5,0.342436711473616));
#32599=CARTESIAN_POINT('',(-0.117775,-8.88924268665971E-15,-0.0924367114736154));
#32600=CARTESIAN_POINT('Ctrl Pts',(-0.117887637745315,-8.43288998643547E-5,
0.332563288526385));
#32601=CARTESIAN_POINT('Ctrl Pts',(-0.117930243971446,-0.00534985313478999,
0.332920053047441));
#32602=CARTESIAN_POINT('Ctrl Pts',(-0.115216603610867,-0.0496516091215746,
0.335924703140636));
#32603=CARTESIAN_POINT('Ctrl Pts',(-0.0590623637863932,-0.126087177724698,
0.34157723880597));
#32604=CARTESIAN_POINT('Ctrl Pts',(0.0739784273282333,-0.117955633685244,
0.349520895522388));
#32605=CARTESIAN_POINT('Ctrl Pts',(0.139224117680559,-0.00172752115601949,
0.357464552238807));
#32606=CARTESIAN_POINT('Ctrl Pts',(0.0768824352591712,0.11608372080921,
0.365408208955224));
#32607=CARTESIAN_POINT('Ctrl Pts',(-0.0559156297430559,0.12751384888047,
0.373351865671643));
#32608=CARTESIAN_POINT('Ctrl Pts',(-0.114624951070718,0.0516215456314347,
0.379070225528695));
#32609=CARTESIAN_POINT('Ctrl Pts',(-0.117915240887596,0.00633474728975054,
0.382140699813609));
#32610=CARTESIAN_POINT('Ctrl Pts',(-0.117860863622998,9.40292562467788E-5,
0.382563288526384));
#32611=CARTESIAN_POINT('Ctrl Pts',(-0.11788816540462,8.4841012113826E-5,
0.342436711473616));
#32612=CARTESIAN_POINT('Ctrl Pts',(-0.1176132193427,-0.0337657100314819,
0.344730276099956));
#32613=CARTESIAN_POINT('Ctrl Pts',(-0.0845149237619996,-0.107208837865588,
0.34967467543133));
#32614=CARTESIAN_POINT('Ctrl Pts',(0.0402561631274929,-0.133343040355529,
0.357269909467738));
#32615=CARTESIAN_POINT('Ctrl Pts',(0.133929618074243,-0.0382594079720193,
0.365222413582842));
#32616=CARTESIAN_POINT('Ctrl Pts',(0.104617274119081,0.0919573329132998,
0.373174917697944));
#32617=CARTESIAN_POINT('Ctrl Pts',(-0.020763734615072,0.137730870367254,
0.381127421813047));
#32618=CARTESIAN_POINT('Ctrl Pts',(-0.106598215372521,0.0725739208566139,
0.387548019738271));
#32619=CARTESIAN_POINT('Ctrl Pts',(-0.117661526993468,0.0166665964275914,
0.391317782958461));
#32620=CARTESIAN_POINT('Ctrl Pts',(-0.11759951728308,4.89701284099274E-5,
0.392436711473616));
#32621=CARTESIAN_POINT('Origin',(0.,0.,-0.0924367114736154));
#32622=CARTESIAN_POINT('',(-0.117597135791184,-4.46042773137295E-5,0.282563288526384));
#32623=CARTESIAN_POINT('',(-0.117869129870917,-9.20611903598989E-5,0.292436711473616));
#32624=CARTESIAN_POINT('',(-0.117775,-8.88924268665971E-15,-0.0924367114736154));
#32625=CARTESIAN_POINT('Ctrl Pts',(-0.117597135791184,-4.46042773137294E-5,
0.282563288526384));
#32626=CARTESIAN_POINT('Ctrl Pts',(-0.117654518243026,-0.0169184081852861,
0.283699406281271));
#32627=CARTESIAN_POINT('Ctrl Pts',(-0.106362773508523,-0.0730457989372372,
0.287483409608297));
#32628=CARTESIAN_POINT('Ctrl Pts',(-0.0200165152988323,-0.137788527592198,
0.293915298507463));
#32629=CARTESIAN_POINT('Ctrl Pts',(0.104968269293632,-0.0914767820950745,
0.301858955223881));
#32630=CARTESIAN_POINT('Ctrl Pts',(0.133758329466478,0.0386658573002006,
0.309802611940298));
#32631=CARTESIAN_POINT('Ctrl Pts',(0.0399699596916912,0.133374441107753,
0.317746268656717));
#32632=CARTESIAN_POINT('Ctrl Pts',(-0.084590271720082,0.107092283864913,
0.325333160852078));
#32633=CARTESIAN_POINT('Ctrl Pts',(-0.117614023033548,0.0337305621770822,
0.330272167475301));
#32634=CARTESIAN_POINT('Ctrl Pts',(-0.117887637745315,-8.43288998643547E-5,
0.332563288526385));
#32635=CARTESIAN_POINT('Ctrl Pts',(-0.117869129870917,-9.2061190359885E-5,
0.292436711473616));
#32636=CARTESIAN_POINT('Ctrl Pts',(-0.117920440224669,-0.00606290911736031,
0.292841099831383));
#32637=CARTESIAN_POINT('Ctrl Pts',(-0.114789890532149,-0.0511197142210238,
0.295896322894184));
#32638=CARTESIAN_POINT('Ctrl Pts',(-0.0566691588697243,-0.127238089669758,
0.301602380662019));
#32639=CARTESIAN_POINT('Ctrl Pts',(0.0763719541489209,-0.116482829853556,
0.309554884777122));
#32640=CARTESIAN_POINT('Ctrl Pts',(0.139281709756163,0.00123707506708643,
0.317507388892225));
#32641=CARTESIAN_POINT('Ctrl Pts',(0.0742909098282569,0.117820990265484,
0.325459893007327));
#32642=CARTESIAN_POINT('Ctrl Pts',(-0.0589202520252667,0.1262114453589,
0.33341239712243));
#32643=CARTESIAN_POINT('Ctrl Pts',(-0.115211084829427,0.0497097039247984,
0.339071336611193));
#32644=CARTESIAN_POINT('Ctrl Pts',(-0.11793099393452,0.00535776373524371,
0.342079441394922));
#32645=CARTESIAN_POINT('Ctrl Pts',(-0.11788816540462,8.4841012113826E-5,
0.342436711473616));
#32646=CARTESIAN_POINT('Origin',(0.,0.,-0.0924367114736154));
#32647=CARTESIAN_POINT('',(-0.117724026649356,0.00010549178999148,0.232563288526384));
#32648=CARTESIAN_POINT('',(-0.117591763024586,-3.83449468523145E-5,0.242436711473616));
#32649=CARTESIAN_POINT('',(-0.117775,-8.88924268665971E-15,-0.0924367114736154));
#32650=CARTESIAN_POINT('Ctrl Pts',(-0.117724026649356,0.000105491789991495,
0.232563288526384));
#32651=CARTESIAN_POINT('Ctrl Pts',(-0.117478226080151,-0.0282662610808501,
0.234478759515102));
#32652=CARTESIAN_POINT('Ctrl Pts',(-0.0929369215417509,-0.0962395631396471,
0.239042116075959));
#32653=CARTESIAN_POINT('Ctrl Pts',(0.0207448421498254,-0.137680756627218,
0.246253358208955));
#32654=CARTESIAN_POINT('Ctrl Pts',(0.126961839902422,-0.0571579428392388,
0.254197014925373));
#32655=CARTESIAN_POINT('Ctrl Pts',(0.116828827462796,0.075745391244066,
0.262140671641791));
#32656=CARTESIAN_POINT('Ctrl Pts',(-0.000368128572008151,0.139234348141551,
0.270084328358209));
#32657=CARTESIAN_POINT('Ctrl Pts',(-0.100514230788311,0.0842953826634335,
0.27689186731974));
#32658=CARTESIAN_POINT('Ctrl Pts',(-0.117520780198996,0.0224084148687892,
0.281051520709132));
#32659=CARTESIAN_POINT('Ctrl Pts',(-0.117597135791184,-4.46042773137294E-5,
0.282563288526384));
#32660=CARTESIAN_POINT('Ctrl Pts',(-0.117591763024586,-3.83449468523075E-5,
0.242436711473616));
#32661=CARTESIAN_POINT('Ctrl Pts',(-0.117642174491994,-0.017358594045656,
0.243602758267844));
#32662=CARTESIAN_POINT('Ctrl Pts',(-0.10593062496396,-0.0739889980249599,
0.247419639767106));
#32663=CARTESIAN_POINT('Ctrl Pts',(-0.0183140487741412,-0.138077951344142,
0.253887355971402));
#32664=CARTESIAN_POINT('Ctrl Pts',(0.106234136865658,-0.0900845891054932,
0.261839860086505));
#32665=CARTESIAN_POINT('Ctrl Pts',(0.133228916899009,0.040632262203075,
0.269792364201608));
#32666=CARTESIAN_POINT('Ctrl Pts',(0.0378813411502606,0.134037043471229,
0.27774486831671));
#32667=CARTESIAN_POINT('Ctrl Pts',(-0.085634823441202,0.105866601183683,
0.285292984074047));
#32668=CARTESIAN_POINT('Ctrl Pts',(-0.117584092098319,0.0330770181317487,
0.290190265126349));
#32669=CARTESIAN_POINT('Ctrl Pts',(-0.117869129870917,-9.2061190359885E-5,
0.292436711473616));
#32670=CARTESIAN_POINT('Origin',(0.,0.,-0.0924367114736154));
#32671=CARTESIAN_POINT('',(-0.117966882359366,-1.29211934964908E-5,0.182563288526384));
#32672=CARTESIAN_POINT('',(-0.117728105208174,0.000106637828744482,0.192436711473616));
#32673=CARTESIAN_POINT('',(-0.117775,-8.88924268665971E-15,-0.0924367114736154));
#32674=CARTESIAN_POINT('Ctrl Pts',(-0.117966882359366,-1.29211934964912E-5,
0.182563288526384));
#32675=CARTESIAN_POINT('Ctrl Pts',(-0.117967957119725,-0.000704465266726215,
0.182610227176794));
#32676=CARTESIAN_POINT('Ctrl Pts',(-0.117649070375187,-0.0404061166150831,
0.185305051399342));
#32677=CARTESIAN_POINT('Ctrl Pts',(-0.0733536600413758,-0.118345172107485,
0.19064776119403));
#32678=CARTESIAN_POINT('Ctrl Pts',(0.0597282696676458,-0.12577310138558,
0.198591417910448));
#32679=CARTESIAN_POINT('Ctrl Pts',(0.138074187460599,-0.0179404007303906,
0.206535074626866));
#32680=CARTESIAN_POINT('Ctrl Pts',(0.0898865489335327,0.106333191146418,
0.214478731343283));
#32681=CARTESIAN_POINT('Ctrl Pts',(-0.0406746665030564,0.133161220808791,
0.222422388059702));
#32682=CARTESIAN_POINT('Ctrl Pts',(-0.111466604862902,0.0609145729578186,
0.228450573787402));
#32683=CARTESIAN_POINT('Ctrl Pts',(-0.117818012892196,0.0109539388206346,
0.231830873942963));
#32684=CARTESIAN_POINT('Ctrl Pts',(-0.117724026649356,0.000105491789991495,
0.232563288526384));
#32685=CARTESIAN_POINT('Ctrl Pts',(-0.117728105208174,0.000106637828744488,
0.192436711473616));
#32686=CARTESIAN_POINT('Ctrl Pts',(-0.11747787316262,-0.0284437724366353,
0.194364416704305));
#32687=CARTESIAN_POINT('Ctrl Pts',(-0.0926723165398222,-0.0966441001570621,
0.198942956640028));
#32688=CARTESIAN_POINT('Ctrl Pts',(0.0215406810767683,-0.137611496939632,
0.206172331280785));
#32689=CARTESIAN_POINT('Ctrl Pts',(0.127397488829925,-0.056309900280862,
0.214124835395888));
#32690=CARTESIAN_POINT('Ctrl Pts',(0.116266864218555,0.0767003345124148,
0.222077339510991));
#32691=CARTESIAN_POINT('Ctrl Pts',(-0.0016300870944122,0.139277664563073,
0.230029843626094));
#32692=CARTESIAN_POINT('Ctrl Pts',(-0.100962832358778,0.0835357163242542,
0.236816300946969));
#32693=CARTESIAN_POINT('Ctrl Pts',(-0.117527571486354,0.0220164272984534,
0.240951923562809));
#32694=CARTESIAN_POINT('Ctrl Pts',(-0.117591763024586,-3.83449468523075E-5,
0.242436711473616));
#32695=CARTESIAN_POINT('Origin',(0.,0.,-0.0924367114736154));
#32696=CARTESIAN_POINT('',(-0.117685857408994,-9.79219620674319E-5,0.132563288526384));
#32697=CARTESIAN_POINT('',(-0.117968412270431,-1.06668654225733E-5,0.142436711473616));
#32698=CARTESIAN_POINT('',(-0.117775,-8.88924268665971E-15,-0.0924367114736154));
#32699=CARTESIAN_POINT('Ctrl Pts',(-0.117685857408994,-9.79219620674231E-5,
0.132563288526384));
#32700=CARTESIAN_POINT('Ctrl Pts',(-0.117781952389543,-0.0123469217649596,
0.133389580410625));
#32701=CARTESIAN_POINT('Ctrl Pts',(-0.110383000729775,-0.063735125339128,
0.136863757867004));
#32702=CARTESIAN_POINT('Ctrl Pts',(-0.03593748288359,-0.134517045800752,
0.142985820895522));
#32703=CARTESIAN_POINT('Ctrl Pts',(0.0935927050428541,-0.103086105216301,
0.150929477611941));
#32704=CARTESIAN_POINT('Ctrl Pts',(0.137352931996012,0.0228147184504364,
0.158873134328358));
#32705=CARTESIAN_POINT('Ctrl Pts',(0.0552405729858772,0.127807739141585,
0.166816791044776));
#32706=CARTESIAN_POINT('Ctrl Pts',(-0.0767108666901454,0.115747243191764,
0.174713509110785));
#32707=CARTESIAN_POINT('Ctrl Pts',(-0.117907328140755,0.0383066600647174,
0.179962341604654));
#32708=CARTESIAN_POINT('Ctrl Pts',(-0.117966882359366,-1.29211934964912E-5,
0.182563288526384));
#32709=CARTESIAN_POINT('Ctrl Pts',(-0.117968412270431,-1.06668654225827E-5,
0.142436711473616));
#32710=CARTESIAN_POINT('Ctrl Pts',(-0.117969144731522,-0.000578292161741028,
0.142475240435732));
#32711=CARTESIAN_POINT('Ctrl Pts',(-0.117707998838203,-0.0401984655398319,
0.145164604102881));
#32712=CARTESIAN_POINT('Ctrl Pts',(-0.0736248085349355,-0.118238371369349,
0.150504802475065));
#32713=CARTESIAN_POINT('Ctrl Pts',(0.0596315829014974,-0.125876921640408,
0.158457306590168));
#32714=CARTESIAN_POINT('Ctrl Pts',(0.138129079193178,-0.0179243554725553,
0.166409810705271));
#32715=CARTESIAN_POINT('Ctrl Pts',(0.0897844651888838,0.106487909275724,
0.174362314820374));
#32716=CARTESIAN_POINT('Ctrl Pts',(-0.0410080379701501,0.133113732800722,
0.182314818935477));
#32717=CARTESIAN_POINT('Ctrl Pts',(-0.111567175621,0.0606792399755161,0.188339617819891));
#32718=CARTESIAN_POINT('Ctrl Pts',(-0.117821973380904,0.0108165964048154,
0.19171358199927));
#32719=CARTESIAN_POINT('Ctrl Pts',(-0.117728105208174,0.000106637828744488,
0.192436711473616));
#32720=CARTESIAN_POINT('Origin',(0.,0.,-0.0924367114736154));
#32721=CARTESIAN_POINT('',(-0.117616583813332,6.45879523355414E-5,0.0825632885263843));
#32722=CARTESIAN_POINT('',(-0.117696063073914,-0.000101172369946279,0.092436711473616));
#32723=CARTESIAN_POINT('',(-0.117775,-8.88924268665971E-15,-0.0924367114736154));
#32724=CARTESIAN_POINT('Ctrl Pts',(-0.117616583813332,6.4587952335533E-5,
0.0825632885263843));
#32725=CARTESIAN_POINT('Ctrl Pts',(-0.117498290532644,-0.023772899795338,
0.0841689336444552));
#32726=CARTESIAN_POINT('Ctrl Pts',(-0.0988756392612849,-0.087091103874762,
0.0884224643346654));
#32727=CARTESIAN_POINT('Ctrl Pts',(0.00455872999049264,-0.139160029798142,
0.0953238805970148));
#32728=CARTESIAN_POINT('Ctrl Pts',(0.119435794773867,-0.0715642270726515,
0.103267537313433));
#32729=CARTESIAN_POINT('Ctrl Pts',(0.124859895376695,0.0616145512171006,
0.111211194029851));
#32730=CARTESIAN_POINT('Ctrl Pts',(0.0158602180480347,0.138328544685192,
0.119154850746269));
#32731=CARTESIAN_POINT('Ctrl Pts',(-0.094824103560013,0.0934823880103396,
0.126272215578446));
#32732=CARTESIAN_POINT('Ctrl Pts',(-0.117474012159943,0.0269054906934358,
0.130741694838485));
#32733=CARTESIAN_POINT('Ctrl Pts',(-0.117685857408994,-9.79219620674231E-5,
0.132563288526384));
#32734=CARTESIAN_POINT('Ctrl Pts',(-0.117696063073914,-0.000101172369946261,
0.092436711473616));
#32735=CARTESIAN_POINT('Ctrl Pts',(-0.117792623998916,-0.0119605829319943,
0.0932368988721926));
#32736=CARTESIAN_POINT('Ctrl Pts',(-0.110686607712821,-0.0629944099979452,
0.0966879209758034));
#32737=CARTESIAN_POINT('Ctrl Pts',(-0.0371242974264225,-0.134248668971966,
0.102789777784449));
#32738=CARTESIAN_POINT('Ctrl Pts',(0.0928396337021713,-0.10383510521762,
0.110742281899551));
#32739=CARTESIAN_POINT('Ctrl Pts',(0.137550169005636,0.0219289054269618,
0.118694786014654));
#32740=CARTESIAN_POINT('Ctrl Pts',(0.0559501922162531,0.127555870431356,
0.126647290129757));
#32741=CARTESIAN_POINT('Ctrl Pts',(-0.0763838391282559,0.116105719252975,
0.134561265282744));
#32742=CARTESIAN_POINT('Ctrl Pts',(-0.117918750607874,0.0384749486295239,
0.139824405730697));
#32743=CARTESIAN_POINT('Ctrl Pts',(-0.117968412270431,-1.06668654225827E-5,
0.142436711473616));
#32744=CARTESIAN_POINT('Origin',(0.,0.,-0.0924367114736154));
#32745=CARTESIAN_POINT('',(-0.117919967015755,7.48285734863531E-5,0.0325632885263843));
#32746=CARTESIAN_POINT('',(-0.117605093279175,5.63740904734461E-5,0.042436711473616));
#32747=CARTESIAN_POINT('',(-0.117775,-8.88924268665971E-15,-0.0924367114736154));
#32748=CARTESIAN_POINT('Ctrl Pts',(-0.117919967015755,7.48285734863559E-5,
0.0325632885263843));
#32749=CARTESIAN_POINT('Ctrl Pts',(-0.117681732256532,-0.0350969523534404,
0.0349482868782861));
#32750=CARTESIAN_POINT('Ctrl Pts',(-0.0823020584651488,-0.1097611636214,
0.0399811708023271));
#32751=CARTESIAN_POINT('Ctrl Pts',(0.0446654385229893,-0.131869273048715,
0.0476619402985074));
#32752=CARTESIAN_POINT('Ctrl Pts',(0.135042047193827,-0.033912683303242,
0.0556055970149253));
#32753=CARTESIAN_POINT('Ctrl Pts',(0.101666114468308,0.0951356880412728,
0.0635492537313433));
#32754=CARTESIAN_POINT('Ctrl Pts',(-0.0248796065525388,0.136992916606216,
0.0714929104477611));
#32755=CARTESIAN_POINT('Ctrl Pts',(-0.107654697213721,0.0702257630245385,
0.0778309220461081));
#32756=CARTESIAN_POINT('Ctrl Pts',(-0.117693369175918,0.0155377418730691,
0.0815210480723159));
#32757=CARTESIAN_POINT('Ctrl Pts',(-0.117616583813332,6.4587952335533E-5,
0.0825632885263843));
#32758=CARTESIAN_POINT('Ctrl Pts',(-0.117605093279175,5.6374090473453E-5,
0.042436711473616));
#32759=CARTESIAN_POINT('Ctrl Pts',(-0.117506950346121,-0.0231366833782073,
0.0439985573086537));
#32760=CARTESIAN_POINT('Ctrl Pts',(-0.0996401976376468,-0.0858346907547986,
0.0482112378487256));
#32761=CARTESIAN_POINT('Ctrl Pts',(0.00241643506700816,-0.139265216174241,
0.0550747530938317));
#32762=CARTESIAN_POINT('Ctrl Pts',(0.118445458723555,-0.0732914200146354,
0.0630272572089346));
#32763=CARTESIAN_POINT('Ctrl Pts',(0.125708256673902,0.0599868231457294,
0.0709797613240373));
#32764=CARTESIAN_POINT('Ctrl Pts',(0.0175344664057042,0.138178956948752,
0.0789322654391402));
#32765=CARTESIAN_POINT('Ctrl Pts',(-0.0942361274410431,0.0943834610594897,
0.0860845821556665));
#32766=CARTESIAN_POINT('Ctrl Pts',(-0.117472740117216,0.0273268854223547,
0.0905860641671583));
#32767=CARTESIAN_POINT('Ctrl Pts',(-0.117696063073914,-0.000101172369946261,
0.092436711473616));
#32768=CARTESIAN_POINT('Origin',(0.,0.,0.55));
#32769=CARTESIAN_POINT('',(-0.143213254968838,-6.38556725402083E-7,0.507000235761732));
#32770=CARTESIAN_POINT('Ctrl Pts',(-0.0334019664626817,0.112939183906321,
0.532225));
#32771=CARTESIAN_POINT('Ctrl Pts',(-0.025060850432499,0.115799622360937,
0.531847620192936));
#32772=CARTESIAN_POINT('Ctrl Pts',(-0.0164290366846974,0.117635249741265,
0.531473612813392));
#32773=CARTESIAN_POINT('Ctrl Pts',(-0.00767275263448023,0.118510014194121,
0.531100586051555));
#32774=CARTESIAN_POINT('Ctrl Pts',(-0.00421690952474848,0.118855257529045,
0.530953363558858));
#32775=CARTESIAN_POINT('Ctrl Pts',(-0.000739669302851069,0.119050301419728,
0.530806218229583));
#32776=CARTESIAN_POINT('Ctrl Pts',(0.00274357664202706,0.119096927952431,
0.530659241408731));
#32777=CARTESIAN_POINT('Ctrl Pts',(0.00973382066470735,0.119190498962541,
0.5303642855372));
#32778=CARTESIAN_POINT('Ctrl Pts',(0.0167166427004772,0.118687723090435,
0.530071327820757));
#32779=CARTESIAN_POINT('Ctrl Pts',(0.023612882680227,0.11761343656186,0.529779224661465));
#32780=CARTESIAN_POINT('Ctrl Pts',(0.0274136336191392,0.117021360946144,
0.529618236737583));
#32781=CARTESIAN_POINT('Ctrl Pts',(0.0311881579134606,0.116255363574116,
0.529457508384123));
#32782=CARTESIAN_POINT('Ctrl Pts',(0.0349231679080101,0.115317271371855,
0.529296848155877));
#32783=CARTESIAN_POINT('Ctrl Pts',(0.037971953630239,0.114551532560831,
0.529165705639333));
#32784=CARTESIAN_POINT('Ctrl Pts',(0.0409939934565533,0.113670841591964,
0.529034622190513));
#32785=CARTESIAN_POINT('Ctrl Pts',(0.0439689729533011,0.112680856226694,
0.528904071147902));
#32786=CARTESIAN_POINT('Ctrl Pts',(0.0505577881110133,0.110488293021555,
0.528614934133899));
#32787=CARTESIAN_POINT('Ctrl Pts',(0.0569328249215936,0.107756906396238,
0.528327689901185));
#32788=CARTESIAN_POINT('Ctrl Pts',(0.0630179104963209,0.104502120084129,
0.528041256645784));
#32789=CARTESIAN_POINT('Ctrl Pts',(0.0668676595642169,0.102442968997859,
0.527860043720435));
#32790=CARTESIAN_POINT('Ctrl Pts',(0.0706013360983203,0.100173990889927,
0.527679155388847));
#32791=CARTESIAN_POINT('Ctrl Pts',(0.0741982818595768,0.0976957705995567,
0.527498317717128));
#32792=CARTESIAN_POINT('Ctrl Pts',(0.0762868294587642,0.0962568050489885,
0.527393315276118));
#32793=CARTESIAN_POINT('Ctrl Pts',(0.0783301222953497,0.0947465519651971,
0.527288283929736));
#32794=CARTESIAN_POINT('Ctrl Pts',(0.0803210903525092,0.0931669243552789,
0.527183314414725));
#32795=CARTESIAN_POINT('Ctrl Pts',(0.0873333522084643,0.0876034185040368,
0.526813607967904));
#32796=CARTESIAN_POINT('Ctrl Pts',(0.0936466399845286,0.0812254488323135,
0.526447434844115));
#32797=CARTESIAN_POINT('Ctrl Pts',(0.0992257444432458,0.0742158265894858,
0.526082561055055));
#32798=CARTESIAN_POINT('Ctrl Pts',(0.101943770530818,0.0708008813664647,
0.525904801974781));
#32799=CARTESIAN_POINT('Ctrl Pts',(0.104487132714136,0.0672353052679948,
0.525727351283807));
#32800=CARTESIAN_POINT('Ctrl Pts',(0.106849003984973,0.0635370592318222,
0.525549950667934));
#32801=CARTESIAN_POINT('Ctrl Pts',(0.108451822333258,0.0610273472604538,
0.525429562666425));
#32802=CARTESIAN_POINT('Ctrl Pts',(0.109972218146102,0.0584542637442968,
0.525309095710787));
#32803=CARTESIAN_POINT('Ctrl Pts',(0.111403508282751,0.0558304813946845,
0.525188806889777));
#32804=CARTESIAN_POINT('Ctrl Pts',(0.115946659550801,0.0475021629053002,
0.524806990306466));
#32805=CARTESIAN_POINT('Ctrl Pts',(0.119574294719482,0.0387078320373927,
0.524428851599571));
#32806=CARTESIAN_POINT('Ctrl Pts',(0.122229265704535,0.02963297991244,0.524051927142185));
#32807=CARTESIAN_POINT('Ctrl Pts',(0.123491040005696,0.0253201586942182,
0.523872793887439));
#32808=CARTESIAN_POINT('Ctrl Pts',(0.124532521003962,0.0209434889498052,
0.523693934885913));
#32809=CARTESIAN_POINT('Ctrl Pts',(0.125343829183128,0.0165211886089503,
0.523515085689393));
#32810=CARTESIAN_POINT('Ctrl Pts',(0.126073723283802,0.0125426623065107,
0.523354183856031));
#32811=CARTESIAN_POINT('Ctrl Pts',(0.126617185118597,0.00852274589339418,
0.523193115530006));
#32812=CARTESIAN_POINT('Ctrl Pts',(0.126964066890117,0.00450317609134152,
0.523032822082874));
#32813=CARTESIAN_POINT('Ctrl Pts',(0.127610380106321,-0.00298612228009172,
0.522734161899901));
#32814=CARTESIAN_POINT('Ctrl Pts',(0.127580071374667,-0.0104910608890547,
0.522437493943663));
#32815=CARTESIAN_POINT('Ctrl Pts',(0.126833825603371,-0.0179253657039838,
0.52214162882945));
#32816=CARTESIAN_POINT('Ctrl Pts',(0.126370997360361,-0.0225361874571381,
0.521958130662699));
#32817=CARTESIAN_POINT('Ctrl Pts',(0.125632379838884,-0.0271199619342287,
0.521774941316387));
#32818=CARTESIAN_POINT('Ctrl Pts',(0.124632255285918,-0.0316602427367966,
0.52159177704026));
#32819=CARTESIAN_POINT('Ctrl Pts',(0.123677051866189,-0.0359965943804856,
0.521416839686298));
#32820=CARTESIAN_POINT('Ctrl Pts',(0.122480780227546,-0.0402989646849493,
0.521241685776095));
#32821=CARTESIAN_POINT('Ctrl Pts',(0.121065837229724,-0.044520244829744,
0.521067408183846));
#32822=CARTESIAN_POINT('Ctrl Pts',(0.118338362465597,-0.0526572758514579,
0.520731466922931));
#32823=CARTESIAN_POINT('Ctrl Pts',(0.114798640009948,-0.0605127756442529,
0.520398022841861));
#32824=CARTESIAN_POINT('Ctrl Pts',(0.11054080941355,-0.0679858568570343,
0.520065383890604));
#32825=CARTESIAN_POINT('Ctrl Pts',(0.108372779925159,-0.0717910482735648,
0.5198960086562));
#32826=CARTESIAN_POINT('Ctrl Pts',(0.10601800718922,-0.0754969965361626,
0.51972684216845));
#32827=CARTESIAN_POINT('Ctrl Pts',(0.103485875290119,-0.0790891197455118,
0.519557661047695));
#32828=CARTESIAN_POINT('Ctrl Pts',(0.101239265068231,-0.0822761972920135,
0.519407556688845));
#32829=CARTESIAN_POINT('Ctrl Pts',(0.0988505693656959,-0.0853758696950735,
0.519257316754896));
#32830=CARTESIAN_POINT('Ctrl Pts',(0.0963426843438634,-0.0883583266502687,
0.51910776182463));
#32831=CARTESIAN_POINT('Ctrl Pts',(0.0906830843157466,-0.0950889037383469,
0.518770257880003));
#32832=CARTESIAN_POINT('Ctrl Pts',(0.084404823468622,-0.101245530098652,
0.518435260730044));
#32833=CARTESIAN_POINT('Ctrl Pts',(0.077590384105458,-0.106717161154373,
0.51810105566737));
#32834=CARTESIAN_POINT('Ctrl Pts',(0.072812396824573,-0.110553629893275,
0.517866725672845));
#32835=CARTESIAN_POINT('Ctrl Pts',(0.0677701261881638,-0.114053116790221,
0.517632785084427));
#32836=CARTESIAN_POINT('Ctrl Pts',(0.0624852082906241,-0.117169678449436,
0.517398642838002));
#32837=CARTESIAN_POINT('Ctrl Pts',(0.060232694538615,-0.11849800523378,
0.517298847790998));
#32838=CARTESIAN_POINT('Ctrl Pts',(0.0579421351333471,-0.119753052219492,
0.517199285984453));
#32839=CARTESIAN_POINT('Ctrl Pts',(0.0556164103289471,-0.120931647626768,
0.517099943244175));
#32840=CARTESIAN_POINT('Ctrl Pts',(0.0470766353824801,-0.125259304756293,
0.516735168941155));
#32841=CARTESIAN_POINT('Ctrl Pts',(0.0380619111816488,-0.128561628767388,
0.516373216300106));
#32842=CARTESIAN_POINT('Ctrl Pts',(0.0287540615399164,-0.13087769180711,
0.516011917283344));
#32843=CARTESIAN_POINT('Ctrl Pts',(0.0244834739512418,-0.131940337901829,
0.515846147620515));
#32844=CARTESIAN_POINT('Ctrl Pts',(0.0201508023558736,-0.132794720803219,
0.515680515553343));
#32845=CARTESIAN_POINT('Ctrl Pts',(0.0157724288157125,-0.133441328903782,
0.515514811679433));
#32846=CARTESIAN_POINT('Ctrl Pts',(0.0127414878228209,-0.13388894512025,
0.515400102721983));
#32847=CARTESIAN_POINT('Ctrl Pts',(0.0096905970655013,-0.134236406792975,
0.515285434752076));
#32848=CARTESIAN_POINT('Ctrl Pts',(0.00663678161128016,-0.134483505205774,
0.515171166690044));
#32849=CARTESIAN_POINT('Ctrl Pts',(-0.00335208404858516,-0.135291750788136,
0.514797402021565));
#32850=CARTESIAN_POINT('Ctrl Pts',(-0.0134050142894213,-0.135035519709951,
0.514426646108251));
#32851=CARTESIAN_POINT('Ctrl Pts',(-0.0233297246571887,-0.13373576937046,
0.514056571073779));
#32852=CARTESIAN_POINT('Ctrl Pts',(-0.0275876193693317,-0.133178151073044,
0.5138978016514));
#32853=CARTESIAN_POINT('Ctrl Pts',(-0.0318220223293205,-0.132427814053447,
0.513739157550061));
#32854=CARTESIAN_POINT('Ctrl Pts',(-0.0360175989408762,-0.131483472271743,
0.513580454950452));
#32855=CARTESIAN_POINT('Ctrl Pts',(-0.0391091145169674,-0.130787632915777,
0.513463514752696));
#32856=CARTESIAN_POINT('Ctrl Pts',(-0.0421792587373029,-0.12998615137042,
0.513346550232001));
#32857=CARTESIAN_POINT('Ctrl Pts',(-0.0452082926810733,-0.129082949079949,
0.513230012664731));
#32858=CARTESIAN_POINT('Ctrl Pts',(-0.0547989520179786,-0.126223190608758,
0.512861026338271));
#32859=CARTESIAN_POINT('Ctrl Pts',(-0.0640135938008781,-0.122340292920341,
0.512494993993967));
#32860=CARTESIAN_POINT('Ctrl Pts',(-0.0726621826878073,-0.117434240919462,
0.512129678956248));
#32861=CARTESIAN_POINT('Ctrl Pts',(-0.0732258670681981,-0.11711448183293,
0.512105869016456));
#32862=CARTESIAN_POINT('Ctrl Pts',(-0.073787141143001,-0.116790358750658,
0.512082062123761));
#32863=CARTESIAN_POINT('Ctrl Pts',(-0.0743459493499517,-0.11646186427858,
0.5120582576589));
#32864=CARTESIAN_POINT('Ctrl Pts',(-0.0780940452153038,-0.11425855237787,
0.511898593904482));
#32865=CARTESIAN_POINT('Ctrl Pts',(-0.0817313018976771,-0.111858709629848,
0.511739039373249));
#32866=CARTESIAN_POINT('Ctrl Pts',(-0.085250803842968,-0.109275770384611,
0.511579407204066));
#32867=CARTESIAN_POINT('Ctrl Pts',(-0.0875213278289363,-0.107609447819153,
0.511476424260826));
#32868=CARTESIAN_POINT('Ctrl Pts',(-0.0897413530091093,-0.105867722400153,
0.511373470200391));
#32869=CARTESIAN_POINT('Ctrl Pts',(-0.0919020268850941,-0.104060687103246,
0.511270839257698));
#32870=CARTESIAN_POINT('Ctrl Pts',(-0.0994865656445924,-0.0977175136139456,
0.510910577410027));
#32871=CARTESIAN_POINT('Ctrl Pts',(-0.106368098520952,-0.0905540945926997,
0.510553119515254));
#32872=CARTESIAN_POINT('Ctrl Pts',(-0.112476669881714,-0.082740585635558,
0.510196385012091));
#32873=CARTESIAN_POINT('Ctrl Pts',(-0.115701946031867,-0.0786151162581588,
0.510008032086826));
#32874=CARTESIAN_POINT('Ctrl Pts',(-0.118711292938496,-0.0743076837297934,
0.509819880825374));
#32875=CARTESIAN_POINT('Ctrl Pts',(-0.121490605137305,-0.0698396458594739,
0.509631624987483));
#32876=CARTESIAN_POINT('Ctrl Pts',(-0.123158603264919,-0.0671581627195108,
0.509518643658775));
#32877=CARTESIAN_POINT('Ctrl Pts',(-0.124742701375389,-0.0644198867277164,
0.509405676189658));
#32878=CARTESIAN_POINT('Ctrl Pts',(-0.126234357059848,-0.06164059243669,
0.509293097144302));
#32879=CARTESIAN_POINT('Ctrl Pts',(-0.131306921574689,-0.0521892493795411,
0.508910257809098));
#32880=CARTESIAN_POINT('Ctrl Pts',(-0.135335100093566,-0.0422336175385342,
0.508530533331389));
#32881=CARTESIAN_POINT('Ctrl Pts',(-0.138212265982587,-0.0319628814891436,
0.508151426353207));
#32882=CARTESIAN_POINT('Ctrl Pts',(-0.139343321582236,-0.0279253063303673,
0.508002393907016));
#32883=CARTESIAN_POINT('Ctrl Pts',(-0.140295939750969,-0.0238387054236251,
0.507853456888584));
#32884=CARTESIAN_POINT('Ctrl Pts',(-0.14106118303298,-0.0197137190414539,
0.507704463579619));
#32885=CARTESIAN_POINT('Ctrl Pts',(-0.141663078970186,-0.0164692442413196,
0.507587274093027));
#32886=CARTESIAN_POINT('Ctrl Pts',(-0.142148737315268,-0.0132004963364534,
0.507470032942495));
#32887=CARTESIAN_POINT('Ctrl Pts',(-0.14251240365623,-0.00992818124989041,
0.507353216880015));
#32888=CARTESIAN_POINT('Ctrl Pts',(-0.14286252481498,-0.00677774740200931,
0.507240751769694));
#32889=CARTESIAN_POINT('Ctrl Pts',(-0.143100295244155,-0.00362062020727709,
0.507128557913111));
#32890=CARTESIAN_POINT('Ctrl Pts',(-0.143222931917338,-0.0004616047295162,
0.507016572073626));
#32891=CARTESIAN_POINT('Ctrl Pts',(-0.143228895796354,-0.000307980323141247,
0.507011126149655));
#32892=CARTESIAN_POINT('Ctrl Pts',(-0.143234587305958,-0.000154351422170947,
0.50700568071763));
#32893=CARTESIAN_POINT('Ctrl Pts',(-0.143240006909252,-7.18572550341278E-7,
0.507000235770275));
#32894=CARTESIAN_POINT('',(-0.00156805256656782,0.146109107730171,0.50365));
#32895=CARTESIAN_POINT('Ctrl Pts',(-0.0015703316452181,0.146071601053478,
0.50365));
#32896=CARTESIAN_POINT('Ctrl Pts',(-0.0117120407853717,0.144648246558049,
0.504950624278524));
#32897=CARTESIAN_POINT('Ctrl Pts',(-0.0216505365241647,0.142222557694311,
0.506260995613922));
#32898=CARTESIAN_POINT('Ctrl Pts',(-0.0312063389538959,0.13880538472021,
0.507590209176103));
#32899=CARTESIAN_POINT('Ctrl Pts',(-0.0379631701734481,0.136389129130603,
0.508530085419929));
#32900=CARTESIAN_POINT('Ctrl Pts',(-0.0445284394867549,0.133476109724793,
0.50947938238263));
#32901=CARTESIAN_POINT('Ctrl Pts',(-0.050827361354341,0.13005807034167,
0.510441315490383));
#32902=CARTESIAN_POINT('Ctrl Pts',(-0.0535603409840707,0.12857504956382,
0.510858679547901));
#32903=CARTESIAN_POINT('Ctrl Pts',(-0.056235007151428,0.127001156165417,
0.511277203939051));
#32904=CARTESIAN_POINT('Ctrl Pts',(-0.0588447172056459,0.125337452214503,
0.511696981696819));
#32905=CARTESIAN_POINT('Ctrl Pts',(-0.0624191770014244,0.123058715204999,
0.512271941629964));
#32906=CARTESIAN_POINT('Ctrl Pts',(-0.0658727208815536,0.120611069028702,
0.512849385708712));
#32907=CARTESIAN_POINT('Ctrl Pts',(-0.0691906694557284,0.117994047416377,
0.513430106410014));
#32908=CARTESIAN_POINT('Ctrl Pts',(-0.0733832729377804,0.114687144467415,
0.51416391273038));
#32909=CARTESIAN_POINT('Ctrl Pts',(-0.0773595119772722,0.111109779201256,
0.514902950893669));
#32910=CARTESIAN_POINT('Ctrl Pts',(-0.0811052238678245,0.107288843574283,
0.515648819828442));
#32911=CARTESIAN_POINT('Ctrl Pts',(-0.0841017207582698,0.104232169153142,
0.516245500515327));
#32912=CARTESIAN_POINT('Ctrl Pts',(-0.0869506135922833,0.101019546539762,
0.516846552684068));
#32913=CARTESIAN_POINT('Ctrl Pts',(-0.0896425492995218,0.097664267789728,
0.517452794926569));
#32914=CARTESIAN_POINT('Ctrl Pts',(-0.0913307146861822,0.0955601070428074,
0.517832981261246));
#32915=CARTESIAN_POINT('Ctrl Pts',(-0.0929559105919431,0.0934010507133458,
0.518214974249558));
#32916=CARTESIAN_POINT('Ctrl Pts',(-0.094511034598742,0.0911980939617143,
0.518597709131816));
#32917=CARTESIAN_POINT('Ctrl Pts',(-0.0989061554610084,0.0849720559509604,
0.519679401690337));
#32918=CARTESIAN_POINT('Ctrl Pts',(-0.102756278369653,0.0783797189661076,
0.520769927597638));
#32919=CARTESIAN_POINT('Ctrl Pts',(-0.106019480011838,0.0715022869017531,
0.521874709646989));
#32920=CARTESIAN_POINT('Ctrl Pts',(-0.10810684462629,0.0671030159085511,
0.522581403014228));
#32921=CARTESIAN_POINT('Ctrl Pts',(-0.109953633570546,0.0625869322502571,
0.523293929634644));
#32922=CARTESIAN_POINT('Ctrl Pts',(-0.111544021459737,0.0579753350677128,
0.524013708847662));
#32923=CARTESIAN_POINT('Ctrl Pts',(-0.11291963712523,0.0539865060717378,
0.524636286250227));
#32924=CARTESIAN_POINT('Ctrl Pts',(-0.114104149138597,0.0499208096400247,
0.525265113718246));
#32925=CARTESIAN_POINT('Ctrl Pts',(-0.115079157041328,0.0458232444145113,
0.525896440126774));
#32926=CARTESIAN_POINT('Ctrl Pts',(-0.117097797518837,0.0373397121269415,
0.527203528037759));
#32927=CARTESIAN_POINT('Ctrl Pts',(-0.118231089846825,0.0286982113614575,
0.528524583654289));
#32928=CARTESIAN_POINT('Ctrl Pts',(-0.118391363114938,0.0200276346563605,
0.529869408057975));
#32929=CARTESIAN_POINT('Ctrl Pts',(-0.118483921504357,0.0150203453896601,
0.530646048993314));
#32930=CARTESIAN_POINT('Ctrl Pts',(-0.118251089036742,0.0100034984621487,
0.531430617066573));
#32931=CARTESIAN_POINT('Ctrl Pts',(-0.117668597464311,0.00500517689817885,
0.532225));
#32932=CARTESIAN_POINT('',(-0.115076068242798,0.0902060425677366,0.50365));
#32933=CARTESIAN_POINT('Origin',(0.,0.,0.50365));
#32934=CARTESIAN_POINT('Ctrl Pts',(-0.143240006909252,-7.18572550341278E-7,
0.507000235770275));
#32935=CARTESIAN_POINT('Ctrl Pts',(-0.143520908694302,0.00796217822295569,
0.506718020385041));
#32936=CARTESIAN_POINT('Ctrl Pts',(-0.14307308860376,0.0159355469497794,
0.506437106818574));
#32937=CARTESIAN_POINT('Ctrl Pts',(-0.141950240996583,0.0238446282639654,
0.506156482679269));
#32938=CARTESIAN_POINT('Ctrl Pts',(-0.141327877173321,0.0282284164590215,
0.506000940367809));
#32939=CARTESIAN_POINT('Ctrl Pts',(-0.140497759623186,0.0325924948231262,
0.505845486973662));
#32940=CARTESIAN_POINT('Ctrl Pts',(-0.139466483050223,0.0369239027928834,
0.505689950104037));
#32941=CARTESIAN_POINT('Ctrl Pts',(-0.138800760016326,0.0397199694642927,
0.50558954592591));
#32942=CARTESIAN_POINT('Ctrl Pts',(-0.138051361267828,0.0425008441913541,
0.50548916176982));
#32943=CARTESIAN_POINT('Ctrl Pts',(-0.137223245651255,0.0452539885083259,
0.505389082377033));
#32944=CARTESIAN_POINT('Ctrl Pts',(-0.134183880382411,0.0553586297560613,
0.505021769136614));
#32945=CARTESIAN_POINT('Ctrl Pts',(-0.130080477516678,0.06512485891418,
0.504657328869907));
#32946=CARTESIAN_POINT('Ctrl Pts',(-0.125019236367424,0.0743847486871139,
0.504293559587933));
#32947=CARTESIAN_POINT('Ctrl Pts',(-0.122033398952289,0.0798475441810871,
0.504078956904408));
#32948=CARTESIAN_POINT('Ctrl Pts',(-0.118713161823888,0.0851340339476938,
0.503864587744543));
#32949=CARTESIAN_POINT('Ctrl Pts',(-0.115072616245007,0.0902061753896176,
0.50365));
#32950=CARTESIAN_POINT('',(-0.05,-6.12323399573676E-18,0.6));
#32951=CARTESIAN_POINT('',(-0.1,-1.22464679914735E-17,0.55));
#32952=CARTESIAN_POINT('Origin',(0.,0.,0.6));
#32953=CARTESIAN_POINT('Ctrl Pts',(0.0850780204044556,-0.119080027477571,
-0.0164977839420937));
#32954=CARTESIAN_POINT('Ctrl Pts',(0.124701079614845,-0.0907709019978731,
-0.0138498983699544));
#32955=CARTESIAN_POINT('Ctrl Pts',(0.172780327456066,0.00801716155080004,
-0.00855412722567576));
#32956=CARTESIAN_POINT('Ctrl Pts',(0.0867037234097596,0.149857524855506,
-0.000610470509257829));
#32957=CARTESIAN_POINT('Ctrl Pts',(-0.0789008477636886,0.153920736728128,
0.00733318620716008));
#32958=CARTESIAN_POINT('Ctrl Pts',(-0.172161895422237,0.0171520622219753,
0.015276842923578));
#32959=CARTESIAN_POINT('Ctrl Pts',(-0.107670523249975,-0.135451540092597,
0.0232204996399959));
#32960=CARTESIAN_POINT('Ctrl Pts',(0.0555023301026467,-0.163863876974566,
0.0311641563564139));
#32961=CARTESIAN_POINT('Ctrl Pts',(0.167806441153186,-0.042140702198512,
0.0391078130728317));
#32962=CARTESIAN_POINT('Ctrl Pts',(0.126332717914983,0.118217855613161,
0.0470514697892497));
#32963=CARTESIAN_POINT('Ctrl Pts',(-0.0309159874248675,0.170230637616809,
0.0549951265056676));
#32964=CARTESIAN_POINT('Ctrl Pts',(-0.159831956410111,0.066245824895792,
0.0629387832220855));
#32965=CARTESIAN_POINT('Ctrl Pts',(-0.14227559413168,-0.0984502643440673,
0.0708824399385034));
#32966=CARTESIAN_POINT('Ctrl Pts',(0.00566478568548768,-0.172923543714354,
0.0788260966549214));
#32967=CARTESIAN_POINT('Ctrl Pts',(0.148413742858461,-0.0889274008243077,
0.0867697533713393));
#32968=CARTESIAN_POINT('Ctrl Pts',(0.155153858530075,0.0765636983283585,
0.0947134100877573));
#32969=CARTESIAN_POINT('Ctrl Pts',(0.0197082819896427,0.171890320651054,
0.102657066804175));
#32970=CARTESIAN_POINT('Ctrl Pts',(-0.133798285716779,0.109693800981729,
0.110600723520593));
#32971=CARTESIAN_POINT('Ctrl Pts',(-0.164689815771182,-0.0530280538225922,
0.118544380237011));
#32972=CARTESIAN_POINT('Ctrl Pts',(-0.044656766037051,-0.167154062007556,
0.126488036953429));
#32973=CARTESIAN_POINT('Ctrl Pts',(0.11630050845274,-0.128097231996654,
0.134431693669847));
#32974=CARTESIAN_POINT('Ctrl Pts',(0.170678001253376,0.0283501086412318,
0.142375350386265));
#32975=CARTESIAN_POINT('Ctrl Pts',(0.0686432422541576,0.158816918899349,
0.150319007102683));
#32976=CARTESIAN_POINT('Ctrl Pts',(-0.0962973622855325,0.143741179688805,
0.1582626638191));
#32977=CARTESIAN_POINT('Ctrl Pts',(-0.172989410659926,-0.00306144592864502,
0.166206320535519));
#32978=CARTESIAN_POINT('Ctrl Pts',(-0.0911509925455794,-0.147058509343496,
0.174149977251936));
#32979=CARTESIAN_POINT('Ctrl Pts',(0.0742197602705133,-0.1562886299111,
0.182093633968354));
#32980=CARTESIAN_POINT('Ctrl Pts',(0.171574250349044,-0.0222931661803689,
0.190037290684772));
#32981=CARTESIAN_POINT('Ctrl Pts',(0.111695151232628,0.132132137756553,
0.19798094740119));
#32982=CARTESIAN_POINT('Ctrl Pts',(-0.0505433024217535,0.165469281811646,
0.205924604117608));
#32983=CARTESIAN_POINT('Ctrl Pts',(-0.16646300584434,0.0471675346608595,
0.213868260834026));
#32984=CARTESIAN_POINT('Ctrl Pts',(-0.129833152315396,-0.11435935117077,
0.221811917550444));
#32985=CARTESIAN_POINT('Ctrl Pts',(0.0257780314041745,-0.171085363892111,
0.229755574266861));
#32986=CARTESIAN_POINT('Ctrl Pts',(0.157765784501968,-0.0710258113735757,
0.23769923098328));
#32987=CARTESIAN_POINT('Ctrl Pts',(0.145174263631334,0.0941230142947892,
0.245642887699697));
#32988=CARTESIAN_POINT('Ctrl Pts',(-0.000457445268631668,0.173015893445265,
0.253586544416116));
#32989=CARTESIAN_POINT('Ctrl Pts',(-0.145669943468849,0.0933540369270586,
0.261530201132533));
#32990=CARTESIAN_POINT('Ctrl Pts',(-0.15738800412666,-0.0718590620464598,
0.269473857848952));
#32991=CARTESIAN_POINT('Ctrl Pts',(-0.0248729952365478,-0.171219282641631,
0.277417514565369));
#32992=CARTESIAN_POINT('Ctrl Pts',(0.130436053586269,-0.11367121256306,
0.285361171281788));
#32993=CARTESIAN_POINT('Ctrl Pts',(0.166211263149388,0.0480471086044073,
0.293304827998205));
#32994=CARTESIAN_POINT('Ctrl Pts',(0.0496676170739063,0.16573423439711,
0.301248484714623));
#32995=CARTESIAN_POINT('Ctrl Pts',(-0.112392286114514,0.131539661939415,
0.309192141431041));
#32996=CARTESIAN_POINT('Ctrl Pts',(-0.171453968444308,-0.0232001154910803,
0.317135798147459));
#32997=CARTESIAN_POINT('Ctrl Pts',(-0.0733922898759408,-0.156678908596981,
0.325079454863877));
#32998=CARTESIAN_POINT('Ctrl Pts',(0.0919273431499614,-0.146574459688691,
0.333023111580294));
#32999=CARTESIAN_POINT('Ctrl Pts',(0.173003180832518,-0.00214665863879225,
0.340966768296713));
#33000=CARTESIAN_POINT('Ctrl Pts',(0.0955359320753977,0.14424837648421,
0.34891042501313));
#33001=CARTESIAN_POINT('Ctrl Pts',(-0.0694820837435447,0.158451723911329,
0.356854081729549));
#33002=CARTESIAN_POINT('Ctrl Pts',(-0.170825527907542,0.0274471879557805,
0.364797738445966));
#33003=CARTESIAN_POINT('Ctrl Pts',(-0.115621519313607,-0.128710417100276,
0.372741395162384));
#33004=CARTESIAN_POINT('Ctrl Pts',(0.0455400241630207,-0.16691559576681,
0.380685051878803));
#33005=CARTESIAN_POINT('Ctrl Pts',(0.164967928025121,-0.0521564373559641,
0.38862870859522));
#33006=CARTESIAN_POINT('Ctrl Pts',(0.133216350942249,0.110399739828213,
0.396572365311638));
#33007=CARTESIAN_POINT('Ctrl Pts',(-0.0206169035662114,0.171783768167507,
0.404516022028056));
#33008=CARTESIAN_POINT('Ctrl Pts',(-0.155556614414135,0.0757420715232724,
0.412459678744474));
#33009=CARTESIAN_POINT('Ctrl Pts',(-0.14794130513946,-0.0897107128565239,
0.420403335460892));
#33010=CARTESIAN_POINT('Ctrl Pts',(-0.00475055195827078,-0.17295152931105,
0.42834699217731));
#33011=CARTESIAN_POINT('Ctrl Pts',(0.142794654932494,-0.0976957016900834,
0.436290648893728));
#33012=CARTESIAN_POINT('Ctrl Pts',(0.159478551636871,0.0670884478109748,
0.444234305610146));
#33013=CARTESIAN_POINT('Ctrl Pts',(0.0300170551768464,0.170394816235914,
0.452177962326563));
#33014=CARTESIAN_POINT('Ctrl Pts',(-0.126959218666436,0.117542321186412,
0.460121619042982));
#33015=CARTESIAN_POINT('Ctrl Pts',(-0.167575279308382,-0.043016329325927,
0.468065275759399));
#33016=CARTESIAN_POINT('Ctrl Pts',(-0.054646434915416,-0.164176211557628,
0.476008932475817));
#33017=CARTESIAN_POINT('Ctrl Pts',(0.108406899182729,-0.134840111552273,
0.483952589192236));
#33018=CARTESIAN_POINT('Ctrl Pts',(0.172027477869207,0.0179856562492908,
0.491896245908652));
#33019=CARTESIAN_POINT('Ctrl Pts',(0.0781660714022324,0.154482616143293,
0.499839902625072));
#33020=CARTESIAN_POINT('Ctrl Pts',(-0.0876620486424683,0.149106276403653,
0.507783559341488));
#33021=CARTESIAN_POINT('Ctrl Pts',(-0.144148268866352,0.0548725112369506,
0.513079330485768));
#33022=CARTESIAN_POINT('Ctrl Pts',(-0.146217781693075,0.00621955117001058,
0.515727216057907));
#33023=CARTESIAN_POINT('Ctrl Pts',(0.0795408277542857,-0.111329858282327,
-0.0109985226280625));
#33024=CARTESIAN_POINT('Ctrl Pts',(0.116585071529219,-0.0848631955302966,
-0.00835063705592319));
#33025=CARTESIAN_POINT('Ctrl Pts',(0.161535143861813,0.00749537498591264,
-0.00305486591164458));
#33026=CARTESIAN_POINT('Ctrl Pts',(0.0810607239872927,0.140104242147965,
0.00488879080477336));
#33027=CARTESIAN_POINT('Ctrl Pts',(-0.0737656883858339,0.143903005144011,
0.0128324475211912));
#33028=CARTESIAN_POINT('Ctrl Pts',(-0.160956961675077,0.0160357424907528,
0.0207761042376092));
#33029=CARTESIAN_POINT('Ctrl Pts',(-0.100662926844399,-0.12663585222528,
0.028719760954027));
#33030=CARTESIAN_POINT('Ctrl Pts',(0.0518900329094276,-0.153199008999282,
0.0366634176704451));
#33031=CARTESIAN_POINT('Ctrl Pts',(0.156884976500066,-0.039398029233422,
0.0446070743868629));
#33032=CARTESIAN_POINT('Ctrl Pts',(0.118110516766091,0.110523799755865,
0.052550731103281));
#33033=CARTESIAN_POINT('Ctrl Pts',(-0.0289038604674246,0.159151397279945,
0.0604943878196987));
#33034=CARTESIAN_POINT('Ctrl Pts',(-0.149429500757181,0.0619343012734311,
0.0684380445361168));
#33035=CARTESIAN_POINT('Ctrl Pts',(-0.133015771554951,-0.0920427565348621,
0.0763817012525346));
#33036=CARTESIAN_POINT('Ctrl Pts',(0.00529610045382266,-0.161669039075616,
0.0843253579689526));
#33037=CARTESIAN_POINT('Ctrl Pts',(0.138754426830263,-0.0831396762404221,
0.0922690146853704));
#33038=CARTESIAN_POINT('Ctrl Pts',(0.145055870812282,0.0715806492912723,
0.100212671401788));
#33039=CARTESIAN_POINT('Ctrl Pts',(0.0184255940091067,0.160703061995767,
0.108156328118206));
#33040=CARTESIAN_POINT('Ctrl Pts',(-0.125090197766985,0.102554522168261,
0.116099984834624));
#33041=CARTESIAN_POINT('Ctrl Pts',(-0.153971192640191,-0.0495767916930391,
0.124043641551042));
#33042=CARTESIAN_POINT('Ctrl Pts',(-0.0417503383192307,-0.156275056605288,
0.13198729826746));
#33043=CARTESIAN_POINT('Ctrl Pts',(0.108731240649445,-0.119760189736536,
0.139930954983878));
#33044=CARTESIAN_POINT('Ctrl Pts',(0.159569644834255,0.0265049785776333,
0.147874611700296));
#33045=CARTESIAN_POINT('Ctrl Pts',(0.0641756858313974,0.148480525646761,
0.155818268416713));
#33046=CARTESIAN_POINT('Ctrl Pts',(-0.0900299733154633,0.134385971376294,
0.163761925133132));
#33047=CARTESIAN_POINT('Ctrl Pts',(-0.161730619156435,-0.00286219568969563,
0.171705581849549));
#33048=CARTESIAN_POINT('Ctrl Pts',(-0.0852185483775114,-0.137487396931492,
0.179649238565968));
#33049=CARTESIAN_POINT('Ctrl Pts',(0.0693892634028907,-0.14611678706926,
0.187592895282385));
#33050=CARTESIAN_POINT('Ctrl Pts',(0.160407562719562,-0.0208422443637096,
0.195536551998804));
#33051=CARTESIAN_POINT('Ctrl Pts',(0.104425617132929,0.123532488886508,
0.203480208715221));
#33052=CARTESIAN_POINT('Ctrl Pts',(-0.0472537571155211,0.154699928144028,
0.211423865431639));
#33053=CARTESIAN_POINT('Ctrl Pts',(-0.155628976936467,0.0440976968224941,
0.219367522148057));
#33054=CARTESIAN_POINT('Ctrl Pts',(-0.121383129932039,-0.106916421072365,
0.227311178864475));
#33055=CARTESIAN_POINT('Ctrl Pts',(0.0241003016527248,-0.159950494803813,
0.235254835580893));
#33056=CARTESIAN_POINT('Ctrl Pts',(0.147497802968786,-0.0664031885287967,
0.243198492297311));
#33057=CARTESIAN_POINT('Ctrl Pts',(0.135725784908488,0.0879971399445481,
0.251142149013729));
#33058=CARTESIAN_POINT('Ctrl Pts',(-0.000427673036423806,0.161755378344027,
0.259085805730147));
#33059=CARTESIAN_POINT('Ctrl Pts',(-0.136189204066452,0.0872782104717779,
0.267029462446565));
#33060=CARTESIAN_POINT('Ctrl Pts',(-0.147144609939394,-0.067182208161988,
0.274973119162982));
#33061=CARTESIAN_POINT('Ctrl Pts',(-0.0232541685906426,-0.160075697625154,
0.282916775879401));
#33062=CARTESIAN_POINT('Ctrl Pts',(0.12194679215539,-0.106273069073731,
0.290860432595819));
#33063=CARTESIAN_POINT('Ctrl Pts',(0.155393618588418,0.0449200248363383,
0.298804089312236));
#33064=CARTESIAN_POINT('Ctrl Pts',(0.0464350646131678,0.154947636633991,
0.306747746028654));
#33065=CARTESIAN_POINT('Ctrl Pts',(-0.105077379894898,0.122978573589753,
0.314691402745072));
#33066=CARTESIAN_POINT('Ctrl Pts',(-0.160295109206645,-0.021690166054439,
0.32263505946149));
#33067=CARTESIAN_POINT('Ctrl Pts',(-0.0686156478460915,-0.146481664972887,
0.330578716177908));
#33068=CARTESIAN_POINT('Ctrl Pts',(0.0859443712093853,-0.137034851020875,
0.338522372894326));
#33069=CARTESIAN_POINT('Ctrl Pts',(0.161743493115198,-0.00200694614453471,
0.346466029610744));
#33070=CARTESIAN_POINT('Ctrl Pts',(0.0893180998033222,0.134860157925877,
0.354409686327162));
#33071=CARTESIAN_POINT('Ctrl Pts',(-0.0649599324100484,0.148139098901043,
0.36235334304358));
#33072=CARTESIAN_POINT('Ctrl Pts',(-0.159707569907411,0.0256608233143121,
0.370296999759998));
#33073=CARTESIAN_POINT('Ctrl Pts',(-0.108096442638088,-0.120333466482715,
0.378240656476415));
#33074=CARTESIAN_POINT('Ctrl Pts',(0.0425761107352605,-0.156052110630637,
0.386184313192834));
#33075=CARTESIAN_POINT('Ctrl Pts',(0.154231204318669,-0.0487619032540464,
0.394127969909251));
#33076=CARTESIAN_POINT('Ctrl Pts',(0.124546137462748,0.103214515900207,
0.402071626625669));
#33077=CARTESIAN_POINT('Ctrl Pts',(-0.0192750791284384,0.160603444342461,
0.410015283342087));
#33078=CARTESIAN_POINT('Ctrl Pts',(-0.145432413851821,0.0708124970015145,
0.417958940058505));
#33079=CARTESIAN_POINT('Ctrl Pts',(-0.138312737107664,-0.0838720074246256,
0.425902596774923));
#33080=CARTESIAN_POINT('Ctrl Pts',(-0.00444136844339109,-0.161695203266036,
0.433846253491342));
#33081=CARTESIAN_POINT('Ctrl Pts',(0.133501049956532,-0.0913373036128839,
0.441789910207758));
#33082=CARTESIAN_POINT('Ctrl Pts',(0.1490990968754,0.0627220831686826,0.449733566924177));
#33083=CARTESIAN_POINT('Ctrl Pts',(0.0280634340592545,0.159304890546491,
0.457677223640594));
#33084=CARTESIAN_POINT('Ctrl Pts',(-0.118696242528426,0.109892231611416,
0.465620880357014));
#33085=CARTESIAN_POINT('Ctrl Pts',(-0.156668859524218,-0.0402166673045443,
0.47356453707343));
#33086=CARTESIAN_POINT('Ctrl Pts',(-0.0510898425507461,-0.153491015690964,
0.481508193789849));
#33087=CARTESIAN_POINT('Ctrl Pts',(0.101351376704318,-0.126064217718754,
0.489451850506266));
#33088=CARTESIAN_POINT('Ctrl Pts',(0.160831292514208,0.0168150831315976,
0.497395507222684));
#33089=CARTESIAN_POINT('Ctrl Pts',(0.0730787339911879,0.144428315365945,
0.505339163939102));
#33090=CARTESIAN_POINT('Ctrl Pts',(-0.0819566778647476,0.13940188772757,
0.51328282065552));
#33091=CARTESIAN_POINT('Ctrl Pts',(-0.134766565682532,0.0513012049880128,
0.518578591799799));
#33092=CARTESIAN_POINT('Ctrl Pts',(-0.136701386950153,0.005814759746065,
0.521226477371938));
#33093=CARTESIAN_POINT('Ctrl Pts',(0.0740036351041157,-0.103579689087084,
-0.00549926131403131));
#33094=CARTESIAN_POINT('Ctrl Pts',(0.108469063443593,-0.0789554890627202,
-0.00285137574189201));
#33095=CARTESIAN_POINT('Ctrl Pts',(0.150289960267559,0.00697358842102527,
0.00244439540238661));
#33096=CARTESIAN_POINT('Ctrl Pts',(0.0754177245648256,0.130350959440424,
0.0103880521188046));
#33097=CARTESIAN_POINT('Ctrl Pts',(-0.0686305290079791,0.133885273559895,
0.0183317088352224));
#33098=CARTESIAN_POINT('Ctrl Pts',(-0.149752027927918,0.0149194227595303,
0.0262753655516404));
#33099=CARTESIAN_POINT('Ctrl Pts',(-0.0936553304388222,-0.117820164357962,
0.0342190222680582));
#33100=CARTESIAN_POINT('Ctrl Pts',(0.0482777357162085,-0.142534141023999,
0.0421626789844763));
#33101=CARTESIAN_POINT('Ctrl Pts',(0.145963511846947,-0.036655356268332,
0.050106335700894));
#33102=CARTESIAN_POINT('Ctrl Pts',(0.1098883156172,0.102829743898569,0.0580499924173122));
#33103=CARTESIAN_POINT('Ctrl Pts',(-0.0268917335099817,0.14807215694308,
0.0659936491337298));
#33104=CARTESIAN_POINT('Ctrl Pts',(-0.139027045104252,0.0576227776510703,
0.073937305850148));
#33105=CARTESIAN_POINT('Ctrl Pts',(-0.123755948978222,-0.0856352487256572,
0.0818809625665656));
#33106=CARTESIAN_POINT('Ctrl Pts',(0.00492741522215772,-0.150414534436879,
0.0898246192829839));
#33107=CARTESIAN_POINT('Ctrl Pts',(0.129095110802064,-0.0773519516565369,
0.0977682759994015));
#33108=CARTESIAN_POINT('Ctrl Pts',(0.134957883094489,0.0665976002541865,
0.10571193271582));
#33109=CARTESIAN_POINT('Ctrl Pts',(0.0171429060285707,0.14951580334048,
0.113655589432237));
#33110=CARTESIAN_POINT('Ctrl Pts',(-0.116382109817192,0.0954152433547932,
0.121599246148655));
#33111=CARTESIAN_POINT('Ctrl Pts',(-0.1432525695092,-0.046125529563486,
0.129542902865073));
#33112=CARTESIAN_POINT('Ctrl Pts',(-0.0388439106014103,-0.14539605120302,
0.137486559581491));
#33113=CARTESIAN_POINT('Ctrl Pts',(0.101161972846149,-0.111423147476419,
0.145430216297909));
#33114=CARTESIAN_POINT('Ctrl Pts',(0.148461288415133,0.0246598485140348,
0.153373873014327));
#33115=CARTESIAN_POINT('Ctrl Pts',(0.0597081294086373,0.138144132394173,
0.161317529730745));
#33116=CARTESIAN_POINT('Ctrl Pts',(-0.0837625843453943,0.125030763063784,
0.169261186447163));
#33117=CARTESIAN_POINT('Ctrl Pts',(-0.150471827652945,-0.00266294545074625,
0.177204843163581));
#33118=CARTESIAN_POINT('Ctrl Pts',(-0.0792861042094436,-0.127916284519489,
0.185148499879999));
#33119=CARTESIAN_POINT('Ctrl Pts',(0.0645587665352683,-0.13594494422742,
0.193092156596417));
#33120=CARTESIAN_POINT('Ctrl Pts',(0.149240875090081,-0.01939132254705,
0.201035813312835));
#33121=CARTESIAN_POINT('Ctrl Pts',(0.0971560830332309,0.114932840016463,
0.208979470029252));
#33122=CARTESIAN_POINT('Ctrl Pts',(-0.0439642118092888,0.143930574476409,
0.216923126745671));
#33123=CARTESIAN_POINT('Ctrl Pts',(-0.144794948028593,0.0410278589841287,
0.224866783462088));
#33124=CARTESIAN_POINT('Ctrl Pts',(-0.112933107548683,-0.0994734909739605,
0.232810440178506));
#33125=CARTESIAN_POINT('Ctrl Pts',(0.0224225719012751,-0.148815625715515,
0.240754096894924));
#33126=CARTESIAN_POINT('Ctrl Pts',(0.137229821435604,-0.0617805656840178,
0.248697753611342));
#33127=CARTESIAN_POINT('Ctrl Pts',(0.126277306185642,0.081871265594307,
0.25664141032776));
#33128=CARTESIAN_POINT('Ctrl Pts',(-0.000397900804215911,0.150494863242789,
0.264585067044178));
#33129=CARTESIAN_POINT('Ctrl Pts',(-0.126708464664056,0.0812023840164973,
0.272528723760596));
#33130=CARTESIAN_POINT('Ctrl Pts',(-0.136901215752127,-0.0625053542775162,
0.280472380477014));
#33131=CARTESIAN_POINT('Ctrl Pts',(-0.0216353419447375,-0.148932112608676,
0.288416037193432));
#33132=CARTESIAN_POINT('Ctrl Pts',(0.113457530724511,-0.0988749255844029,
0.29635969390985));
#33133=CARTESIAN_POINT('Ctrl Pts',(0.144575974027448,0.0417929410682694,
0.304303350626268));
#33134=CARTESIAN_POINT('Ctrl Pts',(0.0432025121524296,0.144161038870872,
0.312247007342686));
#33135=CARTESIAN_POINT('Ctrl Pts',(-0.0977624736752833,0.114417485240091,
0.320190664059103));
#33136=CARTESIAN_POINT('Ctrl Pts',(-0.149136249968981,-0.0201802166177978,
0.328134320775522));
#33137=CARTESIAN_POINT('Ctrl Pts',(-0.0638390058162424,-0.136284421348793,
0.336077977491939));
#33138=CARTESIAN_POINT('Ctrl Pts',(0.0799613992688094,-0.127495242353059,
0.344021634208357));
#33139=CARTESIAN_POINT('Ctrl Pts',(0.150483805397878,-0.00186723365027712,
0.351965290924775));
#33140=CARTESIAN_POINT('Ctrl Pts',(0.0831002675312467,0.125471939367544,
0.359908947641193));
#33141=CARTESIAN_POINT('Ctrl Pts',(-0.0604377810765522,0.137826473890756,
0.367852604357611));
#33142=CARTESIAN_POINT('Ctrl Pts',(-0.148589611907278,0.0238744586728436,
0.375796261074029));
#33143=CARTESIAN_POINT('Ctrl Pts',(-0.100571365962569,-0.111956515865154,
0.383739917790446));
#33144=CARTESIAN_POINT('Ctrl Pts',(0.0396121973075005,-0.145188625494464,
0.391683574506865));
#33145=CARTESIAN_POINT('Ctrl Pts',(0.143494480612217,-0.0453673691521286,
0.399627231223282));
#33146=CARTESIAN_POINT('Ctrl Pts',(0.115875923983247,0.0960292919722012,
0.407570887939701));
#33147=CARTESIAN_POINT('Ctrl Pts',(-0.0179332546906655,0.149423120517415,
0.415514544656118));
#33148=CARTESIAN_POINT('Ctrl Pts',(-0.135308213289508,0.0658829224797566,
0.423458201372536));
#33149=CARTESIAN_POINT('Ctrl Pts',(-0.128684169075867,-0.0780333019927274,
0.431401858088955));
#33150=CARTESIAN_POINT('Ctrl Pts',(-0.0041321849285115,-0.150438877221023,
0.439345514805372));
#33151=CARTESIAN_POINT('Ctrl Pts',(0.124207444980571,-0.0849789055356846,
0.44728917152179));
#33152=CARTESIAN_POINT('Ctrl Pts',(0.13871964211393,0.0583557185263908,
0.455232828238208));
#33153=CARTESIAN_POINT('Ctrl Pts',(0.0261098129416626,0.148214964857068,
0.463176484954626));
#33154=CARTESIAN_POINT('Ctrl Pts',(-0.110433266390416,0.10224214203642,
0.471120141671043));
#33155=CARTESIAN_POINT('Ctrl Pts',(-0.145762439740054,-0.0374170052831618,
0.479063798387463));
#33156=CARTESIAN_POINT('Ctrl Pts',(-0.0475332501860763,-0.142805819824299,
0.487007455103879));
#33157=CARTESIAN_POINT('Ctrl Pts',(0.0942958542259076,-0.117288323885235,
0.494951111820298));
#33158=CARTESIAN_POINT('Ctrl Pts',(0.149635107159208,0.0156445100139045,
0.502894768536715));
#33159=CARTESIAN_POINT('Ctrl Pts',(0.0679913965801436,0.134374014588598,
0.510838425253134));
#33160=CARTESIAN_POINT('Ctrl Pts',(-0.0762513070870269,0.129697499051486,
0.518782081969551));
#33161=CARTESIAN_POINT('Ctrl Pts',(-0.125384862498713,0.0477298987390752,
0.52407785311383));
#33162=CARTESIAN_POINT('Ctrl Pts',(-0.127184992207232,0.00540996832211942,
0.526725738685969));
#33163=CARTESIAN_POINT('Ctrl Pts',(0.0684664424539458,-0.0958295198918399,
-1.2490009027033E-16));
#33164=CARTESIAN_POINT('Ctrl Pts',(0.100353055357967,-0.0730477825951437,
0.00264788557213918));
#33165=CARTESIAN_POINT('Ctrl Pts',(0.139044776673305,0.00645180185613777,
0.00794365671641779));
#33166=CARTESIAN_POINT('Ctrl Pts',(0.0697747251423586,0.120597676732883,
0.0158873134328358));
#33167=CARTESIAN_POINT('Ctrl Pts',(-0.0634953696301243,0.123867541975778,
0.0238309701492536));
#33168=CARTESIAN_POINT('Ctrl Pts',(-0.138547094180758,0.0138031030283078,
0.0317746268656716));
#33169=CARTESIAN_POINT('Ctrl Pts',(-0.0866477340332458,-0.109004476490645,
0.0397182835820895));
#33170=CARTESIAN_POINT('Ctrl Pts',(0.0446654385229893,-0.131869273048715,
0.0476619402985074));
#33171=CARTESIAN_POINT('Ctrl Pts',(0.135042047193827,-0.033912683303242,
0.0556055970149253));
#33172=CARTESIAN_POINT('Ctrl Pts',(0.101666114468308,0.0951356880412728,
0.0635492537313433));
#33173=CARTESIAN_POINT('Ctrl Pts',(-0.0248796065525388,0.136992916606216,
0.0714929104477611));
#33174=CARTESIAN_POINT('Ctrl Pts',(-0.128624589451322,0.0533112540287094,
0.079436567164179));
#33175=CARTESIAN_POINT('Ctrl Pts',(-0.114496126401493,-0.079227740916452,
0.087380223880597));
#33176=CARTESIAN_POINT('Ctrl Pts',(0.00455872999049264,-0.139160029798142,
0.0953238805970148));
#33177=CARTESIAN_POINT('Ctrl Pts',(0.119435794773867,-0.0715642270726515,
0.103267537313433));
#33178=CARTESIAN_POINT('Ctrl Pts',(0.124859895376695,0.0616145512171006,
0.111211194029851));
#33179=CARTESIAN_POINT('Ctrl Pts',(0.0158602180480347,0.138328544685192,
0.119154850746269));
#33180=CARTESIAN_POINT('Ctrl Pts',(-0.107674021867399,0.0882759645413252,
0.127098507462686));
#33181=CARTESIAN_POINT('Ctrl Pts',(-0.132533946378209,-0.0426742674339329,
0.135042164179105));
#33182=CARTESIAN_POINT('Ctrl Pts',(-0.03593748288359,-0.134517045800752,
0.142985820895522));
#33183=CARTESIAN_POINT('Ctrl Pts',(0.0935927050428541,-0.103086105216301,
0.150929477611941));
#33184=CARTESIAN_POINT('Ctrl Pts',(0.137352931996012,0.0228147184504364,
0.158873134328358));
#33185=CARTESIAN_POINT('Ctrl Pts',(0.0552405729858772,0.127807739141585,
0.166816791044776));
#33186=CARTESIAN_POINT('Ctrl Pts',(-0.0774951953753252,0.115675554751273,
0.174760447761194));
#33187=CARTESIAN_POINT('Ctrl Pts',(-0.139213036149455,-0.00246369521179678,
0.182704104477612));
#33188=CARTESIAN_POINT('Ctrl Pts',(-0.0733536600413758,-0.118345172107485,
0.19064776119403));
#33189=CARTESIAN_POINT('Ctrl Pts',(0.0597282696676458,-0.12577310138558,
0.198591417910448));
#33190=CARTESIAN_POINT('Ctrl Pts',(0.138074187460599,-0.0179404007303906,
0.206535074626866));
#33191=CARTESIAN_POINT('Ctrl Pts',(0.0898865489335327,0.106333191146418,
0.214478731343283));
#33192=CARTESIAN_POINT('Ctrl Pts',(-0.0406746665030564,0.133161220808791,
0.222422388059702));
#33193=CARTESIAN_POINT('Ctrl Pts',(-0.133960919120719,0.0379580211457631,
0.230366044776119));
#33194=CARTESIAN_POINT('Ctrl Pts',(-0.104483085165326,-0.0920305608755558,
0.238309701492537));
#33195=CARTESIAN_POINT('Ctrl Pts',(0.0207448421498254,-0.137680756627218,
0.246253358208955));
#33196=CARTESIAN_POINT('Ctrl Pts',(0.126961839902422,-0.0571579428392388,
0.254197014925373));
#33197=CARTESIAN_POINT('Ctrl Pts',(0.116828827462796,0.075745391244066,
0.262140671641791));
#33198=CARTESIAN_POINT('Ctrl Pts',(-0.000368128572008151,0.139234348141551,
0.270084328358209));
#33199=CARTESIAN_POINT('Ctrl Pts',(-0.117227725261659,0.0751265575612168,
0.278027985074627));
#33200=CARTESIAN_POINT('Ctrl Pts',(-0.12665782156486,-0.0578285003930446,
0.285971641791045));
#33201=CARTESIAN_POINT('Ctrl Pts',(-0.0200165152988323,-0.137788527592198,
0.293915298507463));
#33202=CARTESIAN_POINT('Ctrl Pts',(0.104968269293632,-0.0914767820950745,
0.301858955223881));
#33203=CARTESIAN_POINT('Ctrl Pts',(0.133758329466478,0.0386658573002006,
0.309802611940298));
#33204=CARTESIAN_POINT('Ctrl Pts',(0.0399699596916912,0.133374441107753,
0.317746268656717));
#33205=CARTESIAN_POINT('Ctrl Pts',(-0.0904475674556682,0.10585639689043,
0.325689925373134));
#33206=CARTESIAN_POINT('Ctrl Pts',(-0.137977390731318,-0.0186702671811566,
0.333633582089553));
#33207=CARTESIAN_POINT('Ctrl Pts',(-0.0590623637863932,-0.126087177724698,
0.34157723880597));
#33208=CARTESIAN_POINT('Ctrl Pts',(0.0739784273282333,-0.117955633685244,
0.349520895522388));
#33209=CARTESIAN_POINT('Ctrl Pts',(0.139224117680559,-0.00172752115601949,
0.357464552238807));
#33210=CARTESIAN_POINT('Ctrl Pts',(0.0768824352591712,0.11608372080921,
0.365408208955224));
#33211=CARTESIAN_POINT('Ctrl Pts',(-0.0559156297430559,0.12751384888047,
0.373351865671643));
#33212=CARTESIAN_POINT('Ctrl Pts',(-0.137471653907146,0.0220880940313751,
0.381295522388059));
#33213=CARTESIAN_POINT('Ctrl Pts',(-0.0930462892870504,-0.103579565247593,
0.389239179104478));
#33214=CARTESIAN_POINT('Ctrl Pts',(0.0366482838797405,-0.134325140358292,
0.397182835820896));
#33215=CARTESIAN_POINT('Ctrl Pts',(0.132757756905765,-0.0419728350502109,
0.405126492537314));
#33216=CARTESIAN_POINT('Ctrl Pts',(0.107205710503746,0.0888440680441954,
0.413070149253731));
#33217=CARTESIAN_POINT('Ctrl Pts',(-0.0165914302528927,0.138242796692368,
0.42101380597015));
#33218=CARTESIAN_POINT('Ctrl Pts',(-0.125184012727194,0.0609533479579989,
0.428957462686568));
#33219=CARTESIAN_POINT('Ctrl Pts',(-0.119055601044071,-0.0721945965608292,
0.436901119402986));
#33220=CARTESIAN_POINT('Ctrl Pts',(-0.00382300141363195,-0.139182551176009,
0.444844776119403));
#33221=CARTESIAN_POINT('Ctrl Pts',(0.11491384000461,-0.0786205074584852,
0.452788432835821));
#33222=CARTESIAN_POINT('Ctrl Pts',(0.128340187352459,0.0539893538840985,
0.460732089552239));
#33223=CARTESIAN_POINT('Ctrl Pts',(0.024156191824071,0.137125039167645,
0.468675746268657));
#33224=CARTESIAN_POINT('Ctrl Pts',(-0.102170290252407,0.094592052461424,
0.476619402985075));
#33225=CARTESIAN_POINT('Ctrl Pts',(-0.13485601995589,-0.0346173432617789,
0.484563059701493));
#33226=CARTESIAN_POINT('Ctrl Pts',(-0.0439766578214066,-0.132120623957634,
0.492506716417911));
#33227=CARTESIAN_POINT('Ctrl Pts',(0.087240331747497,-0.108512430051717,
0.500450373134329));
#33228=CARTESIAN_POINT('Ctrl Pts',(0.138438921804208,0.0144739368962113,
0.508394029850746));
#33229=CARTESIAN_POINT('Ctrl Pts',(0.0629040591690992,0.12431971381125,
0.516337686567165));
#33230=CARTESIAN_POINT('Ctrl Pts',(-0.0705459363093062,0.119993110375402,
0.524281343283582));
#33231=CARTESIAN_POINT('Ctrl Pts',(-0.116003159314893,0.0441585924901374,
0.529577114427861));
#33232=CARTESIAN_POINT('Ctrl Pts',(-0.117668597464311,0.00500517689817385,
0.532225));
#33233=CARTESIAN_POINT('',(0.0684664424539457,-0.0958295198918399,0.));
#33234=CARTESIAN_POINT('Ctrl Pts',(0.0684664424539458,-0.0958295198918399,
-1.2490009027033E-16));
#33235=CARTESIAN_POINT('Ctrl Pts',(0.100353055357967,-0.0730477825951437,
0.00264788557213918));
#33236=CARTESIAN_POINT('Ctrl Pts',(0.139044776673305,0.00645180185613777,
0.00794365671641779));
#33237=CARTESIAN_POINT('Ctrl Pts',(0.0697747251423586,0.120597676732883,
0.0158873134328358));
#33238=CARTESIAN_POINT('Ctrl Pts',(-0.0634953696301243,0.123867541975778,
0.0238309701492536));
#33239=CARTESIAN_POINT('Ctrl Pts',(-0.116013612970437,0.0468487789511056,
0.0293896285137698));
#33240=CARTESIAN_POINT('Ctrl Pts',(-0.117946226519694,0.00395164958315818,
0.0323004013061468));
#33241=CARTESIAN_POINT('Ctrl Pts',(-0.117919967015755,7.48285734863559E-5,
0.0325632885263843));
#33242=CARTESIAN_POINT('Ctrl Pts',(0.0635548502597316,0.132093933345895,
7.26415455565288E-18));
#33243=CARTESIAN_POINT('Ctrl Pts',(0.0667625318922158,0.13018322972067,
8.97431508554919E-18));
#33244=CARTESIAN_POINT('Ctrl Pts',(0.0698866263065284,0.128144700630429,
-1.82766240468292E-17));
#33245=CARTESIAN_POINT('Ctrl Pts',(0.0729183991770622,0.125977863427922,
-1.55040910665427E-17));
#33246=CARTESIAN_POINT('Ctrl Pts',(0.0787736058599248,0.121793090949712,
-9.35723626730848E-18));
#33247=CARTESIAN_POINT('Ctrl Pts',(0.0842851176408076,0.117130107773036,
-2.42858544627756E-17));
#33248=CARTESIAN_POINT('Ctrl Pts',(0.0894225077026563,0.112048986470911,
-3.0140820395097E-17));
#33249=CARTESIAN_POINT('Ctrl Pts',(0.0927550575340165,0.108752937361409,
-3.39388512036349E-17));
#33250=CARTESIAN_POINT('Ctrl Pts',(0.095930929613759,0.105278801629612,
-4.52445550988079E-17));
#33251=CARTESIAN_POINT('Ctrl Pts',(0.0989262797420343,0.101660133512415,
-3.46944695195361E-17));
#33252=CARTESIAN_POINT('Ctrl Pts',(0.103069367071931,0.0966548895891983,
-2.01018763264428E-17));
#33253=CARTESIAN_POINT('Ctrl Pts',(0.106874603061403,0.0913668016366946,
-3.77038544403596E-17));
#33254=CARTESIAN_POINT('Ctrl Pts',(0.110317478847291,0.0858396385675292,
-3.33934269125535E-17));
#33255=CARTESIAN_POINT('Ctrl Pts',(0.112268215177796,0.082707943300496,
-3.09511350317464E-17));
#33256=CARTESIAN_POINT('Ctrl Pts',(0.114103333501928,0.079497785539906,
-4.97099315558713E-17));
#33257=CARTESIAN_POINT('Ctrl Pts',(0.115814486180912,0.0762220963964089,
-4.59701721133854E-17));
#33258=CARTESIAN_POINT('Ctrl Pts',(0.120425861906472,0.0673944601566279,
-3.58919154362862E-17));
#33259=CARTESIAN_POINT('Ctrl Pts',(0.124112940735196,0.0581470311761757,
-7.4029188042833E-18));
#33260=CARTESIAN_POINT('Ctrl Pts',(0.126786742395323,0.0486381528803429,
-1.99493199737333E-17));
#33261=CARTESIAN_POINT('Ctrl Pts',(0.128289456800478,0.0432940285927791,
-2.70005751402403E-17));
#33262=CARTESIAN_POINT('Ctrl Pts',(0.129471235246761,0.0378670663167402,
-8.81130640021771E-18));
#33263=CARTESIAN_POINT('Ctrl Pts',(0.130308765287913,0.0323855967712197,
-1.47451495458029E-17));
#33264=CARTESIAN_POINT('Ctrl Pts',(0.130909407220836,0.0284545133457784,
-1.90006566219738E-17));
#33265=CARTESIAN_POINT('Ctrl Pts',(0.131332629221345,0.0244917931761562,
-4.99383881545994E-18));
#33266=CARTESIAN_POINT('Ctrl Pts',(0.1315678106143,0.0205341495544984,-6.07153216591882E-18));
#33267=CARTESIAN_POINT('Ctrl Pts',(0.131851015138327,0.015768370408227,
-7.36928633144951E-18));
#33268=CARTESIAN_POINT('Ctrl Pts',(0.131863254926577,0.0110027231344166,
-1.87693227394301E-17));
#33269=CARTESIAN_POINT('Ctrl Pts',(0.131591710623677,0.00625556877829329,
-1.38777878078145E-17));
#33270=CARTESIAN_POINT('Ctrl Pts',(0.131146495407245,-0.00152771126671145,
-5.8577860622257E-18));
#33271=CARTESIAN_POINT('Ctrl Pts',(0.12993932260643,-0.00926206422336292,
-1.85374582714576E-17));
#33272=CARTESIAN_POINT('Ctrl Pts',(0.128016835267175,-0.0168585737917118,
-1.04083408558608E-17));
#33273=CARTESIAN_POINT('Ctrl Pts',(0.126984115402176,-0.0209392593575938,
-6.04154952851233E-18));
#33274=CARTESIAN_POINT('Ctrl Pts',(0.125742427413826,-0.0249846391579523,
1.89772622437785E-17));
#33275=CARTESIAN_POINT('Ctrl Pts',(0.124308621487175,-0.0289511201777135,
1.38777878078145E-17));
#33276=CARTESIAN_POINT('Ctrl Pts',(0.121785637190381,-0.0359307044717815,
4.90454136999372E-18));
#33277=CARTESIAN_POINT('Ctrl Pts',(0.118666317325564,-0.042682712152767,
2.07260850608487E-18));
#33278=CARTESIAN_POINT('Ctrl Pts',(0.114994151346376,-0.0491304207397526,
8.67361737988404E-18));
#33279=CARTESIAN_POINT('Ctrl Pts',(0.112470213235982,-0.0535620334499726,
1.32105958166033E-17));
#33280=CARTESIAN_POINT('Ctrl Pts',(0.109684704250007,-0.0578497076893306,
-2.69424258846107E-17));
#33281=CARTESIAN_POINT('Ctrl Pts',(0.106648013733876,-0.0619641182107045,
-2.60208521396521E-17));
#33282=CARTESIAN_POINT('Ctrl Pts',(0.104460102807982,-0.0649285176730499,
-2.53568657192706E-17));
#33283=CARTESIAN_POINT('Ctrl Pts',(0.102139560475227,-0.0678046962501359,
-1.87244270863087E-17));
#33284=CARTESIAN_POINT('Ctrl Pts',(0.0997061632112326,-0.0705633954799611,
-1.90819582357449E-17));
#33285=CARTESIAN_POINT('Ctrl Pts',(0.0939222145804643,-0.0771205552455056,
-1.9931775005426E-17));
#33286=CARTESIAN_POINT('Ctrl Pts',(0.087486631308301,-0.0830406987797476,
-2.77894727952103E-19));
#33287=CARTESIAN_POINT('Ctrl Pts',(0.0804584136226653,-0.0881761753022089,
-1.73472347597681E-18));
#33288=CARTESIAN_POINT('Ctrl Pts',(0.0766344364937381,-0.0909703324621629,
-2.52736822068868E-18));
#33289=CARTESIAN_POINT('Ctrl Pts',(0.0726345968903183,-0.0935314830199203,
-1.19936303452846E-17));
#33290=CARTESIAN_POINT('Ctrl Pts',(0.0684664424539472,-0.0958295198918389,
-1.04083408558608E-17));
#33291=CARTESIAN_POINT('Ctrl Pts',(-0.00157033164522019,0.146071601053478,
0.50365));
#33292=CARTESIAN_POINT('Ctrl Pts',(0.0218930565124332,0.146360870028846,
0.502379967541691));
#33293=CARTESIAN_POINT('Ctrl Pts',(0.0454120282149095,0.141318853716995,
0.501109935083381));
#33294=CARTESIAN_POINT('Ctrl Pts',(0.0661716191392787,0.130837066204352,
0.499839902625071));
#33295=CARTESIAN_POINT('Ctrl Pts',(0.109453206891224,0.108983629511958,
0.497192017052932));
#33296=CARTESIAN_POINT('Ctrl Pts',(0.140740342380216,0.0634846428806245,
0.494544131480792));
#33297=CARTESIAN_POINT('Ctrl Pts',(0.145780480343632,0.0152641882646972,
0.491896245908653));
#33298=CARTESIAN_POINT('Ctrl Pts',(0.150820618307048,-0.0329562663512301,
0.489248360336514));
#33299=CARTESIAN_POINT('Ctrl Pts',(0.129613758744889,-0.0838981889517511,
0.486600474764375));
#33300=CARTESIAN_POINT('Ctrl Pts',(0.0918347732807851,-0.114258500252904,
0.483952589192235));
#33301=CARTESIAN_POINT('Ctrl Pts',(0.0540557878166811,-0.144618811554058,
0.481304703620096));
#33302=CARTESIAN_POINT('Ctrl Pts',(-0.000295323549367926,-0.154397511555843,
0.478656818047957));
#33303=CARTESIAN_POINT('Ctrl Pts',(-0.0462923532978867,-0.139093547851452,
0.476008932475817));
#33304=CARTESIAN_POINT('Ctrl Pts',(-0.0922893830464049,-0.123789584147061,
0.473361046903678));
#33305=CARTESIAN_POINT('Ctrl Pts',(-0.129932331177393,-0.0834029567364939,
0.470713161331538));
#33306=CARTESIAN_POINT('Ctrl Pts',(-0.141984461802563,-0.0364498679458208,
0.468065275759399));
#33307=CARTESIAN_POINT('Ctrl Pts',(-0.145018518318758,-0.0246296902999453,
0.467398685367696));
#33308=CARTESIAN_POINT('Ctrl Pts',(-0.146430750426956,-0.0123933615350992,
0.466732094975993));
#33309=CARTESIAN_POINT('Ctrl Pts',(-0.146320034481408,-0.000132042578932776,
0.466065504584291));
#33310=CARTESIAN_POINT('Origin',(0.,0.,-0.0924367114736154));
#33311=CARTESIAN_POINT('',(-0.0684664424539447,-0.0958295198918406,0.));
#33312=CARTESIAN_POINT('Ctrl Pts',(-0.0686153921261821,-0.095961513397809,
-8.6871699070401E-17));
#33313=CARTESIAN_POINT('Ctrl Pts',(-0.0390777571216276,-0.11683521110507,
0.00245324280107157));
#33314=CARTESIAN_POINT('Ctrl Pts',(0.0440758903380829,-0.130444567971902,
0.00755732030717748));
#33315=CARTESIAN_POINT('Ctrl Pts',(0.134343829836486,-0.03677094505856,
0.0153122325183177));
#33316=CARTESIAN_POINT('Ctrl Pts',(0.103577487134497,0.0931457228401511,
0.0232647366334205));
#33317=CARTESIAN_POINT('Ctrl Pts',(-0.022319455813322,0.137480661654608,
0.0312172407485234));
#33318=CARTESIAN_POINT('Ctrl Pts',(-0.107013184840641,0.0716760847082379,
0.0376078990285884));
#33319=CARTESIAN_POINT('Ctrl Pts',(-0.117673522927843,0.0162276125558733,
0.0413477226036194));
#33320=CARTESIAN_POINT('Ctrl Pts',(-0.117605093279175,5.6374090473453E-5,
0.042436711473616));
#33321=CARTESIAN_POINT('Origin',(0.,0.,0.));
#33322=CARTESIAN_POINT('Ctrl Pts',(-0.0510216505388437,0.106149619882937,
-0.0164977839420935));
#33323=CARTESIAN_POINT('Ctrl Pts',(-0.0863815445949669,0.0891536084077042,
-0.0138469492370593));
#33324=CARTESIAN_POINT('Ctrl Pts',(-0.138162556478479,0.0173380738482791,
-0.00854527982699074));
#33325=CARTESIAN_POINT('Ctrl Pts',(-0.0892152289856901,-0.107087400898305,
-0.000592775711887911));
#33326=CARTESIAN_POINT('Ctrl Pts',(0.0417759011768067,-0.132831332515275,
0.00735972840321487));
#33327=CARTESIAN_POINT('Ctrl Pts',(0.134343829836486,-0.03677094505856,
0.0153122325183177));
#33328=CARTESIAN_POINT('Ctrl Pts',(0.103577487134497,0.0931457228401511,
0.0232647366334205));
#33329=CARTESIAN_POINT('Ctrl Pts',(-0.022319455813322,0.137480661654608,
0.0312172407485234));
#33330=CARTESIAN_POINT('Ctrl Pts',(-0.127711920735776,0.0555937658099327,
0.0391697448636261));
#33331=CARTESIAN_POINT('Ctrl Pts',(-0.115832853027164,-0.0773572203301017,
0.047122248978729));
#33332=CARTESIAN_POINT('Ctrl Pts',(0.00241643506700816,-0.139265216174241,
0.0550747530938317));
#33333=CARTESIAN_POINT('Ctrl Pts',(0.118445458723555,-0.0732914200146354,
0.0630272572089346));
#33334=CARTESIAN_POINT('Ctrl Pts',(0.125708256673902,0.0599868231457294,
0.0709797613240373));
#33335=CARTESIAN_POINT('Ctrl Pts',(0.0175344664057042,0.138178956948752,
0.0789322654391402));
#33336=CARTESIAN_POINT('Ctrl Pts',(-0.106740805893122,0.0894837054538652,
0.0868847695542431));
#33337=CARTESIAN_POINT('Ctrl Pts',(-0.132997503503664,-0.0413835288220579,
0.0948372736693457));
#33338=CARTESIAN_POINT('Ctrl Pts',(-0.0371242974264225,-0.134248668971966,
0.102789777784449));
#33339=CARTESIAN_POINT('Ctrl Pts',(0.0928396337021713,-0.10383510521762,
0.110742281899551));
#33340=CARTESIAN_POINT('Ctrl Pts',(0.137550169005636,0.0219289054269618,
0.118694786014654));
#33341=CARTESIAN_POINT('Ctrl Pts',(0.0559501922162531,0.127555870431356,
0.126647290129757));
#33342=CARTESIAN_POINT('Ctrl Pts',(-0.0770281035821754,0.116049974518826,
0.13459979424486));
#33343=CARTESIAN_POINT('Ctrl Pts',(-0.13927251071013,-0.00202308703008076,
0.142552298359963));
#33344=CARTESIAN_POINT('Ctrl Pts',(-0.0736248085349355,-0.118238371369349,
0.150504802475065));
#33345=CARTESIAN_POINT('Ctrl Pts',(0.0596315829014974,-0.125876921640408,
0.158457306590168));
#33346=CARTESIAN_POINT('Ctrl Pts',(0.138129079193178,-0.0179243554725553,
0.166409810705271));
#33347=CARTESIAN_POINT('Ctrl Pts',(0.0897844651888838,0.106487909275724,
0.174362314820374));
#33348=CARTESIAN_POINT('Ctrl Pts',(-0.0410080379701501,0.133113732800722,
0.182314818935477));
#33349=CARTESIAN_POINT('Ctrl Pts',(-0.134143401206605,0.0375029724551737,
0.190267323050579));
#33350=CARTESIAN_POINT('Ctrl Pts',(-0.104096649768354,-0.0925462723956308,
0.198219827165683));
#33351=CARTESIAN_POINT('Ctrl Pts',(0.0215406810767683,-0.137611496939632,
0.206172331280785));
#33352=CARTESIAN_POINT('Ctrl Pts',(0.127397488829925,-0.056309900280862,
0.214124835395888));
#33353=CARTESIAN_POINT('Ctrl Pts',(0.116266864218555,0.0767003345124148,
0.222077339510991));
#33354=CARTESIAN_POINT('Ctrl Pts',(-0.0016300870944122,0.139277664563073,
0.230029843626094));
#33355=CARTESIAN_POINT('Ctrl Pts',(-0.1180301509465,0.0739581536911037,
0.237982347741196));
#33356=CARTESIAN_POINT('Ctrl Pts',(-0.126044685167542,-0.0592761534753867,
0.245934851856299));
#33357=CARTESIAN_POINT('Ctrl Pts',(-0.0183140487741412,-0.138077951344142,
0.253887355971402));
#33358=CARTESIAN_POINT('Ctrl Pts',(0.106234136865658,-0.0900845891054932,
0.261839860086505));
#33359=CARTESIAN_POINT('Ctrl Pts',(0.133228916899009,0.040632262203075,
0.269792364201608));
#33360=CARTESIAN_POINT('Ctrl Pts',(0.0378813411502606,0.134037043471229,
0.27774486831671));
#33361=CARTESIAN_POINT('Ctrl Pts',(-0.092252170148986,0.104357376993109,
0.285697372431813));
#33362=CARTESIAN_POINT('Ctrl Pts',(-0.137671731315388,-0.021152291274371,
0.293649876546916));
#33363=CARTESIAN_POINT('Ctrl Pts',(-0.0566691588697243,-0.127238089669758,
0.301602380662019));
#33364=CARTESIAN_POINT('Ctrl Pts',(0.0763719541489209,-0.116482829853556,
0.309554884777122));
#33365=CARTESIAN_POINT('Ctrl Pts',(0.139281709756163,0.00123707506708643,
0.317507388892225));
#33366=CARTESIAN_POINT('Ctrl Pts',(0.0742909098282569,0.117820990265484,
0.325459893007327));
#33367=CARTESIAN_POINT('Ctrl Pts',(-0.0589202520252667,0.1262114453589,
0.33341239712243));
#33368=CARTESIAN_POINT('Ctrl Pts',(-0.13802572406761,0.0187035960922139,
0.341364901237533));
#33369=CARTESIAN_POINT('Ctrl Pts',(-0.0903839958430062,-0.105979518461414,
0.349317405352636));
#33370=CARTESIAN_POINT('Ctrl Pts',(0.0402561631274929,-0.133343040355529,
0.357269909467738));
#33371=CARTESIAN_POINT('Ctrl Pts',(0.133929618074243,-0.0382594079720193,
0.365222413582842));
#33372=CARTESIAN_POINT('Ctrl Pts',(0.104617274119081,0.0919573329132998,
0.373174917697944));
#33373=CARTESIAN_POINT('Ctrl Pts',(-0.020763734615072,0.137730870367254,
0.381127421813047));
#33374=CARTESIAN_POINT('Ctrl Pts',(-0.127077674436729,0.0570279646339328,
0.38907992592815));
#33375=CARTESIAN_POINT('Ctrl Pts',(-0.116697873675526,-0.0760429626350431,
0.397032430043252));
#33376=CARTESIAN_POINT('Ctrl Pts',(0.000844063931402275,-0.139284651766041,
0.404984934158356));
#33377=CARTESIAN_POINT('Ctrl Pts',(0.117610871049501,-0.0746230633995127,
0.412937438273457));
#33378=CARTESIAN_POINT('Ctrl Pts',(0.126377239427685,0.0585638604483229,
0.420889942388562));
#33379=CARTESIAN_POINT('Ctrl Pts',(0.0190929207373193,0.137972437690235,
0.428842446503664));
#33380=CARTESIAN_POINT('Ctrl Pts',(-0.105723916050958,0.0906826070998613,
0.436794950618767));
#33381=CARTESIAN_POINT('Ctrl Pts',(-0.133456368516637,-0.0398795994144927,
0.44474745473387));
#33382=CARTESIAN_POINT('Ctrl Pts',(-0.038636663810782,-0.133821400192823,
0.452699958848972));
#33383=CARTESIAN_POINT('Ctrl Pts',(0.0916608011058181,-0.104875817685159,
0.460652462964076));
#33384=CARTESIAN_POINT('Ctrl Pts',(0.137790741908166,0.0203740232160909,
0.468604967079177));
#33385=CARTESIAN_POINT('Ctrl Pts',(0.0573828398023632,0.126918127906013,
0.476557471194281));
#33386=CARTESIAN_POINT('Ctrl Pts',(-0.0757067578384881,0.11690841395886,
0.484509975309383));
#33387=CARTESIAN_POINT('Ctrl Pts',(-0.139299045817393,-0.000444250914572553,
0.492462479424487));
#33388=CARTESIAN_POINT('Ctrl Pts',(-0.0749307309976486,-0.117412744486246,
0.500414983539588));
#33389=CARTESIAN_POINT('Ctrl Pts',(0.0581614397283287,-0.126517333775439,
0.508367487654693));
#33390=CARTESIAN_POINT('Ctrl Pts',(0.138005962114904,-0.01953005209576,
0.516319991769794));
#33391=CARTESIAN_POINT('Ctrl Pts',(0.0908022345067483,0.105567300931769,
0.524272495884898));
#33392=CARTESIAN_POINT('Ctrl Pts',(0.00421962447768953,0.124065836989857,
0.529574165294966));
#33393=CARTESIAN_POINT('Ctrl Pts',(-0.0334019664626881,0.11293918390632,
0.532225));
#33394=CARTESIAN_POINT('Ctrl Pts',(-0.0551480035117362,0.114734422509853,
-0.0109985226280624));
#33395=CARTESIAN_POINT('Ctrl Pts',(-0.0933676130497917,0.096363866272985,
-0.0083476879230281));
#33396=CARTESIAN_POINT('Ctrl Pts',(-0.149336390912421,0.0187402827500406,
-0.00304601851295955));
#33397=CARTESIAN_POINT('Ctrl Pts',(-0.0964304703874203,-0.115748046141832,
0.00490648560214325));
#33398=CARTESIAN_POINT('Ctrl Pts',(0.0451545083405425,-0.143574006615959,
0.0128589897172461));
#33399=CARTESIAN_POINT('Ctrl Pts',(0.145208826475777,-0.0397447786538297,
0.0208114938323489));
#33400=CARTESIAN_POINT('Ctrl Pts',(0.1119542696856,0.100678841159424,0.0287639979474517));
#33401=CARTESIAN_POINT('Ctrl Pts',(-0.0241245317345429,0.148599348152253,
0.0367165020625545));
#33402=CARTESIAN_POINT('Ctrl Pts',(-0.138040564718016,0.060089886543023,
0.0446690061776573));
#33403=CARTESIAN_POINT('Ctrl Pts',(-0.125200782766784,-0.0836134506306251,
0.0526215102927601));
#33404=CARTESIAN_POINT('Ctrl Pts',(0.00261186316306541,-0.150528227713698,
0.0605740144078629));
#33405=CARTESIAN_POINT('Ctrl Pts',(0.128024681770397,-0.0792188305486153,
0.0685265185229658));
#33406=CARTESIAN_POINT('Ctrl Pts',(0.135874855228935,0.0648382304092657,
0.0764790226380685));
#33407=CARTESIAN_POINT('Ctrl Pts',(0.0189525584669602,0.149354117763329,
0.0844315267531714));
#33408=CARTESIAN_POINT('Ctrl Pts',(-0.115373420421943,0.096720659768857,
0.0923840308682741));
#33409=CARTESIAN_POINT('Ctrl Pts',(-0.143753616608078,-0.0447304030485916,
0.100336534983377));
#33410=CARTESIAN_POINT('Ctrl Pts',(-0.0401267082350556,-0.145105969519263,
0.10828903909848));
#33411=CARTESIAN_POINT('Ctrl Pts',(0.100347997200478,-0.112232722514991,
0.116241543213583));
#33412=CARTESIAN_POINT('Ctrl Pts',(0.148674476878943,0.0237023957618521,
0.124194047328685));
#33413=CARTESIAN_POINT('Ctrl Pts',(0.0604751387741805,0.137871893915615,
0.132146551443788));
#33414=CARTESIAN_POINT('Ctrl Pts',(-0.0832577167141655,0.125435463861147,
0.140099055558891));
#33415=CARTESIAN_POINT('Ctrl Pts',(-0.150536112191887,-0.00218670328107987,
0.148051559673994));
#33416=CARTESIAN_POINT('Ctrl Pts',(-0.0795791817151125,-0.127800846319831,
0.156004063789097));
#33417=CARTESIAN_POINT('Ctrl Pts',(0.0644542602705204,-0.136057160898527,
0.163956567904199));
#33418=CARTESIAN_POINT('Ctrl Pts',(0.149300206166772,-0.0193739796362248,
0.171909072019302));
#33419=CARTESIAN_POINT('Ctrl Pts',(0.0970457433117808,0.115100070904688,
0.179861576134405));
#33420=CARTESIAN_POINT('Ctrl Pts',(-0.0443245445434091,0.143879245897109,
0.187814080249508));
#33421=CARTESIAN_POINT('Ctrl Pts',(-0.144992188270862,0.0405360084359473,
0.195766584364611));
#33422=CARTESIAN_POINT('Ctrl Pts',(-0.11251541936329,-0.100030910430598,
0.203719088479714));
#33423=CARTESIAN_POINT('Ctrl Pts',(0.023282773942454,-0.148740764681937,
0.211671592594816));
#33424=CARTESIAN_POINT('Ctrl Pts',(0.13770070327361,-0.0608639380662604,
0.219624096709919));
#33425=CARTESIAN_POINT('Ctrl Pts',(0.125669894417509,0.0829034394687354,
0.227576600825022));
#33426=CARTESIAN_POINT('Ctrl Pts',(-0.00176191965288545,0.150541682860363,
0.235529104940125));
#33427=CARTESIAN_POINT('Ctrl Pts',(-0.127575786164206,0.0799394860104231,
0.243481609055227));
#33428=CARTESIAN_POINT('Ctrl Pts',(-0.136238492225245,-0.0640700856498972,
0.25143411317033));
#33429=CARTESIAN_POINT('Ctrl Pts',(-0.0197951892077968,-0.149244943376008,
0.259386617285433));
#33430=CARTESIAN_POINT('Ctrl Pts',(0.114825774765427,-0.0973701396147685,
0.267339121400536));
#33431=CARTESIAN_POINT('Ctrl Pts',(0.144003745457388,0.0439183780806738,
0.275291625515639));
#33432=CARTESIAN_POINT('Ctrl Pts',(0.0409449775285778,0.144877228901612,
0.283244129630741));
#33433=CARTESIAN_POINT('Ctrl Pts',(-0.0997130227974173,0.112797232784741,
0.291196633745845));
#33434=CARTESIAN_POINT('Ctrl Pts',(-0.148805870485663,-0.0228629732899794,
0.299149137860947));
#33435=CARTESIAN_POINT('Ctrl Pts',(-0.0612522515314454,-0.137528412778265,
0.30710164197605));
#33436=CARTESIAN_POINT('Ctrl Pts',(0.0825485014914671,-0.125903326175825,
0.315054146091153));
#33437=CARTESIAN_POINT('Ctrl Pts',(0.150546055206619,0.00133712295512629,
0.323006650206255));
#33438=CARTESIAN_POINT('Ctrl Pts',(0.0802991536500716,0.12734970970746,
0.330959154321359));
#33439=CARTESIAN_POINT('Ctrl Pts',(-0.0636854008305359,0.136418739071857,
0.338911658436461));
#33440=CARTESIAN_POINT('Ctrl Pts',(-0.149188492242044,0.0202162409895048,
0.346864162551565));
#33441=CARTESIAN_POINT('Ctrl Pts',(-0.0976937607371238,-0.114550564212591,
0.354816666666667));
#33442=CARTESIAN_POINT('Ctrl Pts',(0.0435118621620017,-0.144127098596976,
0.36276917078177));
#33443=CARTESIAN_POINT('Ctrl Pts',(0.144761115524102,-0.041353620334011,
0.370721674896872));
#33444=CARTESIAN_POINT('Ctrl Pts',(0.113078148973544,0.0993943407332879,
0.378674179011976));
#33445=CARTESIAN_POINT('Ctrl Pts',(-0.0224429922861266,0.148869792381672,
0.386626683127078));
#33446=CARTESIAN_POINT('Ctrl Pts',(-0.137355024035624,0.0616400755499871,
0.394579187242181));
#33447=CARTESIAN_POINT('Ctrl Pts',(-0.126135761569897,-0.0821929029373033,
0.402531691357283));
#33448=CARTESIAN_POINT('Ctrl Pts',(0.000912327221120078,-0.150549235150219,
0.410484195472387));
#33449=CARTESIAN_POINT('Ctrl Pts',(0.127122597194663,-0.0806581699915775,
0.418436699587489));
#33450=CARTESIAN_POINT('Ctrl Pts',(0.136597941661171,0.0633001862455649,
0.426389203702593));
#33451=CARTESIAN_POINT('Ctrl Pts',(0.0206370520896696,0.149130896352934,
0.434341707817695));
#33452=CARTESIAN_POINT('Ctrl Pts',(-0.114274290072485,0.0980165220446819,
0.442294211932798));
#33453=CARTESIAN_POINT('Ctrl Pts',(-0.144249592121994,-0.0431048440285699,
0.450246716047901));
#33454=CARTESIAN_POINT('Ctrl Pts',(-0.0417613865685641,-0.144644145570336,
0.458199220163003));
#33455=CARTESIAN_POINT('Ctrl Pts',(0.0990738270496334,-0.113357602133906,
0.466151724278107));
#33456=CARTESIAN_POINT('Ctrl Pts',(0.148934506006449,0.0220217631535408,
0.474104228393209));
#33457=CARTESIAN_POINT('Ctrl Pts',(0.0620236510875902,0.137182574251203,
0.482056732508312));
#33458=CARTESIAN_POINT('Ctrl Pts',(-0.0818295077294796,0.126363329203676,
0.490009236623415));
#33459=CARTESIAN_POINT('Ctrl Pts',(-0.150564793313981,-0.000480179506898605,
0.497961740738518));
#33460=CARTESIAN_POINT('Ctrl Pts',(-0.0809907200679325,-0.126908447234973,
0.50591424485362));
#33461=CARTESIAN_POINT('Ctrl Pts',(0.0628652199313619,-0.136749366076106,
0.513866748968723));
#33462=CARTESIAN_POINT('Ctrl Pts',(0.149167132050327,-0.0211095362495466,
0.521819253083827));
#33463=CARTESIAN_POINT('Ctrl Pts',(0.0981458242641405,0.114105008776176,
0.529771757198928));
#33464=CARTESIAN_POINT('Ctrl Pts',(0.00456088470396912,0.134099605593792,
0.535073426608997));
#33465=CARTESIAN_POINT('Ctrl Pts',(-0.0361033354336669,0.122073089461044,
0.537724261314032));
#33466=CARTESIAN_POINT('Ctrl Pts',(-0.0592743564846287,0.123319225136769,
-0.00549926131403118));
#33467=CARTESIAN_POINT('Ctrl Pts',(-0.100353681504617,0.103574124138266,
-0.00284842660899691));
#33468=CARTESIAN_POINT('Ctrl Pts',(-0.160510225346362,0.0201424916518021,
0.00245324280107164));
#33469=CARTESIAN_POINT('Ctrl Pts',(-0.103645711789151,-0.124408691385358,
0.0104057469161744));
#33470=CARTESIAN_POINT('Ctrl Pts',(0.0485331155042784,-0.154316680716642,
0.0183582510312773));
#33471=CARTESIAN_POINT('Ctrl Pts',(0.156073823115068,-0.0427186122490994,
0.02631075514638));
#33472=CARTESIAN_POINT('Ctrl Pts',(0.120331052236703,0.108211959478697,
0.0342632592614829));
#33473=CARTESIAN_POINT('Ctrl Pts',(-0.0259296076557639,0.159718034649898,
0.0422157633765857));
#33474=CARTESIAN_POINT('Ctrl Pts',(-0.148369208700255,0.0645860072761131,
0.0501682674916885));
#33475=CARTESIAN_POINT('Ctrl Pts',(-0.134568712506405,-0.0898696809311483,
0.0581207716067913));
#33476=CARTESIAN_POINT('Ctrl Pts',(0.00280729125912282,-0.161791239253156,
0.0660732757218941));
#33477=CARTESIAN_POINT('Ctrl Pts',(0.137603904817239,-0.0851462410825952,
0.074025779836997));
#33478=CARTESIAN_POINT('Ctrl Pts',(0.146041453783967,0.0696896376728019,
0.0819782839520996));
#33479=CARTESIAN_POINT('Ctrl Pts',(0.0203706505282163,0.160529278577907,
0.0899307880672026));
#33480=CARTESIAN_POINT('Ctrl Pts',(-0.124006034950765,0.103957614083849,
0.0978832921823053));
#33481=CARTESIAN_POINT('Ctrl Pts',(-0.154509729712493,-0.0480772772751253,
0.105835796297408));
#33482=CARTESIAN_POINT('Ctrl Pts',(-0.0431291190436888,-0.155963270066561,
0.113788300412511));
#33483=CARTESIAN_POINT('Ctrl Pts',(0.107856360698785,-0.120630339812362,
0.121740804527614));
#33484=CARTESIAN_POINT('Ctrl Pts',(0.159798784752249,0.0254758860967424,
0.129693308642717));
#33485=CARTESIAN_POINT('Ctrl Pts',(0.065000085332108,0.148187917399874,
0.137645812757819));
#33486=CARTESIAN_POINT('Ctrl Pts',(-0.0894873298461556,0.134820953203468,
0.145598316872922));
#33487=CARTESIAN_POINT('Ctrl Pts',(-0.161799713673645,-0.00235031953207901,
0.153550820988025));
#33488=CARTESIAN_POINT('Ctrl Pts',(-0.0855335548952896,-0.137363321270313,
0.161503325103128));
#33489=CARTESIAN_POINT('Ctrl Pts',(0.0692769376395434,-0.146237400156646,
0.169455829218231));
#33490=CARTESIAN_POINT('Ctrl Pts',(0.160471333140366,-0.0208236037998943,
0.177408333333334));
#33491=CARTESIAN_POINT('Ctrl Pts',(0.104307021434678,0.123712232533651,
0.185360837448436));
#33492=CARTESIAN_POINT('Ctrl Pts',(-0.0476410511166683,0.154644758993495,
0.193313341563539));
#33493=CARTESIAN_POINT('Ctrl Pts',(-0.155840975335119,0.043569044416721,
0.201265845678642));
#33494=CARTESIAN_POINT('Ctrl Pts',(-0.120934188958227,-0.107515548465566,
0.209218349793745));
#33495=CARTESIAN_POINT('Ctrl Pts',(0.0250248668081396,-0.159870032424242,
0.217170853908847));
#33496=CARTESIAN_POINT('Ctrl Pts',(0.148003917717295,-0.0654179758516589,
0.22512335802395));
#33497=CARTESIAN_POINT('Ctrl Pts',(0.135072924616463,0.0891065444250562,
0.233075862139053));
#33498=CARTESIAN_POINT('Ctrl Pts',(-0.0018937522113587,0.161805701157652,
0.241028366254156));
#33499=CARTESIAN_POINT('Ctrl Pts',(-0.137121421381912,0.0859208183297427,
0.248980870369259));
#33500=CARTESIAN_POINT('Ctrl Pts',(-0.146432299282947,-0.0688640178244077,
0.256933374484361));
#33501=CARTESIAN_POINT('Ctrl Pts',(-0.0212763296414524,-0.160411935407873,
0.264885878599465));
#33502=CARTESIAN_POINT('Ctrl Pts',(0.123417412665197,-0.104655690124044,
0.272838382714567));
#33503=CARTESIAN_POINT('Ctrl Pts',(0.154778574015767,0.0472044939582724,
0.28079088682967));
#33504=CARTESIAN_POINT('Ctrl Pts',(0.0440086139068953,0.155717414331996,
0.288743390944773));
#33505=CARTESIAN_POINT('Ctrl Pts',(-0.107173875445849,0.121237088576372,
0.296695895059875));
#33506=CARTESIAN_POINT('Ctrl Pts',(-0.159940009655938,-0.0245736553055878,
0.304648399174979));
#33507=CARTESIAN_POINT('Ctrl Pts',(-0.0658353441931666,-0.147818735886772,
0.312600903290081));
#33508=CARTESIAN_POINT('Ctrl Pts',(0.0887250488340134,-0.135323822498093,
0.320553407405184));
#33509=CARTESIAN_POINT('Ctrl Pts',(0.161810400657075,0.00143717084316612,
0.328505911520287));
#33510=CARTESIAN_POINT('Ctrl Pts',(0.0863073974718863,0.136878429149436,
0.33645841563539));
#33511=CARTESIAN_POINT('Ctrl Pts',(-0.0684505496358049,0.146626032784815,
0.344410919750492));
#33512=CARTESIAN_POINT('Ctrl Pts',(-0.160351260416479,0.0217288858867957,
0.352363423865596));
#33513=CARTESIAN_POINT('Ctrl Pts',(-0.105003525631241,-0.123121609963769,
0.360315927980698));
#33514=CARTESIAN_POINT('Ctrl Pts',(0.0467675611965104,-0.154911156838423,
0.368268432095801));
#33515=CARTESIAN_POINT('Ctrl Pts',(0.155592612973961,-0.0444478326960028,
0.376220936210903));
#33516=CARTESIAN_POINT('Ctrl Pts',(0.121539023828006,0.106831348553276,
0.384173440326007));
#33517=CARTESIAN_POINT('Ctrl Pts',(-0.0241222499571812,0.160008714396091,
0.392125944441109));
#33518=CARTESIAN_POINT('Ctrl Pts',(-0.147632373634519,0.0662521864660413,
0.400078448556213));
#33519=CARTESIAN_POINT('Ctrl Pts',(-0.135573649464267,-0.0883428432395635,
0.408030952671315));
#33520=CARTESIAN_POINT('Ctrl Pts',(0.00098059051083778,-0.161813818534397,
0.415983456786418));
#33521=CARTESIAN_POINT('Ctrl Pts',(0.136634323339825,-0.0866932765836425,
0.423935960901521));
#33522=CARTESIAN_POINT('Ctrl Pts',(0.146818643894656,0.068036512042807,
0.431888465016623));
#33523=CARTESIAN_POINT('Ctrl Pts',(0.0221811834420201,0.160289355015634,
0.439840969131727));
#33524=CARTESIAN_POINT('Ctrl Pts',(-0.122824664094011,0.105350436989503,
0.447793473246828));
#33525=CARTESIAN_POINT('Ctrl Pts',(-0.155042815727352,-0.0463300886426471,
0.455745977361933));
#33526=CARTESIAN_POINT('Ctrl Pts',(-0.0448861093263465,-0.155466890947849,
0.463698481477034));
#33527=CARTESIAN_POINT('Ctrl Pts',(0.106486852993449,-0.121839386582653,
0.471650985592139));
#33528=CARTESIAN_POINT('Ctrl Pts',(0.160078270104732,0.0236695030909907,
0.47960348970724));
#33529=CARTESIAN_POINT('Ctrl Pts',(0.0666644623728171,0.147447020596393,
0.487555993822343));
#33530=CARTESIAN_POINT('Ctrl Pts',(-0.087952257620471,0.135818244448492,
0.495508497937446));
#33531=CARTESIAN_POINT('Ctrl Pts',(-0.161830540810569,-0.000516108099224624,
0.503461002052549));
#33532=CARTESIAN_POINT('Ctrl Pts',(-0.0870507091382164,-0.136404149983702,
0.511413506167652));
#33533=CARTESIAN_POINT('Ctrl Pts',(0.0675690001343951,-0.146981398376774,
0.519366010282755));
#33534=CARTESIAN_POINT('Ctrl Pts',(0.16032830198575,-0.0226890204033332,
0.527318514397857));
#33535=CARTESIAN_POINT('Ctrl Pts',(0.105489414021532,0.122642716620584,
0.53527101851296));
#33536=CARTESIAN_POINT('Ctrl Pts',(0.00490214493024879,0.144133374197726,
0.540572687923028));
#33537=CARTESIAN_POINT('Ctrl Pts',(-0.0388047044046456,0.131206995015769,
0.543223522628063));
#33538=CARTESIAN_POINT('Ctrl Pts',(-0.0634007094575211,0.131904027763685,
0.));
#33539=CARTESIAN_POINT('Ctrl Pts',(-0.107339749959441,0.110784382003547,
0.00265083470503427));
#33540=CARTESIAN_POINT('Ctrl Pts',(-0.171684059780304,0.0215447005535634,
0.00795250411510281));
#33541=CARTESIAN_POINT('Ctrl Pts',(-0.110860953190881,-0.133069336628884,
0.0159050082302056));
#33542=CARTESIAN_POINT('Ctrl Pts',(0.0519117226680141,-0.165059354817326,
0.0238575123453085));
#33543=CARTESIAN_POINT('Ctrl Pts',(0.166938819754359,-0.045692445844369,
0.0318100164604112));
#33544=CARTESIAN_POINT('Ctrl Pts',(0.128707834787806,0.11574507779797,0.0397625205755141));
#33545=CARTESIAN_POINT('Ctrl Pts',(-0.0277346835769849,0.170836721147544,
0.0477150246906169));
#33546=CARTESIAN_POINT('Ctrl Pts',(-0.158697852682494,0.0690821280092034,
0.0556675288057197));
#33547=CARTESIAN_POINT('Ctrl Pts',(-0.143936642246025,-0.0961259112316717,
0.0636200329208225));
#33548=CARTESIAN_POINT('Ctrl Pts',(0.00300271935518024,-0.173054250792614,
0.0715725370359253));
#33549=CARTESIAN_POINT('Ctrl Pts',(0.14718312786408,-0.0910736516165751,
0.0795250411510281));
#33550=CARTESIAN_POINT('Ctrl Pts',(0.156208052339,0.0745410449363381,0.0874775452661308));
#33551=CARTESIAN_POINT('Ctrl Pts',(0.0217887425894723,0.171704439392484,
0.0954300493812338));
#33552=CARTESIAN_POINT('Ctrl Pts',(-0.132638649479586,0.11119456839884,
0.103382553496337));
#33553=CARTESIAN_POINT('Ctrl Pts',(-0.165265842816907,-0.0514241515016591,
0.111335057611439));
#33554=CARTESIAN_POINT('Ctrl Pts',(-0.0461315298523219,-0.166820570613858,
0.119287561726542));
#33555=CARTESIAN_POINT('Ctrl Pts',(0.115364724197092,-0.129027957109734,
0.127240065841645));
#33556=CARTESIAN_POINT('Ctrl Pts',(0.170923092625556,0.0272493764316328,
0.135192569956748));
#33557=CARTESIAN_POINT('Ctrl Pts',(0.0695250318900354,0.158503940884133,
0.143145074071851));
#33558=CARTESIAN_POINT('Ctrl Pts',(-0.0957169429781459,0.144206442545789,
0.151097578186953));
#33559=CARTESIAN_POINT('Ctrl Pts',(-0.173063315155402,-0.00251393578307793,
0.159050082302056));
#33560=CARTESIAN_POINT('Ctrl Pts',(-0.0914879280754666,-0.146925796220795,
0.167002586417159));
#33561=CARTESIAN_POINT('Ctrl Pts',(0.0740996150085664,-0.156417639414764,
0.174955090532262));
#33562=CARTESIAN_POINT('Ctrl Pts',(0.171642460113959,-0.0222732279635641,
0.182907594647365));
#33563=CARTESIAN_POINT('Ctrl Pts',(0.111568299557575,0.132324394162615,
0.190860098762467));
#33564=CARTESIAN_POINT('Ctrl Pts',(-0.0509575576899273,0.165410272089882,
0.19881260287757));
#33565=CARTESIAN_POINT('Ctrl Pts',(-0.166689762399376,0.0466020803974948,
0.206765106992673));
#33566=CARTESIAN_POINT('Ctrl Pts',(-0.129352958553163,-0.115000186500534,
0.214717611107776));
#33567=CARTESIAN_POINT('Ctrl Pts',(0.0267669596738252,-0.170999300166548,
0.222670115222879));
#33568=CARTESIAN_POINT('Ctrl Pts',(0.15830713216098,-0.0699720136370574,
0.230622619337982));
#33569=CARTESIAN_POINT('Ctrl Pts',(0.144475954815417,0.0953096493813769,
0.238575123453084));
#33570=CARTESIAN_POINT('Ctrl Pts',(-0.00202558476983171,0.173069719454941,
0.246527627568187));
#33571=CARTESIAN_POINT('Ctrl Pts',(-0.146667056599619,0.091902150649062,
0.25448013168329));
#33572=CARTESIAN_POINT('Ctrl Pts',(-0.156626106340649,-0.073657949998918,
0.262432635798393));
#33573=CARTESIAN_POINT('Ctrl Pts',(-0.0227574700751082,-0.171578927439738,
0.270385139913495));
#33574=CARTESIAN_POINT('Ctrl Pts',(0.132009050564966,-0.111941240633319,
0.278337644028599));
#33575=CARTESIAN_POINT('Ctrl Pts',(0.165553402574146,0.0504906098358712,
0.286290148143701));
#33576=CARTESIAN_POINT('Ctrl Pts',(0.0470722502852127,0.16655759976238,
0.294242652258804));
#33577=CARTESIAN_POINT('Ctrl Pts',(-0.11463472809428,0.129676944368004,
0.302195156373907));
#33578=CARTESIAN_POINT('Ctrl Pts',(-0.171074148826212,-0.0262843373211962,
0.31014766048901));
#33579=CARTESIAN_POINT('Ctrl Pts',(-0.0704184368548879,-0.158109058995279,
0.318100164604112));
#33580=CARTESIAN_POINT('Ctrl Pts',(0.0949015961765597,-0.144744318820362,
0.326052668719215));
#33581=CARTESIAN_POINT('Ctrl Pts',(0.173074746107531,0.00153721873120606,
0.334005172834318));
#33582=CARTESIAN_POINT('Ctrl Pts',(0.0923156412937011,0.146407148591411,
0.341957676949421));
#33583=CARTESIAN_POINT('Ctrl Pts',(-0.0732156984410742,0.156833326497772,
0.349910181064524));
#33584=CARTESIAN_POINT('Ctrl Pts',(-0.171514028590913,0.0232415307840867,
0.357862685179626));
#33585=CARTESIAN_POINT('Ctrl Pts',(-0.112313290525359,-0.131692655714946,
0.365815189294729));
#33586=CARTESIAN_POINT('Ctrl Pts',(0.0500232602310192,-0.165695215079871,
0.373767693409832));
#33587=CARTESIAN_POINT('Ctrl Pts',(0.16642411042382,-0.0475420450579947,
0.381720197524935));
#33588=CARTESIAN_POINT('Ctrl Pts',(0.129999898682469,0.114268356373264,
0.389672701640038));
#33589=CARTESIAN_POINT('Ctrl Pts',(-0.0258015076282358,0.171147636410509,
0.39762520575514));
#33590=CARTESIAN_POINT('Ctrl Pts',(-0.157909723233413,0.0708642973820958,
0.405577709870244));
#33591=CARTESIAN_POINT('Ctrl Pts',(-0.145011537358637,-0.0944927835418238,
0.413530213985346));
#33592=CARTESIAN_POINT('Ctrl Pts',(0.00104885380055552,-0.173078401918574,
0.421482718100449));
#33593=CARTESIAN_POINT('Ctrl Pts',(0.146146049484986,-0.0927283831757074,
0.429435222215551));
#33594=CARTESIAN_POINT('Ctrl Pts',(0.157039346128141,0.0727728378400491,
0.437387726330655));
#33595=CARTESIAN_POINT('Ctrl Pts',(0.0237253147943705,0.171447813678334,
0.445340230445757));
#33596=CARTESIAN_POINT('Ctrl Pts',(-0.131375038115538,0.112684351934323,
0.45329273456086));
#33597=CARTESIAN_POINT('Ctrl Pts',(-0.16583603933271,-0.0495553332567244,
0.461245238675963));
#33598=CARTESIAN_POINT('Ctrl Pts',(-0.0480108320841284,-0.166289636325362,
0.469197742791066));
#33599=CARTESIAN_POINT('Ctrl Pts',(0.113899878937264,-0.130321171031401,
0.477150246906169));
#33600=CARTESIAN_POINT('Ctrl Pts',(0.171222034203015,0.0253172430284407,
0.485102751021271));
#33601=CARTESIAN_POINT('Ctrl Pts',(0.071305273658044,0.157711466941583,
0.493055255136374));
#33602=CARTESIAN_POINT('Ctrl Pts',(-0.0940750075114624,0.145273159693308,
0.501007759251477));
#33603=CARTESIAN_POINT('Ctrl Pts',(-0.173096288307157,-0.000552036691550711,
0.50896026336658));
#33604=CARTESIAN_POINT('Ctrl Pts',(-0.0931106982085004,-0.14589985273243,
0.516912767481683));
#33605=CARTESIAN_POINT('Ctrl Pts',(0.0722727803374284,-0.157213430677441,
0.524865271596785));
#33606=CARTESIAN_POINT('Ctrl Pts',(0.171489471921174,-0.0242685045571198,
0.532817775711888));
#33607=CARTESIAN_POINT('Ctrl Pts',(0.112833003778924,0.131180424464991,
0.540770279826991));
#33608=CARTESIAN_POINT('Ctrl Pts',(0.00524340515652838,0.154167142801661,
0.54607194923706));
#33609=CARTESIAN_POINT('Ctrl Pts',(-0.0415060733756244,0.140340900570494,
0.548722783942094));
#33610=CARTESIAN_POINT('Ctrl Pts',(-0.146267142220666,-0.000128791573925899,
0.458934495415709));
#33611=CARTESIAN_POINT('Ctrl Pts',(-0.146386413462202,-0.014310462982192,
0.459704743169127));
#33612=CARTESIAN_POINT('Ctrl Pts',(-0.144492166435918,-0.0284609503391585,
0.460474990922545));
#33613=CARTESIAN_POINT('Ctrl Pts',(-0.140455004588417,-0.04197110290299,
0.461245238675963));
#33614=CARTESIAN_POINT('Ctrl Pts',(-0.126560970249849,-0.0884667676129373,
0.463896073380997));
#33615=CARTESIAN_POINT('Ctrl Pts',(-0.0872859011669886,-0.12737820196915,
0.466546908086032));
#33616=CARTESIAN_POINT('Ctrl Pts',(-0.0406632481219932,-0.140839174931596,
0.469197742791066));
#33617=CARTESIAN_POINT('Ctrl Pts',(0.00595940492300207,-0.154300147894042,
0.4718485774961));
#33618=CARTESIAN_POINT('Ctrl Pts',(0.0599296419301325,-0.142310659462721,
0.474499412201135));
#33619=CARTESIAN_POINT('Ctrl Pts',(0.0964684529779897,-0.110376179570421,
0.477150246906169));
#33620=CARTESIAN_POINT('Ctrl Pts',(0.133007264025847,-0.0784416996781205,
0.479801081611203));
#33621=CARTESIAN_POINT('Ctrl Pts',(0.152114649114431,-0.0265622283248395,
0.482451916316237));
#33622=CARTESIAN_POINT('Ctrl Pts',(0.145015548234561,0.0214432113373248,
0.485102751021272));
#33623=CARTESIAN_POINT('Ctrl Pts',(0.137916447354691,0.0694486509994885,
0.487753585726306));
#33624=CARTESIAN_POINT('Ctrl Pts',(0.104610860506367,0.113580058970536,
0.49040442043134));
#33625=CARTESIAN_POINT('Ctrl Pts',(0.0603946868872881,0.133572711748014,
0.493055255136374));
#33626=CARTESIAN_POINT('Ctrl Pts',(0.0161785132682088,0.153565364525491,
0.495706089841409));
#33627=CARTESIAN_POINT('Ctrl Pts',(-0.0389482471216264,0.1494192621094,
0.498356924546443));
#33628=CARTESIAN_POINT('Ctrl Pts',(-0.0796818407824932,0.123042011503878,
0.501007759251477));
#33629=CARTESIAN_POINT('Ctrl Pts',(-0.0932156861533014,0.114278099486334,
0.501888506167652));
#33630=CARTESIAN_POINT('Ctrl Pts',(-0.105160643384876,0.103060050144818,
0.502769253083826));
#33631=CARTESIAN_POINT('Ctrl Pts',(-0.115072616245005,0.0902061753896192,
0.50365));
#33632=CARTESIAN_POINT('Ctrl Pts',(-0.0686153921261811,-0.0959615133978097,
-2.38524477946811E-18));
#33633=CARTESIAN_POINT('Ctrl Pts',(-0.0712073975642253,-0.0945517549303093,
-2.83889532725695E-18));
#33634=CARTESIAN_POINT('Ctrl Pts',(-0.0737377474651001,-0.0930410231931718,
5.14426139154652E-18));
#33635=CARTESIAN_POINT('Ctrl Pts',(-0.0761998018605363,-0.091430646244207,
6.50521303491303E-18));
#33636=CARTESIAN_POINT('Ctrl Pts',(-0.0821844297375259,-0.0875162295688071,
8.61254391956714E-18));
#33637=CARTESIAN_POINT('Ctrl Pts',(-0.0877662752922461,-0.0830147043174395,
8.93950144287772E-18));
#33638=CARTESIAN_POINT('Ctrl Pts',(-0.0929202787198591,-0.0780195924546499,
9.54097911787244E-18));
#33639=CARTESIAN_POINT('Ctrl Pts',(-0.0954786058604465,-0.0755401353824292,
9.83953861283751E-18));
#33640=CARTESIAN_POINT('Ctrl Pts',(-0.0979275180792717,-0.0729421130511386,
1.49939491249404E-17));
#33641=CARTESIAN_POINT('Ctrl Pts',(-0.100258897735172,-0.0702429236064683,
1.47451495458029E-17));
#33642=CARTESIAN_POINT('Ctrl Pts',(-0.104668940139426,-0.0651371314726185,
1.42745197659725E-17));
#33643=CARTESIAN_POINT('Ctrl Pts',(-0.108665118623842,-0.0596642636850333,
-1.289688799178E-17));
#33644=CARTESIAN_POINT('Ctrl Pts',(-0.112224391688578,-0.0538945629536488,
-2.42861286636753E-17));
#33645=CARTESIAN_POINT('Ctrl Pts',(-0.114007263482302,-0.0510044681210456,
-2.99911014422584E-17));
#33646=CARTESIAN_POINT('Ctrl Pts',(-0.115680198610802,-0.0480392113919056,
-9.85233076388881E-18));
#33647=CARTESIAN_POINT('Ctrl Pts',(-0.117233217251657,-0.0450208645520303,
-8.67361737988404E-18));
#33648=CARTESIAN_POINT('Ctrl Pts',(-0.121574823694362,-0.0365827983617143,
-5.37841570781424E-18));
#33649=CARTESIAN_POINT('Ctrl Pts',(-0.124997594823754,-0.027708690332575,
-9.37762199309504E-19));
#33650=CARTESIAN_POINT('Ctrl Pts',(-0.127437485841812,-0.018577962661637,
9.54097911787244E-18));
#33651=CARTESIAN_POINT('Ctrl Pts',(-0.12867484687016,-0.0139474252741679,
1.48551452162951E-17));
#33652=CARTESIAN_POINT('Ctrl Pts',(-0.129658851279119,-0.00925026145395888,
3.85592351303264E-18));
#33653=CARTESIAN_POINT('Ctrl Pts',(-0.13037677319566,-0.00450727571206391,
1.12757025938492E-17));
#33654=CARTESIAN_POINT('Ctrl Pts',(-0.130820878643177,-0.00157327166937493,
1.5865567080829E-17));
#33655=CARTESIAN_POINT('Ctrl Pts',(-0.131161668086746,0.00136911314303839,
-1.28026844144678E-17));
#33656=CARTESIAN_POINT('Ctrl Pts',(-0.131397381290232,0.00431340779322604,
-1.38777878078145E-17));
#33657=CARTESIAN_POINT('Ctrl Pts',(-0.131719489313798,0.0083368605168951,
-1.53469436465178E-17));
#33658=CARTESIAN_POINT('Ctrl Pts',(-0.131845540542961,0.0123645321806217,
2.00482317967995E-17));
#33659=CARTESIAN_POINT('Ctrl Pts',(-0.131770346471732,0.0163834363085182,
1.56125112837913E-17));
#33660=CARTESIAN_POINT('Ctrl Pts',(-0.131648667841181,0.0228868047604438,
8.25177748690449E-18));
#33661=CARTESIAN_POINT('Ctrl Pts',(-0.131000732502959,0.0293672129596454,
8.03096099599679E-18));
#33662=CARTESIAN_POINT('Ctrl Pts',(-0.129864039936534,0.0357832484813204,
1.04083408558608E-17));
#33663=CARTESIAN_POINT('Ctrl Pts',(-0.129251059617937,0.0392432020469336,
1.16903823743602E-17));
#33664=CARTESIAN_POINT('Ctrl Pts',(-0.128495732458156,0.0426844698916631,
9.6775998731851E-18));
#33665=CARTESIAN_POINT('Ctrl Pts',(-0.127602533865954,0.0461005734698996,
1.21430643318376E-17));
#33666=CARTESIAN_POINT('Ctrl Pts',(-0.126801717254801,0.0491633553806105,
1.43535300781251E-17));
#33667=CARTESIAN_POINT('Ctrl Pts',(-0.125892295195939,0.0521970927094408,
-2.04303423409802E-17));
#33668=CARTESIAN_POINT('Ctrl Pts',(-0.12487995022281,0.0551944839930744,
-1.90819582357449E-17));
#33669=CARTESIAN_POINT('Ctrl Pts',(-0.122213990144214,0.063087964688102,
-1.55310558352899E-17));
#33670=CARTESIAN_POINT('Ctrl Pts',(-0.118834573434494,0.0707355529753685,
-2.09602125306395E-19));
#33671=CARTESIAN_POINT('Ctrl Pts',(-0.114813287039476,0.0780547614149283,
-3.46944695195361E-18));
#33672=CARTESIAN_POINT('Ctrl Pts',(-0.112113271799503,0.0829691028445349,
-5.65820692756715E-18));
#33673=CARTESIAN_POINT('Ctrl Pts',(-0.109123295952561,0.0877354841888059,
1.59792597750096E-17));
#33674=CARTESIAN_POINT('Ctrl Pts',(-0.105858764968584,0.0923275350572008,
1.73472347597681E-17));
#33675=CARTESIAN_POINT('Ctrl Pts',(-0.104035851863276,0.0948917348608856,
1.81111115738308E-17));
#33676=CARTESIAN_POINT('Ctrl Pts',(-0.102127627911009,0.0974005222622627,
-1.86461934882118E-17));
#33677=CARTESIAN_POINT('Ctrl Pts',(-0.100145200306236,0.0998394990060757,
-1.56125112837913E-17));
#33678=CARTESIAN_POINT('Ctrl Pts',(-0.0936292563097381,0.10785605196023,
-5.64125013933619E-18));
#33679=CARTESIAN_POINT('Ctrl Pts',(-0.0862946795456802,0.115149852779714,
-9.28670353986392E-18));
#33680=CARTESIAN_POINT('Ctrl Pts',(-0.0782486257709069,0.121568627915854,
-1.38777878078145E-17));
#33681=CARTESIAN_POINT('Ctrl Pts',(-0.0735390572914751,0.125325707088318,
-1.65650710848099E-17));
#33682=CARTESIAN_POINT('Ctrl Pts',(-0.0685847970970084,0.128782722422648,
6.71820819248872E-19));
#33683=CARTESIAN_POINT('Ctrl Pts',(-0.0634007094575211,0.131904027763685,
0.));
#33684=CARTESIAN_POINT('Origin',(0.,0.,0.));
#33685=CARTESIAN_POINT('Origin',(-0.0577350269189626,-0.1,-0.3));
#33686=CARTESIAN_POINT('',(-0.0577350269189626,-0.1,-0.3));
#33687=CARTESIAN_POINT('',(0.0577350269189626,-0.1,-0.3));
#33688=CARTESIAN_POINT('',(-0.0288675134594813,-0.1,-0.3));
#33689=CARTESIAN_POINT('',(-0.0577350269189626,-0.1,-0.1));
#33690=CARTESIAN_POINT('',(-0.0577350269189626,-0.1,-0.3));
#33691=CARTESIAN_POINT('',(0.0577350269189626,-0.1,-0.1));
#33692=CARTESIAN_POINT('',(-0.0577350269189626,-0.1,-0.1));
#33693=CARTESIAN_POINT('',(0.0577350269189626,-0.1,-0.3));
#33694=CARTESIAN_POINT('Origin',(-0.115470053837925,1.41410031829988E-17,
-0.3));
#33695=CARTESIAN_POINT('',(-0.115470053837925,1.41410031829988E-17,-0.3));
#33696=CARTESIAN_POINT('',(-0.101036297108185,-0.025,-0.3));
#33697=CARTESIAN_POINT('',(-0.115470053837925,1.38777878078145E-17,-0.1));
#33698=CARTESIAN_POINT('',(-0.115470053837925,1.41410031829988E-17,-0.3));
#33699=CARTESIAN_POINT('',(-0.115470053837925,1.41410031829988E-17,-0.1));
#33700=CARTESIAN_POINT('Origin',(-0.0577350269189626,0.1,-0.3));
#33701=CARTESIAN_POINT('',(-0.0577350269189626,0.1,-0.3));
#33702=CARTESIAN_POINT('',(-0.0721687836487032,0.075,-0.3));
#33703=CARTESIAN_POINT('',(-0.0577350269189626,0.1,-0.1));
#33704=CARTESIAN_POINT('',(-0.0577350269189626,0.1,-0.3));
#33705=CARTESIAN_POINT('',(-0.0577350269189626,0.1,-0.1));
#33706=CARTESIAN_POINT('Origin',(0.0577350269189626,0.1,-0.3));
#33707=CARTESIAN_POINT('',(0.0577350269189626,0.1,-0.3));
#33708=CARTESIAN_POINT('',(0.0288675134594813,0.1,-0.3));
#33709=CARTESIAN_POINT('',(0.0577350269189626,0.1,-0.1));
#33710=CARTESIAN_POINT('',(0.0577350269189626,0.1,-0.3));
#33711=CARTESIAN_POINT('',(0.0577350269189626,0.1,-0.1));
#33712=CARTESIAN_POINT('Origin',(0.115470053837925,0.,-0.3));
#33713=CARTESIAN_POINT('',(0.115470053837925,0.,-0.3));
#33714=CARTESIAN_POINT('',(0.101036297108185,0.025,-0.3));
#33715=CARTESIAN_POINT('',(0.115470053837925,0.,-0.1));
#33716=CARTESIAN_POINT('',(0.115470053837925,0.,-0.3));
#33717=CARTESIAN_POINT('',(0.115470053837925,0.,-0.1));
#33718=CARTESIAN_POINT('Origin',(0.0577350269189626,-0.1,-0.3));
#33719=CARTESIAN_POINT('',(0.0721687836487032,-0.075,-0.3));
#33720=CARTESIAN_POINT('',(0.0577350269189626,-0.1,-0.1));
#33721=CARTESIAN_POINT('Origin',(0.,0.,-0.1));
#33722=CARTESIAN_POINT('Origin',(0.,0.,0.));
#33723=CARTESIAN_POINT('',(-0.3,-3.67394039744206E-17,0.));
#33724=CARTESIAN_POINT('Origin',(0.,0.,0.));
#33725=CARTESIAN_POINT('Origin',(0.,0.,-0.3));
#33726=CARTESIAN_POINT('',(-0.3,-3.67394039744206E-17,-0.3));
#33727=CARTESIAN_POINT('',(-0.3,-3.67394039744206E-17,-0.3));
#33728=CARTESIAN_POINT('Origin',(0.,0.,-0.3));
#33729=CARTESIAN_POINT('Origin',(0.,0.,-0.3));
#33730=CARTESIAN_POINT('Origin',(0.,0.,0.6));
#33731=CARTESIAN_POINT('',(0.,0.,0.));
#33732=CARTESIAN_POINT('Origin',(0.,0.,0.));
#33733=CARTESIAN_POINT('',(-0.146500586129689,0.000104807665585484,0.0160655045842905));
#33734=CARTESIAN_POINT('',(-0.146471000393815,0.000161627070721384,0.00893449541570859));
#33735=CARTESIAN_POINT('',(-0.14635,-1.79227059055215E-17,0.));
#33736=CARTESIAN_POINT('',(0.0634007094575212,0.131904027763685,0.));
#33737=CARTESIAN_POINT('Ctrl Pts',(-0.146500586129689,0.000104807665585484,
0.0160655045842905));
#33738=CARTESIAN_POINT('Ctrl Pts',(-0.14654494062996,0.00598698351314685,
0.0157446908947048));
#33739=CARTESIAN_POINT('Ctrl Pts',(-0.146221105349753,0.0118639507829193,
0.0154238772051191));
#33740=CARTESIAN_POINT('Ctrl Pts',(-0.145512600887712,0.0176938044004412,
0.0151030635155334));
#33741=CARTESIAN_POINT('Ctrl Pts',(-0.139696831446137,0.0655482447521769,
0.0124696595607311));
#33742=CARTESIAN_POINT('Ctrl Pts',(-0.107962161373412,0.110228180545907,
0.00983625560592885));
#33743=CARTESIAN_POINT('Ctrl Pts',(-0.06469522132477,0.13152107817143,0.0072028516511266));
#33744=CARTESIAN_POINT('Ctrl Pts',(-0.0252475006917791,0.150934428781716,
0.00480190110075107));
#33745=CARTESIAN_POINT('Ctrl Pts',(0.0237864150713563,0.150907312609249,
0.00240095055037554));
#33746=CARTESIAN_POINT('Ctrl Pts',(0.0635538308725811,0.132076982143462,
1.66967134562768E-17));
#33747=CARTESIAN_POINT('',(-0.063400709457524,0.131904027763684,0.));
#33748=CARTESIAN_POINT('Origin',(0.,0.,0.));
#33749=CARTESIAN_POINT('Ctrl Pts',(-0.0634007094575239,0.131904027763684,
1.49186218934005E-16));
#33750=CARTESIAN_POINT('Ctrl Pts',(-0.107082934395073,0.110907822426531,
0.00263534106650592));
#33751=CARTESIAN_POINT('Ctrl Pts',(-0.139152358317953,0.0667027373135744,
0.00527068213301169));
#33752=CARTESIAN_POINT('Ctrl Pts',(-0.145347393378452,0.0189333151714045,
0.00790602319951745));
#33753=CARTESIAN_POINT('Ctrl Pts',(-0.146153287982764,0.0127191260377668,
0.00824884727158116));
#33754=CARTESIAN_POINT('Ctrl Pts',(-0.14652131876894,0.00644461879462582,
0.00859167134364488));
#33755=CARTESIAN_POINT('Ctrl Pts',(-0.146471000393815,0.000161627070721384,
0.00893449541570859));
#33756=CARTESIAN_POINT('Origin',(0.,0.,0.));
#33757=CARTESIAN_POINT('',(-0.146124286466753,3.81045546672121E-5,0.0660655045842905));
#33758=CARTESIAN_POINT('',(-0.146121893894205,3.63833482308178E-5,0.0589344954157087));
#33759=CARTESIAN_POINT('',(-0.14635,-1.79227059055215E-17,0.));
#33760=CARTESIAN_POINT('Ctrl Pts',(-0.146124286466753,3.81045546672121E-5,
0.0660655045842905));
#33761=CARTESIAN_POINT('Ctrl Pts',(-0.146175624225919,0.0219480700681356,
0.0648784479568517));
#33762=CARTESIAN_POINT('Ctrl Pts',(-0.141554683648142,0.0438374299905643,
0.0636913913294129));
#33763=CARTESIAN_POINT('Ctrl Pts',(-0.132150173022132,0.0634306246655632,
0.062504334701974));
#33764=CARTESIAN_POINT('Ctrl Pts',(-0.111286909296501,0.106896787232447,
0.0598709307471717));
#33765=CARTESIAN_POINT('Ctrl Pts',(-0.0668815981213141,0.139062512957816,
0.0572375267923695));
#33766=CARTESIAN_POINT('Ctrl Pts',(-0.0190775358903001,0.145337701034954,
0.0546041228375673));
#33767=CARTESIAN_POINT('Ctrl Pts',(0.028726526340714,0.151612889112092,
0.051970718882765));
#33768=CARTESIAN_POINT('Ctrl Pts',(0.0799293396275551,0.131997539540999,
0.0493373149279628));
#33769=CARTESIAN_POINT('Ctrl Pts',(0.111303508306999,0.0953874982726326,
0.0467039109731605));
#33770=CARTESIAN_POINT('Ctrl Pts',(0.142677676986443,0.0587774570042668,
0.0440705070183582));
#33771=CARTESIAN_POINT('Ctrl Pts',(0.154223201058489,0.00517272403862895,
0.041437103063556));
#33772=CARTESIAN_POINT('Ctrl Pts',(0.14070340769012,-0.0411058697401277,
0.0388036991087537));
#33773=CARTESIAN_POINT('Ctrl Pts',(0.12718361432175,-0.0873844635188848,
0.0361702951539514));
#33774=CARTESIAN_POINT('Ctrl Pts',(0.0885985035129631,-0.12633691811076,
0.0335368911991492));
#33775=CARTESIAN_POINT('Ctrl Pts',(0.0424500313328507,-0.140301337584722,
0.030903487244347));
#33776=CARTESIAN_POINT('Ctrl Pts',(-0.00369844084726173,-0.154265757058684,
0.0282700832895447));
#33777=CARTESIAN_POINT('Ctrl Pts',(-0.0574102743986997,-0.143242141414731,
0.0256366793347424));
#33778=CARTESIAN_POINT('Ctrl Pts',(-0.0943177567692062,-0.112215861137884,
0.0230032753799401));
#33779=CARTESIAN_POINT('Ctrl Pts',(-0.126728995572139,-0.0849693486522956,
0.0206906851147236));
#33780=CARTESIAN_POINT('Ctrl Pts',(-0.146180856053097,-0.0422969446440751,
0.0183780948495071));
#33781=CARTESIAN_POINT('Ctrl Pts',(-0.146500586129689,0.000104807665585484,
0.0160655045842905));
#33782=CARTESIAN_POINT('Ctrl Pts',(-0.146471000393815,0.000161627070721384,
0.00893449541570859));
#33783=CARTESIAN_POINT('Ctrl Pts',(-0.146134513724681,-0.0418536993801969,
0.0112270124101507));
#33784=CARTESIAN_POINT('Ctrl Pts',(-0.127090283331881,-0.0842484349621326,
0.0135195294045928));
#33785=CARTESIAN_POINT('Ctrl Pts',(-0.0951738980203006,-0.111522448354846,
0.0158120463990349));
#33786=CARTESIAN_POINT('Ctrl Pts',(-0.0584847214035319,-0.142875030567541,
0.0184473874655407));
#33787=CARTESIAN_POINT('Ctrl Pts',(-0.00478572197187679,-0.154246435821546,
0.0210827285320465));
#33788=CARTESIAN_POINT('Ctrl Pts',(0.0414949714453012,-0.140576153089947,
0.0237180695985523));
#33789=CARTESIAN_POINT('Ctrl Pts',(0.0877756648624791,-0.126905870358348,
0.0263534106650582));
#33790=CARTESIAN_POINT('Ctrl Pts',(0.12663805226518,-0.0881938996411451,
0.028988751731564));
#33791=CARTESIAN_POINT('Ctrl Pts',(0.140447863117085,-0.0419714582064656,
0.0316240927980698));
#33792=CARTESIAN_POINT('Ctrl Pts',(0.154257673968991,0.00425098322821388,
0.0342594338645756));
#33793=CARTESIAN_POINT('Ctrl Pts',(0.143014908270101,0.0579838953803693,
0.0368947749310814));
#33794=CARTESIAN_POINT('Ctrl Pts',(0.111816739036639,0.0947918176848183,
0.0395301159975872));
#33795=CARTESIAN_POINT('Ctrl Pts',(0.0806185698031766,0.131599739989267,
0.042165457064093));
#33796=CARTESIAN_POINT('Ctrl Pts',(0.0294649970351413,0.15148267244601,
0.0448007981305989));
#33797=CARTESIAN_POINT('Ctrl Pts',(-0.0184028717348104,0.145423626667293,
0.0474361391971047));
#33798=CARTESIAN_POINT('Ctrl Pts',(-0.0662707405047621,0.139364580888577,
0.0500714802636105));
#33799=CARTESIAN_POINT('Ctrl Pts',(-0.11085290527663,0.107363556874401,
0.0527068213301163));
#33800=CARTESIAN_POINT('Ctrl Pts',(-0.131901071754926,0.0639489919997987,
0.0553421623966221));
#33801=CARTESIAN_POINT('Ctrl Pts',(-0.141464922191872,0.0442223138744639,
0.0565396067363176));
#33802=CARTESIAN_POINT('Ctrl Pts',(-0.146169931163403,0.0221391901971212,
0.0577370510760131));
#33803=CARTESIAN_POINT('Ctrl Pts',(-0.146121893894205,3.63833482308178E-5,
0.0589344954157087));
#33804=CARTESIAN_POINT('Origin',(0.,0.,0.));
#33805=CARTESIAN_POINT('',(-0.146368002745976,-0.000129372869328834,0.116065504584291));
#33806=CARTESIAN_POINT('',(-0.146366557616609,-0.000129983413451606,0.108934495415709));
#33807=CARTESIAN_POINT('',(-0.14635,-1.79227059055215E-17,0.));
#33808=CARTESIAN_POINT('Ctrl Pts',(-0.146368002745976,-0.000129372869328834,
0.116065504584291));
#33809=CARTESIAN_POINT('Ctrl Pts',(-0.146025111950034,0.0376095209348488,
0.114012205018999));
#33810=CARTESIAN_POINT('Ctrl Pts',(-0.131097704503774,0.0755892522017571,
0.111958905453707));
#33811=CARTESIAN_POINT('Ctrl Pts',(-0.104818007194008,0.1024708903805,0.109905605888415));
#33812=CARTESIAN_POINT('Ctrl Pts',(-0.0711136904949951,0.136947210099294,
0.107272201933612));
#33813=CARTESIAN_POINT('Ctrl Pts',(-0.0187363862257596,0.153168661700715,
0.10463879797881));
#33814=CARTESIAN_POINT('Ctrl Pts',(0.0285541005041433,0.143776766284718,
0.102005394024008));
#33815=CARTESIAN_POINT('Ctrl Pts',(0.0758445872340461,0.134384870868722,
0.0993719900692057));
#33816=CARTESIAN_POINT('Ctrl Pts',(0.118048256424616,0.0993796284353078,
0.0967385861144034));
#33817=CARTESIAN_POINT('Ctrl Pts',(0.136020336225278,0.0546403479960236,
0.0941051821596012));
#33818=CARTESIAN_POINT('Ctrl Pts',(0.153992416025939,0.00990106755673973,
0.0914717782047989));
#33819=CARTESIAN_POINT('Ctrl Pts',(0.147732906436694,-0.0445722508884142,
0.0888383742499967));
#33820=CARTESIAN_POINT('Ctrl Pts',(0.120081310876684,-0.0840688974447852,
0.0862049702951944));
#33821=CARTESIAN_POINT('Ctrl Pts',(0.092429715316675,-0.123565544001157,
0.0835715663403921));
#33822=CARTESIAN_POINT('Ctrl Pts',(0.0433860337859016,-0.148085518668745,
0.0809381623855898));
#33823=CARTESIAN_POINT('Ctrl Pts',(-0.00480217723865872,-0.146506046566169,
0.0783047584307875));
#33824=CARTESIAN_POINT('Ctrl Pts',(-0.0529903882632186,-0.144926574463593,
0.0756713544759853));
#33825=CARTESIAN_POINT('Ctrl Pts',(-0.100323128781565,-0.117247655590855,
0.0730379505211831));
#33826=CARTESIAN_POINT('Ctrl Pts',(-0.125328890902702,-0.0760248964502869,
0.0704045465663809));
#33827=CARTESIAN_POINT('Ctrl Pts',(-0.139062832915904,-0.053384075469981,
0.0689581992390174));
#33828=CARTESIAN_POINT('Ctrl Pts',(-0.146061734917782,-0.0266576901787336,
0.067511851911654));
#33829=CARTESIAN_POINT('Ctrl Pts',(-0.146124286466753,3.81045546672121E-5,
0.0660655045842905));
#33830=CARTESIAN_POINT('Ctrl Pts',(-0.146121893894205,3.63833482308178E-5,
0.0589344954157087));
#33831=CARTESIAN_POINT('Ctrl Pts',(-0.146064210518155,-0.026504769812526,
0.060372392142519));
#33832=CARTESIAN_POINT('Ctrl Pts',(-0.139152958627323,-0.0530743047642348,
0.0618102888693293));
#33833=CARTESIAN_POINT('Ctrl Pts',(-0.125571320368441,-0.0756261679111494,
0.0632481855961396));
#33834=CARTESIAN_POINT('Ctrl Pts',(-0.100679234318938,-0.116958657212465,
0.0658835266626455));
#33835=CARTESIAN_POINT('Ctrl Pts',(-0.0533808940352117,-0.144795530080065,
0.0685188677291512));
#33836=CARTESIAN_POINT('Ctrl Pts',(-0.00516183231960515,-0.146494306755382,
0.071154208795657));
#33837=CARTESIAN_POINT('Ctrl Pts',(0.0430572293960016,-0.148193083430699,
0.0737895498621628));
#33838=CARTESIAN_POINT('Ctrl Pts',(0.0921970125434883,-0.123753763913733,
0.0764248909286687));
#33839=CARTESIAN_POINT('Ctrl Pts',(0.119936668638416,-0.0842765346784538,
0.0790602319951745));
#33840=CARTESIAN_POINT('Ctrl Pts',(0.147676324733344,-0.0447993054431753,
0.0816955730616803));
#33841=CARTESIAN_POINT('Ctrl Pts',(0.154015853775713,0.00971583351041531,
0.0843309141281861));
#33842=CARTESIAN_POINT('Ctrl Pts',(0.136075382627054,0.0545053485317346,
0.0869662551946919));
#33843=CARTESIAN_POINT('Ctrl Pts',(0.118134911478395,0.0992948635530542,
0.0896015962611977));
#33844=CARTESIAN_POINT('Ctrl Pts',(0.0759144401387073,0.134358754642102,
0.0922369373277035));
#33845=CARTESIAN_POINT('Ctrl Pts',(0.0285922932904845,0.143769920707126,
0.0948722783942094));
#33846=CARTESIAN_POINT('Ctrl Pts',(-0.0187298535577381,0.15318108677215,
0.0975076194607152));
#33847=CARTESIAN_POINT('Ctrl Pts',(-0.0711536759144954,0.13693952781315,
0.100142960527221));
#33848=CARTESIAN_POINT('Ctrl Pts',(-0.104866248150923,0.102422641268563,
0.102778301593727));
#33849=CARTESIAN_POINT('Ctrl Pts',(-0.131117262559492,0.0755453303453163,
0.104830366201054));
#33850=CARTESIAN_POINT('Ctrl Pts',(-0.146023101823344,0.0375871567885092,
0.106882430808381));
#33851=CARTESIAN_POINT('Ctrl Pts',(-0.146366557616609,-0.000129983413451606,
0.108934495415709));
#33852=CARTESIAN_POINT('Origin',(0.,0.,0.));
#33853=CARTESIAN_POINT('',(-0.14651736545536,8.65668654492988E-5,0.166065504584291));
#33854=CARTESIAN_POINT('',(-0.146524127737672,8.31850724179233E-5,0.158934495415709));
#33855=CARTESIAN_POINT('',(-0.14635,-1.79227059055215E-17,0.));
#33856=CARTESIAN_POINT('Ctrl Pts',(-0.14651736545536,8.65668654492988E-5,
0.166065504584291));
#33857=CARTESIAN_POINT('Ctrl Pts',(-0.146554285531508,0.00533178393548585,
0.165779366035948));
#33858=CARTESIAN_POINT('Ctrl Pts',(-0.146296777197391,0.0105733383781062,
0.165493227487605));
#33859=CARTESIAN_POINT('Ctrl Pts',(-0.145732753046151,0.0157816995937671,
0.165207088939262));
#33860=CARTESIAN_POINT('Ctrl Pts',(-0.140541899038255,0.0637155382981208,
0.16257368498446));
#33861=CARTESIAN_POINT('Ctrl Pts',(-0.109389226009343,0.108837918334108,
0.159940281029658));
#33862=CARTESIAN_POINT('Ctrl Pts',(-0.0664064572564633,0.130680066597967,
0.157306877074855));
#33863=CARTESIAN_POINT('Ctrl Pts',(-0.0234236885035836,0.152522214861825,
0.154673473120053));
#33864=CARTESIAN_POINT('Ctrl Pts',(0.031389175973264,0.151084131353554,
0.152040069165251));
#33865=CARTESIAN_POINT('Ctrl Pts',(0.073167488832194,0.12701817148098,0.149406665210449));
#33866=CARTESIAN_POINT('Ctrl Pts',(0.114945801691124,0.102952211608407,
0.146773261255646));
#33867=CARTESIAN_POINT('Ctrl Pts',(0.143689562932137,0.0562583753715299,
0.144139857300844));
#33868=CARTESIAN_POINT('Ctrl Pts',(0.146359798857064,0.00811829104130666,
0.141506453346042));
#33869=CARTESIAN_POINT('Ctrl Pts',(0.149030034781992,-0.0400217932889162,
0.13887304939124));
#33870=CARTESIAN_POINT('Ctrl Pts',(0.125626745390835,-0.0896081257124856,
0.136239645436437));
#33871=CARTESIAN_POINT('Ctrl Pts',(0.0867663172267087,-0.118146957909964,
0.133606241481635));
#33872=CARTESIAN_POINT('Ctrl Pts',(0.0479058890625822,-0.146685790107443,
0.130972837526833));
#33873=CARTESIAN_POINT('Ctrl Pts',(-0.00641167787451363,-0.154177122078832,
0.128339433572031));
#33874=CARTESIAN_POINT('Ctrl Pts',(-0.0515464175662268,-0.13722267989126,
0.125706029617228));
#33875=CARTESIAN_POINT('Ctrl Pts',(-0.0966811572579399,-0.120268237703689,
0.123072625662426));
#33876=CARTESIAN_POINT('Ctrl Pts',(-0.13263306970427,-0.0788680213571585,
0.120439221707624));
#33877=CARTESIAN_POINT('Ctrl Pts',(-0.143093361363041,-0.0318023192658095,
0.117805817752821));
#33878=CARTESIAN_POINT('Ctrl Pts',(-0.145397626569199,-0.0214343617297895,
0.117225713363311));
#33879=CARTESIAN_POINT('Ctrl Pts',(-0.146464877288401,-0.0107914790330514,
0.116645608973801));
#33880=CARTESIAN_POINT('Ctrl Pts',(-0.146368002745976,-0.000129372869328834,
0.116065504584291));
#33881=CARTESIAN_POINT('Ctrl Pts',(-0.146366557616609,-0.000129983413451606,
0.108934495415709));
#33882=CARTESIAN_POINT('Ctrl Pts',(-0.146464181092139,-0.0108506595114597,
0.109517771874887));
#33883=CARTESIAN_POINT('Ctrl Pts',(-0.145385284604313,-0.0215518621108894,
0.110101048334066));
#33884=CARTESIAN_POINT('Ctrl Pts',(-0.143055987718722,-0.0319735935649507,
0.110684324793244));
#33885=CARTESIAN_POINT('Ctrl Pts',(-0.132531832933994,-0.0790607277237021,
0.11331966585975));
#33886=CARTESIAN_POINT('Ctrl Pts',(-0.0964822012484396,-0.12044278191103,
0.115955006926256));
#33887=CARTESIAN_POINT('Ctrl Pts',(-0.0512822836387571,-0.13732242834474,
0.118590347992762));
#33888=CARTESIAN_POINT('Ctrl Pts',(-0.00608236602907434,-0.154202074778449,
0.121225689059267));
#33889=CARTESIAN_POINT('Ctrl Pts',(0.0482678375047366,-0.14657931345854,
0.123861030125773));
#33890=CARTESIAN_POINT('Ctrl Pts',(0.0870803134198012,-0.117916681520738,
0.126496371192279));
#33891=CARTESIAN_POINT('Ctrl Pts',(0.125892789334866,-0.089254049582936,
0.129131712258785));
#33892=CARTESIAN_POINT('Ctrl Pts',(0.149167537631184,-0.0395515470272406,
0.131767053325291));
#33893=CARTESIAN_POINT('Ctrl Pts',(0.146332238452734,0.00861396207485353,
0.134402394391797));
#33894=CARTESIAN_POINT('Ctrl Pts',(0.143496939274284,0.0567794711769477,
0.137037735458302));
#33895=CARTESIAN_POINT('Ctrl Pts',(0.114551592621066,0.103407986825441,
0.139673076524808));
#33896=CARTESIAN_POINT('Ctrl Pts',(0.0726443273415577,0.127318991170589,
0.142308417591314));
#33897=CARTESIAN_POINT('Ctrl Pts',(0.0307370620620493,0.151229995515737,
0.14494375865782));
#33898=CARTESIAN_POINT('Ctrl Pts',(-0.0241321218437492,0.152423488557541,
0.147579099724326));
#33899=CARTESIAN_POINT('Ctrl Pts',(-0.067039462170215,0.130357334843671,
0.150214440790831));
#33900=CARTESIAN_POINT('Ctrl Pts',(-0.109946802496681,0.108291181129802,
0.152849781857337));
#33901=CARTESIAN_POINT('Ctrl Pts',(-0.140892299243814,0.0629653806602592,
0.155485122923843));
#33902=CARTESIAN_POINT('Ctrl Pts',(-0.145819277598255,0.0149687147614827,
0.158120463990349));
#33903=CARTESIAN_POINT('Ctrl Pts',(-0.1463265762883,0.0100268124462353,
0.158391807798802));
#33904=CARTESIAN_POINT('Ctrl Pts',(-0.146558040382541,0.0050565950257616,
0.158663151607255));
#33905=CARTESIAN_POINT('Ctrl Pts',(-0.146524127737672,8.31850724179233E-5,
0.158934495415709));
#33906=CARTESIAN_POINT('Origin',(0.,0.,0.));
#33907=CARTESIAN_POINT('',(-0.146129957599089,4.76874783713124E-5,0.21606550458429));
#33908=CARTESIAN_POINT('',(-0.146134590291164,5.53529746073057E-5,0.208934495415709));
#33909=CARTESIAN_POINT('',(-0.14635,-1.79227059055215E-17,0.));
#33910=CARTESIAN_POINT('Ctrl Pts',(-0.146129957599089,4.76874783713124E-5,
0.21606550458429));
#33911=CARTESIAN_POINT('Ctrl Pts',(-0.146192738333019,0.0213155226117273,
0.214913123098095));
#33912=CARTESIAN_POINT('Ctrl Pts',(-0.14184845306411,0.0425589323614883,
0.213760741611899));
#33913=CARTESIAN_POINT('Ctrl Pts',(-0.132968065125987,0.0616975770053832,
0.212608360125703));
#33914=CARTESIAN_POINT('Ctrl Pts',(-0.11267474299563,0.105432905191852,
0.2099749561709));
#33915=CARTESIAN_POINT('Ctrl Pts',(-0.0686935897650435,0.13817700942041,
0.207341552216098));
#33916=CARTESIAN_POINT('Ctrl Pts',(-0.0209756858809845,0.145076248759314,
0.204708148261296));
#33917=CARTESIAN_POINT('Ctrl Pts',(0.0267422180030747,0.151975488098219,
0.202074744306494));
#33918=CARTESIAN_POINT('Ctrl Pts',(0.0781968725406062,0.13302986254747,
0.199441340351692));
#33919=CARTESIAN_POINT('Ctrl Pts',(0.110047008199114,0.0968336374273772,
0.196807936396889));
#33920=CARTESIAN_POINT('Ctrl Pts',(0.141897143857622,0.0606374123072843,
0.194174532442087));
#33921=CARTESIAN_POINT('Ctrl Pts',(0.154142760637107,0.00719058761784734,
0.191541128487285));
#33922=CARTESIAN_POINT('Ctrl Pts',(0.141228904479148,-0.0392618630629832,
0.188907724532483));
#33923=CARTESIAN_POINT('Ctrl Pts',(0.128315048321188,-0.0857143137438141,
0.18627432057768));
#33924=CARTESIAN_POINT('Ctrl Pts',(0.0902417192257834,-0.125172390416039,
0.183640916622878));
#33925=CARTESIAN_POINT('Ctrl Pts',(0.0442800434850501,-0.139736806546778,
0.181007512668076));
#33926=CARTESIAN_POINT('Ctrl Pts',(-0.00168163225568323,-0.154301222677517,
0.178374108713273));
#33927=CARTESIAN_POINT('Ctrl Pts',(-0.0555316546417454,-0.143971978266771,
0.175740704758471));
#33928=CARTESIAN_POINT('Ctrl Pts',(-0.0928421483413364,-0.113434707375038,
0.173107300803669));
#33929=CARTESIAN_POINT('Ctrl Pts',(-0.126098584749153,-0.0862155337115625,
0.17076003539721));
#33930=CARTESIAN_POINT('Ctrl Pts',(-0.146214500923306,-0.0429412483281845,
0.16841276999075));
#33931=CARTESIAN_POINT('Ctrl Pts',(-0.14651736545536,8.65668654492988E-5,
0.166065504584291));
#33932=CARTESIAN_POINT('Ctrl Pts',(-0.146524127737672,8.31850724179233E-5,
0.158934495415709));
#33933=CARTESIAN_POINT('Ctrl Pts',(-0.146228674526712,-0.043246078859919,
0.161298492673761));
#33934=CARTESIAN_POINT('Ctrl Pts',(-0.125790555024919,-0.0868176629158599,
0.163662489931814));
#33935=CARTESIAN_POINT('Ctrl Pts',(-0.0921252733308782,-0.11401867430555,
0.166026487189866));
#33936=CARTESIAN_POINT('Ctrl Pts',(-0.0545958307473115,-0.144341866145796,
0.168661828256372));
#33937=CARTESIAN_POINT('Ctrl Pts',(-0.000628485618429035,-0.154320718498276,
0.171297169322878));
#33938=CARTESIAN_POINT('Ctrl Pts',(0.0452626498105411,-0.139422439628514,
0.173932510389384));
#33939=CARTESIAN_POINT('Ctrl Pts',(0.0911537852395115,-0.124524160758753,
0.17656785145589));
#33940=CARTESIAN_POINT('Ctrl Pts',(0.128968710968569,-0.0847487506667484,
0.179203192522395));
#33941=CARTESIAN_POINT('Ctrl Pts',(0.141530385150016,-0.0381637812674535,
0.181838533588901));
#33942=CARTESIAN_POINT('Ctrl Pts',(0.154092059331463,0.00842118813184087,
0.184473874655407));
#33943=CARTESIAN_POINT('Ctrl Pts',(0.141400481965299,0.0618157168384256,
0.187109215721913));
#33944=CARTESIAN_POINT('Ctrl Pts',(0.109220671810841,0.0977658885483793,
0.189744556788419));
#33945=CARTESIAN_POINT('Ctrl Pts',(0.0770408616563825,0.133716060258333,
0.192379897854925));
#33946=CARTESIAN_POINT('Ctrl Pts',(0.025372818713629,0.152221874971656,
0.19501523892143));
#33947=CARTESIAN_POINT('Ctrl Pts',(-0.022313779030084,0.144877256285936,
0.197650579987936));
#33948=CARTESIAN_POINT('Ctrl Pts',(-0.0700003767737975,0.137532637600217,
0.200285921054442));
#33949=CARTESIAN_POINT('Ctrl Pts',(-0.113705529318471,0.104337585515455,
0.202921262120948));
#33950=CARTESIAN_POINT('Ctrl Pts',(-0.133576619842631,0.0603706116554267,
0.205556603187454));
#33951=CARTESIAN_POINT('Ctrl Pts',(-0.142066653397378,0.041585478402751,
0.206682567263539));
#33952=CARTESIAN_POINT('Ctrl Pts',(-0.146205843323087,0.0208339599326467,
0.207808531339624));
#33953=CARTESIAN_POINT('Ctrl Pts',(-0.146134590291164,5.53529746073057E-5,
0.208934495415709));
#33954=CARTESIAN_POINT('Origin',(0.,0.,0.));
#33955=CARTESIAN_POINT('',(-0.146348968946192,-0.000130334789587572,0.266065504584291));
#33956=CARTESIAN_POINT('',(-0.146327394052832,-0.000130859996972892,0.258934495415708));
#33957=CARTESIAN_POINT('',(-0.14635,-1.79227059055215E-17,0.));
#33958=CARTESIAN_POINT('Ctrl Pts',(-0.146348968946192,-0.000130334789587572,
0.266065504584291));
#33959=CARTESIAN_POINT('Ctrl Pts',(-0.146013620606683,0.0369836123692833,
0.264046880160242));
#33960=CARTESIAN_POINT('Ctrl Pts',(-0.131636768783893,0.074328824870482,
0.262028255736193));
#33961=CARTESIAN_POINT('Ctrl Pts',(-0.106148536005423,0.10109196632601,
0.260009631312144));
#33962=CARTESIAN_POINT('Ctrl Pts',(-0.072897767709896,0.136005921449249,
0.257376227357342));
#33963=CARTESIAN_POINT('Ctrl Pts',(-0.020736980756812,0.152910669462462,
0.254742823402539));
#33964=CARTESIAN_POINT('Ctrl Pts',(0.0266722339182632,0.144137744153214,
0.252109419447737));
#33965=CARTESIAN_POINT('Ctrl Pts',(0.0740814485933381,0.135364818843967,
0.249476015492935));
#33966=CARTESIAN_POINT('Ctrl Pts',(0.116739090990404,0.100914220212258,
0.246842611538132));
#33967=CARTESIAN_POINT('Ctrl Pts',(0.135294462171964,0.056413702744499,
0.24420920758333));
#33968=CARTESIAN_POINT('Ctrl Pts',(0.153849833353525,0.0119131852767396,
0.241575803628528));
#33969=CARTESIAN_POINT('Ctrl Pts',(0.148302933319579,-0.0426372510270706,
0.238942399673726));
#33970=CARTESIAN_POINT('Ctrl Pts',(0.121169990969772,-0.082492003492008,
0.236308995718923));
#33971=CARTESIAN_POINT('Ctrl Pts',(0.094037048619966,-0.122346755956945,
0.233675591764121));
#33972=CARTESIAN_POINT('Ctrl Pts',(0.0453180639542996,-0.14750582458301,
0.231042187809319));
#33973=CARTESIAN_POINT('Ctrl Pts',(-0.00288666981273841,-0.146556352606171,
0.228408783854516));
#33974=CARTESIAN_POINT('Ctrl Pts',(-0.0510914035797761,-0.145606880629331,
0.225775379899714));
#33975=CARTESIAN_POINT('Ctrl Pts',(-0.0987818864481854,-0.118548868049589,
0.223141975944912));
#33976=CARTESIAN_POINT('Ctrl Pts',(-0.124324382367327,-0.0776565856875276,
0.22050857199011));
#33977=CARTESIAN_POINT('Ctrl Pts',(-0.138689444093445,-0.0546588268893121,
0.219027549521503));
#33978=CARTESIAN_POINT('Ctrl Pts',(-0.146049272792313,-0.0272853980218952,
0.217546527052897));
#33979=CARTESIAN_POINT('Ctrl Pts',(-0.146129957599089,4.76874783713124E-5,
0.21606550458429));
#33980=CARTESIAN_POINT('Ctrl Pts',(-0.146134590291164,5.53529746073057E-5,
0.208934495415709));
#33981=CARTESIAN_POINT('Ctrl Pts',(-0.146039074200404,-0.0277987783441389,
0.210443872406129));
#33982=CARTESIAN_POINT('Ctrl Pts',(-0.138377421661147,-0.055701587485614,
0.21195324939655));
#33983=CARTESIAN_POINT('Ctrl Pts',(-0.123487844473835,-0.0789814939515912,
0.213462626386971));
#33984=CARTESIAN_POINT('Ctrl Pts',(-0.0974909500772326,-0.119627730063286,
0.216097967453477));
#33985=CARTESIAN_POINT('Ctrl Pts',(-0.0494601327803805,-0.146181306651382,
0.218733308519983));
#33986=CARTESIAN_POINT('Ctrl Pts',(-0.00121289818784218,-0.14658053417448,
0.221368649586488));
#33987=CARTESIAN_POINT('Ctrl Pts',(0.047034336404696,-0.146979761697578,
0.224003990652994));
#33988=CARTESIAN_POINT('Ctrl Pts',(0.0954979882929203,-0.121224640155678,
0.2266393317195));
#33989=CARTESIAN_POINT('Ctrl Pts',(0.122163941197393,-0.0810141690783142,
0.229274672786006));
#33990=CARTESIAN_POINT('Ctrl Pts',(0.148829894101866,-0.0408036980009502,
0.231910013852512));
#33991=CARTESIAN_POINT('Ctrl Pts',(0.153698148022588,0.0138621226118777,
0.234545354919018));
#33992=CARTESIAN_POINT('Ctrl Pts',(0.134557348601142,0.0581519050223658,
0.237180695985524));
#33993=CARTESIAN_POINT('Ctrl Pts',(0.115416549179696,0.102441687432854,
0.239816037052029));
#33994=CARTESIAN_POINT('Ctrl Pts',(0.0722666964160822,0.136355431641002,
0.242451378118535));
#33995=CARTESIAN_POINT('Ctrl Pts',(0.0247081678934101,0.144488167542617,
0.245086719185041));
#33996=CARTESIAN_POINT('Ctrl Pts',(-0.0228503606292616,0.152620903444231,
0.247722060251547));
#33997=CARTESIAN_POINT('Ctrl Pts',(-0.0748175649109913,0.134972631039312,
0.250357401318053));
#33998=CARTESIAN_POINT('Ctrl Pts',(-0.107587875971466,0.0995598968678148,
0.252992742384558));
#33999=CARTESIAN_POINT('Ctrl Pts',(-0.132216325719399,0.072945540282363,
0.254973326728275));
#34000=CARTESIAN_POINT('Ctrl Pts',(-0.146001912399175,0.0362973920726889,
0.256953911071992));
#34001=CARTESIAN_POINT('Ctrl Pts',(-0.146327394052832,-0.000130859996972892,
0.258934495415708));
#34002=CARTESIAN_POINT('Origin',(0.,0.,0.));
#34003=CARTESIAN_POINT('',(-0.146531331768327,7.78185235384022E-5,0.316065504584291));
#34004=CARTESIAN_POINT('',(-0.146550416329645,6.385150607816E-5,0.308934495415709));
#34005=CARTESIAN_POINT('',(-0.14635,-1.79227059055215E-17,0.));
#34006=CARTESIAN_POINT('Ctrl Pts',(-0.146531331768327,7.78185235384022E-5,
0.316065504584291));
#34007=CARTESIAN_POINT('Ctrl Pts',(-0.14656115307709,0.00468624689283061,
0.315814041177191));
#34008=CARTESIAN_POINT('Ctrl Pts',(-0.14636239679671,0.00929207042467623,
0.315562577770091));
#34009=CARTESIAN_POINT('Ctrl Pts',(-0.145926597573945,0.0138753548512781,
0.315311114362991));
#34010=CARTESIAN_POINT('Ctrl Pts',(-0.14136277093227,0.0618729520929492,
0.312677710408189));
#34011=CARTESIAN_POINT('Ctrl Pts',(-0.110802592512226,0.10739869970775,
0.310044306453387));
#34012=CARTESIAN_POINT('Ctrl Pts',(-0.0681090134487845,0.12980084606346,
0.307410902498584));
#34013=CARTESIAN_POINT('Ctrl Pts',(-0.0254154343853437,0.152202992419171,
0.304777498543782));
#34014=CARTESIAN_POINT('Ctrl Pts',(0.0294115453214934,0.151481537515791,
0.30214409458898));
#34015=CARTESIAN_POINT('Ctrl Pts',(0.0715008751789212,0.127963753463258,
0.299510690634177));
#34016=CARTESIAN_POINT('Ctrl Pts',(0.113590205036349,0.104445969410725,
0.296877286679375));
#34017=CARTESIAN_POINT('Ctrl Pts',(0.142941885044368,0.0581318562090376,
0.294243882724573));
#34018=CARTESIAN_POINT('Ctrl Pts',(0.146241172727074,0.0100307901566561,
0.291610478769771));
#34019=CARTESIAN_POINT('Ctrl Pts',(0.149540460409781,-0.038070275895725,
0.288977074814969));
#34020=CARTESIAN_POINT('Ctrl Pts',(0.126787355767176,-0.0879582947988004,
0.286343670860166));
#34021=CARTESIAN_POINT('Ctrl Pts',(0.0883033030491544,-0.117002666731855,
0.283710266905364));
#34022=CARTESIAN_POINT('Ctrl Pts',(0.0498192503311324,-0.14604703866491,
0.281076862950562));
#34023=CARTESIAN_POINT('Ctrl Pts',(-0.00439575046230666,-0.154247763627944,
0.27844345899576));
#34024=CARTESIAN_POINT('Ctrl Pts',(-0.0497482595792165,-0.137884763554925,
0.275810055040957));
#34025=CARTESIAN_POINT('Ctrl Pts',(-0.0951007686961262,-0.121521763481905,
0.273176651086155));
#34026=CARTESIAN_POINT('Ctrl Pts',(-0.131590786136507,-0.0805950383728307,
0.270543247131353));
#34027=CARTESIAN_POINT('Ctrl Pts',(-0.142665420037712,-0.0336700947016615,
0.26790984317655));
#34028=CARTESIAN_POINT('Ctrl Pts',(-0.145250841169412,-0.0227152638644948,
0.267295063645797));
#34029=CARTESIAN_POINT('Ctrl Pts',(-0.146451100522698,-0.0114335245988962,
0.266680284115044));
#34030=CARTESIAN_POINT('Ctrl Pts',(-0.146348968946192,-0.000130334789587572,
0.266065504584291));
#34031=CARTESIAN_POINT('Ctrl Pts',(-0.146327394052832,-0.000130859996972892,
0.258934495415708));
#34032=CARTESIAN_POINT('Ctrl Pts',(-0.146434994267663,-0.0121735902233998,
0.259589252138497));
#34033=CARTESIAN_POINT('Ctrl Pts',(-0.145071563913279,-0.0241922883978194,
0.260244008861286));
#34034=CARTESIAN_POINT('Ctrl Pts',(-0.142142543798705,-0.0358164956803284,
0.260898765584076));
#34035=CARTESIAN_POINT('Ctrl Pts',(-0.130353482726251,-0.0826029581188991,
0.263534106650581));
#34036=CARTESIAN_POINT('Ctrl Pts',(-0.0932019427421253,-0.122998687057965,
0.266169447717088));
#34037=CARTESIAN_POINT('Ctrl Pts',(-0.0475636294365445,-0.138654337383406,
0.268804788783593));
#34038=CARTESIAN_POINT('Ctrl Pts',(-0.00192531613096394,-0.154309987708848,
0.271440129850099));
#34039=CARTESIAN_POINT('Ctrl Pts',(0.0521997704960722,-0.145225559420664,
0.274075470916605));
#34040=CARTESIAN_POINT('Ctrl Pts',(0.090225865564854,-0.115527560795972,
0.27671081198311));
#34041=CARTESIAN_POINT('Ctrl Pts',(0.128251960633635,-0.0858295621712801,
0.279346153049616));
#34042=CARTESIAN_POINT('Ctrl Pts',(0.150179064144164,-0.0355179932100797,
0.281981494116122));
#34043=CARTESIAN_POINT('Ctrl Pts',(0.14604701445983,0.0125536324530514,
0.284616835182628));
#34044=CARTESIAN_POINT('Ctrl Pts',(0.141914964775496,0.0606252581161832,
0.287252176249134));
#34045=CARTESIAN_POINT('Ctrl Pts',(0.1117237618963,0.106456940481245,0.28988751731564));
#34046=CARTESIAN_POINT('Ctrl Pts',(0.0691874497467596,0.129230108403338,
0.292522858382145));
#34047=CARTESIAN_POINT('Ctrl Pts',(0.02665113759722,0.152003276325431,0.295158199448651));
#34048=CARTESIAN_POINT('Ctrl Pts',(-0.0282302838226635,0.151717929804555,
0.297793540515157));
#34049=CARTESIAN_POINT('Ctrl Pts',(-0.0705274923191129,0.128503684568086,
0.300428881581663));
#34050=CARTESIAN_POINT('Ctrl Pts',(-0.112824700815562,0.105289439331617,
0.303064222648169));
#34051=CARTESIAN_POINT('Ctrl Pts',(-0.142537696388578,0.0591462953795561,
0.305699563714675));
#34052=CARTESIAN_POINT('Ctrl Pts',(-0.146169655872548,0.0110343020847702,
0.30833490478118));
#34053=CARTESIAN_POINT('Ctrl Pts',(-0.146445102685266,0.00738550168790281,
0.308534768326023));
#34054=CARTESIAN_POINT('Ctrl Pts',(-0.146570540139926,0.00372537713102106,
0.308734631870866));
#34055=CARTESIAN_POINT('Ctrl Pts',(-0.146550416329645,6.385150607816E-5,
0.308934495415709));
#34056=CARTESIAN_POINT('Origin',(0.,0.,0.));
#34057=CARTESIAN_POINT('',(-0.146136883584905,5.71367125724795E-5,0.366065504584291));
#34058=CARTESIAN_POINT('',(-0.14615227160514,7.39083677616704E-5,0.358934495415709));
#34059=CARTESIAN_POINT('',(-0.14635,-1.79227059055215E-17,0.));
#34060=CARTESIAN_POINT('Ctrl Pts',(-0.146136883584905,5.71367125724795E-5,
0.366065504584291));
#34061=CARTESIAN_POINT('Ctrl Pts',(-0.14621004407594,0.0206825763459024,
0.364947798239338));
#34062=CARTESIAN_POINT('Ctrl Pts',(-0.142132997319362,0.0412803999606639,
0.363830091894385));
#34063=CARTESIAN_POINT('Ctrl Pts',(-0.133763205647759,0.0599541672162359,
0.362712385549432));
#34064=CARTESIAN_POINT('Ctrl Pts',(-0.114043318945497,0.10395102986619,
0.360078981594629));
#34065=CARTESIAN_POINT('Ctrl Pts',(-0.070493949429046,0.137267251375705,
0.357445577639827));
#34066=CARTESIAN_POINT('Ctrl Pts',(-0.0228703083824292,0.144789662428813,
0.354812173685025));
#34067=CARTESIAN_POINT('Ctrl Pts',(0.0247533326641879,0.15231207348192,
0.352178769730223));
#34068=CARTESIAN_POINT('Ctrl Pts',(0.0764512452409704,0.13404067407862,
0.34954536577542));
#34069=CARTESIAN_POINT('Ctrl Pts',(0.108771811167509,0.0982638817017563,
0.346911961820618));
#34070=CARTESIAN_POINT('Ctrl Pts',(0.141092377094047,0.0624870893248929,
0.344278557865816));
#34071=CARTESIAN_POINT('Ctrl Pts',(0.154035596370341,0.00920490397446603,
0.341645153911014));
#34072=CARTESIAN_POINT('Ctrl Pts',(0.141730062949927,-0.0374123857561472,
0.339011749956212));
#34073=CARTESIAN_POINT('Ctrl Pts',(0.129424529529512,-0.0840296754867619,
0.336378346001409));
#34074=CARTESIAN_POINT('Ctrl Pts',(0.0918702434123863,-0.123982069597563,
0.333744942046607));
#34075=CARTESIAN_POINT('Ctrl Pts',(0.0461028784809079,-0.139146045389481,
0.331111538091804));
#34076=CARTESIAN_POINT('Ctrl Pts',(0.000335513549430837,-0.154310021181399,
0.328478134137002));
#34077=CARTESIAN_POINT('Ctrl Pts',(-0.0536449301963988,-0.144685578654437,
0.3258447301822));
#34078=CARTESIAN_POINT('Ctrl Pts',(-0.0913514146376612,-0.114638633956686,
0.323211326227398));
#34079=CARTESIAN_POINT('Ctrl Pts',(-0.125457311698448,-0.0874608681681781,
0.320829385679696));
#34080=CARTESIAN_POINT('Ctrl Pts',(-0.146248854944573,-0.043574665631504,
0.318447445131993));
#34081=CARTESIAN_POINT('Ctrl Pts',(-0.146531331768327,7.78185235384022E-5,
0.316065504584291));
#34082=CARTESIAN_POINT('Ctrl Pts',(-0.146550416329645,6.385150607816E-5,
0.308934495415709));
#34083=CARTESIAN_POINT('Ctrl Pts',(-0.146305193582165,-0.0445544072241828,
0.311369972937372));
#34084=CARTESIAN_POINT('Ctrl Pts',(-0.1244453858937,-0.0893807124057277,
0.313805450459035));
#34085=CARTESIAN_POINT('Ctrl Pts',(-0.0890196886128741,-0.116459517256704,
0.316240927980698));
#34086=CARTESIAN_POINT('Ctrl Pts',(-0.0506868384743053,-0.145760500665881,
0.318876269047204));
#34087=CARTESIAN_POINT('Ctrl Pts',(0.00352978519775653,-0.154281624846726,
0.321511610113709));
#34088=CARTESIAN_POINT('Ctrl Pts',(0.0490028377607838,-0.138152256629371,
0.324146951180215));
#34089=CARTESIAN_POINT('Ctrl Pts',(0.0944758903238113,-0.122022888412016,
0.326782292246721));
#34090=CARTESIAN_POINT('Ctrl Pts',(0.131205371777804,-0.0812430277964604,
0.329417633313227));
#34091=CARTESIAN_POINT('Ctrl Pts',(0.142507292286359,-0.034336507766627,
0.332052974379733));
#34092=CARTESIAN_POINT('Ctrl Pts',(0.153809212794913,0.0125700122632054,
0.334688315446239));
#34093=CARTESIAN_POINT('Ctrl Pts',(0.139683572358031,0.0656031917073164,
0.337323656512744));
#34094=CARTESIAN_POINT('Ctrl Pts',(0.106546798111412,0.1006732533129,0.33995899757925));
#34095=CARTESIAN_POINT('Ctrl Pts',(0.0734100238647925,0.135743314918485,
0.342594338645756));
#34096=CARTESIAN_POINT('Ctrl Pts',(0.0212621158084357,0.152850258685541,
0.345229679712262));
#34097=CARTESIAN_POINT('Ctrl Pts',(-0.026209274243358,0.144223431050692,
0.347865020778768));
#34098=CARTESIAN_POINT('Ctrl Pts',(-0.0736806642951504,0.135596603415843,
0.350500361845274));
#34099=CARTESIAN_POINT('Ctrl Pts',(-0.11647553634238,0.10123600437909,0.353135702911779));
#34100=CARTESIAN_POINT('Ctrl Pts',(-0.135154759147093,0.056749583260925,
0.355771043978285));
#34101=CARTESIAN_POINT('Ctrl Pts',(-0.142628910530197,0.0389491506944377,
0.356825527790759));
#34102=CARTESIAN_POINT('Ctrl Pts',(-0.146242014510603,0.0195275186049996,
0.357880011603234));
#34103=CARTESIAN_POINT('Ctrl Pts',(-0.14615227160514,7.39083677616704E-5,
0.358934495415709));
#34104=CARTESIAN_POINT('Origin',(0.,0.,0.));
#34105=CARTESIAN_POINT('',(-0.146330070388523,-0.000130413829425732,0.416065504584291));
#34106=CARTESIAN_POINT('',(-0.146289342453438,-0.000128032530387096,0.408934495415709));
#34107=CARTESIAN_POINT('',(-0.14635,-1.79227059055215E-17,0.));
#34108=CARTESIAN_POINT('Ctrl Pts',(-0.146330070388523,-0.000130413829425732,
0.416065504584291));
#34109=CARTESIAN_POINT('Ctrl Pts',(-0.146004163689088,0.0363580550473478,
0.414081555301485));
#34110=CARTESIAN_POINT('Ctrl Pts',(-0.13216535679172,0.0730671490760677,
0.412097606018678));
#34111=CARTESIAN_POINT('Ctrl Pts',(-0.107460925463154,0.0996957714768259,
0.410113656735872));
#34112=CARTESIAN_POINT('Ctrl Pts',(-0.0746693880354573,0.135041392531165,
0.40748025278107));
#34113=CARTESIAN_POINT('Ctrl Pts',(-0.0227340340094623,0.152626534075836,
0.404846848826268));
#34114=CARTESIAN_POINT('Ctrl Pts',(0.0247858083562081,0.144474084374625,
0.402213444871466));
#34115=CARTESIAN_POINT('Ctrl Pts',(0.0723056507218785,0.136321634673413,
0.399580040916663));
#34116=CARTESIAN_POINT('Ctrl Pts',(0.115409981427224,0.102431593726319,
0.396946636961861));
#34117=CARTESIAN_POINT('Ctrl Pts',(0.134545471232452,0.0581774313853258,
0.394313233007059));
#34118=CARTESIAN_POINT('Ctrl Pts',(0.15368096103768,0.0139232690443328,
0.391679829052256));
#34119=CARTESIAN_POINT('Ctrl Pts',(0.14884760994279,-0.0406950146905586,
0.389046425097455));
#34120=CARTESIAN_POINT('Ctrl Pts',(0.122237961103967,-0.0809010396527884,
0.386413021142652));
#34121=CARTESIAN_POINT('Ctrl Pts',(0.0956283122651433,-0.121107064615018,
0.38377961718785));
#34122=CARTESIAN_POINT('Ctrl Pts',(0.0472423656823864,-0.146900830804586,
0.381146213233048));
#34123=CARTESIAN_POINT('Ctrl Pts',(-0.000970660813290544,-0.146581564902762,
0.378512809278245));
#34124=CARTESIAN_POINT('Ctrl Pts',(-0.0491836873089679,-0.146262299000937,
0.375879405323443));
#34125=CARTESIAN_POINT('Ctrl Pts',(-0.0972237937175652,-0.11983000100772,
0.373246001368641));
#34126=CARTESIAN_POINT('Ctrl Pts',(-0.123298644977828,-0.0792751001159155,
0.370612597413839));
#34127=CARTESIAN_POINT('Ctrl Pts',(-0.138306441127099,-0.0559330806595814,
0.369096899803989));
#34128=CARTESIAN_POINT('Ctrl Pts',(-0.146037672211633,-0.0279125797478292,
0.36758120219414));
#34129=CARTESIAN_POINT('Ctrl Pts',(-0.146136883584905,5.71367125724795E-5,
0.366065504584291));
#34130=CARTESIAN_POINT('Ctrl Pts',(-0.14615227160514,7.39083677616704E-5,
0.358934495415709));
#34131=CARTESIAN_POINT('Ctrl Pts',(-0.146017731158506,-0.0290904851457483,
0.36051535266974));
#34132=CARTESIAN_POINT('Ctrl Pts',(-0.137560931614845,-0.0583267505026361,
0.362096209923772));
#34133=CARTESIAN_POINT('Ctrl Pts',(-0.121314920725415,-0.0822800955868649,
0.363677067177803));
#34134=CARTESIAN_POINT('Ctrl Pts',(-0.0942322859368278,-0.122211110116912,
0.366312408244309));
#34135=CARTESIAN_POINT('Ctrl Pts',(-0.0455034427974572,-0.147460895977431,
0.368947749310814));
#34136=CARTESIAN_POINT('Ctrl Pts',(0.00273703201223555,-0.146559997189415,
0.37158309037732));
#34137=CARTESIAN_POINT('Ctrl Pts',(0.050977506821928,-0.145659098401399,
0.374218431443826));
#34138=CARTESIAN_POINT('Ctrl Pts',(0.0987296133019425,-0.11860751496485,
0.376853772510332));
#34139=CARTESIAN_POINT('Ctrl Pts',(0.124302447370845,-0.0776931509080149,
0.379489113576838));
#34140=CARTESIAN_POINT('Ctrl Pts',(0.149875281439748,-0.0367787868511801,
0.382124454643343));
#34141=CARTESIAN_POINT('Ctrl Pts',(0.153268843097537,0.0179983578259404,
0.384759795709849));
#34142=CARTESIAN_POINT('Ctrl Pts',(0.132941641804014,0.0617563275693305,
0.387395136776355));
#34143=CARTESIAN_POINT('Ctrl Pts',(0.112614440510491,0.10551429731272,0.39003047784286));
#34144=CARTESIAN_POINT('Ctrl Pts',(0.0685664762656556,0.13825309212238,
0.392665818909367));
#34145=CARTESIAN_POINT('Ctrl Pts',(0.0208060845723004,0.145101450596359,
0.395301159975872));
#34146=CARTESIAN_POINT('Ctrl Pts',(-0.0269543071210555,0.151949809070337,
0.397936501042378));
#34147=CARTESIAN_POINT('Ctrl Pts',(-0.0784271262629304,0.132907731208634,
0.400571842108884));
#34148=CARTESIAN_POINT('Ctrl Pts',(-0.110231373247062,0.0966248853684404,
0.40320718317539));
#34149=CARTESIAN_POINT('Ctrl Pts',(-0.133271130208243,0.0703407243117375,
0.405116287255496));
#34150=CARTESIAN_POINT('Ctrl Pts',(-0.145989017153952,0.0350087805988431,
0.407025391335602));
#34151=CARTESIAN_POINT('Ctrl Pts',(-0.146289342453438,-0.000128032530387096,
0.408934495415709));
#34152=CARTESIAN_POINT('Origin',(0.,0.,0.));
#34153=CARTESIAN_POINT('',(-0.146544022497492,6.84377374728824E-5,0.466065504584291));
#34154=CARTESIAN_POINT('',(-0.146570300119817,4.22437972465385E-5,0.458934495415709));
#34155=CARTESIAN_POINT('',(-0.14635,-1.79227059055215E-17,0.));
#34156=CARTESIAN_POINT('Ctrl Pts',(-0.146544022497492,6.84377374728824E-5,
0.466065504584291));
#34157=CARTESIAN_POINT('Ctrl Pts',(-0.146567170791634,0.00404048499144927,
0.465848716318434));
#34158=CARTESIAN_POINT('Ctrl Pts',(-0.146419528859516,0.00801078566506452,
0.465631928052577));
#34159=CARTESIAN_POINT('Ctrl Pts',(-0.146095506097533,0.0119666390378655,
0.46541513978672));
#34160=CARTESIAN_POINT('Ctrl Pts',(-0.142159486684863,0.0600197930006592,
0.462781735831918));
#34161=CARTESIAN_POINT('Ctrl Pts',(-0.112197024986195,0.105941128890497,
0.460148331877115));
#34162=CARTESIAN_POINT('Ctrl Pts',(-0.0697999311245908,0.128899445176305,
0.457514927922313));
#34163=CARTESIAN_POINT('Ctrl Pts',(-0.0274028372629858,0.151857761462114,
0.454881523967511));
#34164=CARTESIAN_POINT('Ctrl Pts',(0.0274288887615551,0.151853058143892,
0.452248120012709));
#34165=CARTESIAN_POINT('Ctrl Pts',(0.0698220433938502,0.12888746877825,
0.449614716057906));
#34166=CARTESIAN_POINT('Ctrl Pts',(0.112215198026145,0.105921879412608,
0.446981312103104));
#34167=CARTESIAN_POINT('Ctrl Pts',(0.142169781266193,0.0599954039995453,
0.444347908148302));
#34168=CARTESIAN_POINT('Ctrl Pts',(0.146097556879977,0.0119415755015296,
0.441714504193499));
#34169=CARTESIAN_POINT('Ctrl Pts',(0.150025332493762,-0.036112252996486,
0.439081100238697));
#34170=CARTESIAN_POINT('Ctrl Pts',(0.127926300481281,-0.0862934345794555,
0.436447696283895));
#34171=CARTESIAN_POINT('Ctrl Pts',(0.0898251994650805,-0.11583838264071,
0.433814292329093));
#34172=CARTESIAN_POINT('Ctrl Pts',(0.0517240984488793,-0.145383330701964,
0.431180888374291));
#34173=CARTESIAN_POINT('Ctrl Pts',(-0.00237907157104229,-0.154292045241502,
0.428547484419488));
#34174=CARTESIAN_POINT('Ctrl Pts',(-0.0479416004074503,-0.138523284332019,
0.425914080464686));
#34175=CARTESIAN_POINT('Ctrl Pts',(-0.0935041292438574,-0.122754523422536,
0.423280676509884));
#34176=CARTESIAN_POINT('Ctrl Pts',(-0.130526016896751,-0.0823082870640309,
0.420647272555081));
#34177=CARTESIAN_POINT('Ctrl Pts',(-0.142213100308499,-0.0355321186027758,
0.418013868600279));
#34178=CARTESIAN_POINT('Ctrl Pts',(-0.145095389184054,-0.0239960984301615,
0.417364413928283));
#34179=CARTESIAN_POINT('Ctrl Pts',(-0.146436757404375,-0.0120750773303437,
0.416714959256287));
#34180=CARTESIAN_POINT('Ctrl Pts',(-0.146330070388523,-0.000130413829425732,
0.416065504584291));
#34181=CARTESIAN_POINT('Ctrl Pts',(-0.146289342453438,-0.000128032530387096,
0.408934495415709));
#34182=CARTESIAN_POINT('Ctrl Pts',(-0.146403588367378,-0.0134943301275472,
0.409660732402108));
#34183=CARTESIAN_POINT('Ctrl Pts',(-0.144720893191604,-0.0268323904448261,
0.410386969388508));
#34184=CARTESIAN_POINT('Ctrl Pts',(-0.141125892037436,-0.0396334040556115,
0.411113206374907));
#34185=CARTESIAN_POINT('Ctrl Pts',(-0.128080489017291,-0.0860852338207874,
0.413748547441413));
#34186=CARTESIAN_POINT('Ctrl Pts',(-0.0898540081506159,-0.125465279532456,
0.416383888507919));
#34187=CARTESIAN_POINT('Ctrl Pts',(-0.0438104358868217,-0.139885559754408,
0.419019229574425));
#34188=CARTESIAN_POINT('Ctrl Pts',(0.00223313637697255,-0.15430583997636,
0.42165457064093));
#34189=CARTESIAN_POINT('Ctrl Pts',(0.0560938000378854,-0.143766354708596,
0.424289911707436));
#34190=CARTESIAN_POINT('Ctrl Pts',(0.0933059016336915,-0.11305455692152,
0.426925252773942));
#34191=CARTESIAN_POINT('Ctrl Pts',(0.130518003229497,-0.082342759134444,
0.429560593840448));
#34192=CARTESIAN_POINT('Ctrl Pts',(0.151081542760197,-0.0314586488280562,
0.432195934906954));
#34193=CARTESIAN_POINT('Ctrl Pts',(0.145655743526821,0.0164841893354265,
0.434831275973459));
#34194=CARTESIAN_POINT('Ctrl Pts',(0.140229944293446,0.06442702749891,0.437466617039965));
#34195=CARTESIAN_POINT('Ctrl Pts',(0.108814806295994,0.109428593519488,
0.440101958106471));
#34196=CARTESIAN_POINT('Ctrl Pts',(0.0656803334199076,0.131047388078691,
0.442737299172977));
#34197=CARTESIAN_POINT('Ctrl Pts',(0.022545860543821,0.152666182637894,
0.445372640239483));
#34198=CARTESIAN_POINT('Ctrl Pts',(-0.032307947210901,0.150902205735721,
0.448007981305989));
#34199=CARTESIAN_POINT('Ctrl Pts',(-0.0739643108743681,0.126556725768634,
0.450643322372494));
#34200=CARTESIAN_POINT('Ctrl Pts',(-0.115620674537836,0.102211245801546,
0.453278663439));
#34201=CARTESIAN_POINT('Ctrl Pts',(-0.144079594110048,0.0552842627695439,
0.455914004505506));
#34202=CARTESIAN_POINT('Ctrl Pts',(-0.14641389757273,0.0070918768996262,
0.458549345572012));
#34203=CARTESIAN_POINT('Ctrl Pts',(-0.146527615505388,0.00474413652285832,
0.458677728853244));
#34204=CARTESIAN_POINT('Ctrl Pts',(-0.146579333222338,0.00239339303023303,
0.458806112134477));
#34205=CARTESIAN_POINT('Ctrl Pts',(-0.146570300119817,4.22437972465385E-5,
0.458934495415709));
#34206=CARTESIAN_POINT('Origin',(0.,0.,0.));
#34207=CARTESIAN_POINT('',(-0.146145057762853,6.62388175271394E-5,0.516065504584291));
#34208=CARTESIAN_POINT('',(-0.146174937959923,9.05479403153491E-5,0.508934495415709));
#34209=CARTESIAN_POINT('',(-0.14635,-1.79227059055215E-17,0.));
#34210=CARTESIAN_POINT('Ctrl Pts',(-0.146145057762853,6.62388175271395E-5,
0.516065504584291));
#34211=CARTESIAN_POINT('Ctrl Pts',(-0.146227515408595,0.0200490060336265,
0.514982473380581));
#34212=CARTESIAN_POINT('Ctrl Pts',(-0.142408399519226,0.0400016020167204,
0.513899442176871));
#34213=CARTESIAN_POINT('Ctrl Pts',(-0.134535488644935,0.0582005124275171,
0.512816410973161));
#34214=CARTESIAN_POINT('Ctrl Pts',(-0.115392407114926,0.102451391335448,
0.510183007018359));
#34215=CARTESIAN_POINT('Ctrl Pts',(-0.0722822630505052,0.136334037036404,
0.507549603063556));
#34216=CARTESIAN_POINT('Ctrl Pts',(-0.0247610227936349,0.144478334368756,
0.504916199108754));
#34217=CARTESIAN_POINT('Ctrl Pts',(0.0227602174632348,0.152622631701108,
0.502282795153951));
#34218=CARTESIAN_POINT('Ctrl Pts',(0.0746925539125539,0.135028580664858,
0.49964939119915));
#34219=CARTESIAN_POINT('Ctrl Pts',(0.107478027152826,0.0996773345906346,
0.497015987244347));
#34220=CARTESIAN_POINT('Ctrl Pts',(0.140263500393099,0.06432608851641,0.494382583289545));
#34221=CARTESIAN_POINT('Ctrl Pts',(0.153902110424324,0.0112176474042102,
0.491749179334742));
#34222=CARTESIAN_POINT('Ctrl Pts',(0.142207002516364,-0.0355565153954619,
0.48911577537994));
#34223=CARTESIAN_POINT('Ctrl Pts',(0.130511894608405,-0.0823306781951331,
0.486482371425138));
#34224=CARTESIAN_POINT('Ctrl Pts',(0.0934830687612624,-0.122770562682277,
0.483848967470336));
#34225=CARTESIAN_POINT('Ctrl Pts',(0.0479178353914133,-0.138531506897017,
0.481215563515534));
#34226=CARTESIAN_POINT('Ctrl Pts',(0.00235260202156486,-0.154292451111757,
0.478582159560731));
#34227=CARTESIAN_POINT('Ctrl Pts',(-0.0517490388709899,-0.145374455054093,
0.475948755605929));
#34228=CARTESIAN_POINT('Ctrl Pts',(-0.0898450707539318,-0.115822971007387,
0.473315351651126));
#34229=CARTESIAN_POINT('Ctrl Pts',(-0.124804943950367,-0.0887042375336795,
0.470898735962181));
#34230=CARTESIAN_POINT('Ctrl Pts',(-0.146285980252562,-0.044209381789552,
0.468482120273236));
#34231=CARTESIAN_POINT('Ctrl Pts',(-0.146544022497492,6.84377374728824E-5,
0.466065504584291));
#34232=CARTESIAN_POINT('Ctrl Pts',(-0.146570300119817,4.22437972465385E-5,
0.458934495415709));
#34233=CARTESIAN_POINT('Ctrl Pts',(-0.14639390949893,-0.0458689668946884,
0.461441453200982));
#34234=CARTESIAN_POINT('Ctrl Pts',(-0.123052682342738,-0.0919348900534666,
0.463948410986256));
#34235=CARTESIAN_POINT('Ctrl Pts',(-0.0858494648887911,-0.118815796503266,
0.466455368771529));
#34236=CARTESIAN_POINT('Ctrl Pts',(-0.0467410413890165,-0.147073295328412,
0.469090709838035));
#34237=CARTESIAN_POINT('Ctrl Pts',(0.00768549296368549,-0.154130504270872,
0.471726050904541));
#34238=CARTESIAN_POINT('Ctrl Pts',(0.0527074437553312,-0.136781758627296,
0.474361391971047));
#34239=CARTESIAN_POINT('Ctrl Pts',(0.0977293945469769,-0.11943301298372,
0.476996733037553));
#34240=CARTESIAN_POINT('Ctrl Pts',(0.133346761777566,-0.0776783127541087,
0.479632074104058));
#34241=CARTESIAN_POINT('Ctrl Pts',(0.143380722078222,-0.0304843018080604,
0.482267415170564));
#34242=CARTESIAN_POINT('Ctrl Pts',(0.153414682378878,0.0167097091379873,
0.48490275623707));
#34243=CARTESIAN_POINT('Ctrl Pts',(0.137865235749601,0.0693430308004717,
0.487538097303576));
#34244=CARTESIAN_POINT('Ctrl Pts',(0.103795558670285,0.103507517218417,
0.490173438370082));
#34245=CARTESIAN_POINT('Ctrl Pts',(0.0697258815909678,0.137672003636362,
0.492808779436588));
#34246=CARTESIAN_POINT('Ctrl Pts',(0.0171359740616113,0.153367654809767,
0.495444120503093));
#34247=CARTESIAN_POINT('Ctrl Pts',(-0.0300857383810333,0.143464882345699,
0.498079461569599));
#34248=CARTESIAN_POINT('Ctrl Pts',(-0.0773074508236773,0.133562109881631,
0.500714802636104));
#34249=CARTESIAN_POINT('Ctrl Pts',(-0.11916096817961,0.09806091378009,0.503350143702611));
#34250=CARTESIAN_POINT('Ctrl Pts',(-0.136634759914189,0.0530873478673518,
0.505985484769117));
#34251=CARTESIAN_POINT('Ctrl Pts',(-0.143152625668081,0.0363118437555022,
0.506968488317981));
#34252=CARTESIAN_POINT('Ctrl Pts',(-0.146278417362408,0.0182184011065993,
0.507951491866845));
#34253=CARTESIAN_POINT('Ctrl Pts',(-0.146174937959923,9.05479403153491E-5,
0.508934495415709));
#34254=CARTESIAN_POINT('Origin',(0.,0.,0.));
#34255=CARTESIAN_POINT('',(-0.146311419053965,-0.000129619860865307,0.566065504584291));
#34256=CARTESIAN_POINT('',(-0.146253314944083,-0.00012165943743628,0.558934495415709));
#34257=CARTESIAN_POINT('',(-0.14635,-1.79227059055215E-17,0.));
#34258=CARTESIAN_POINT('Ctrl Pts',(-0.146311419053965,-0.000129619860865307,
0.566065504584291));
#34259=CARTESIAN_POINT('Ctrl Pts',(-0.145996667082224,0.0357327735863427,
0.564116230442728));
#34260=CARTESIAN_POINT('Ctrl Pts',(-0.132683527872108,0.0718042758553121,
0.562166956301165));
#34261=CARTESIAN_POINT('Ctrl Pts',(-0.10875495194318,0.0982825405633859,
0.560217682159602));
#34262=CARTESIAN_POINT('Ctrl Pts',(-0.0764282488179375,0.134053787671104,
0.557584278204799));
#34263=CARTESIAN_POINT('Ctrl Pts',(-0.0247272024587828,0.152316317789357,
0.554950874249997));
#34264=CARTESIAN_POINT('Ctrl Pts',(0.022895147382597,0.144785736790908,
0.552317470295194));
#34265=CARTESIAN_POINT('Ctrl Pts',(0.0705174972239762,0.13725515579246,
0.549684066340392));
#34266=CARTESIAN_POINT('Ctrl Pts',(0.11406115054758,0.103931463677311,0.54705066238559));
#34267=CARTESIAN_POINT('Ctrl Pts',(0.133773489094236,0.0599312186369601,
0.544417258430788));
#34268=CARTESIAN_POINT('Ctrl Pts',(0.153485827640893,0.0159309735966095,
0.541783854475986));
#34269=CARTESIAN_POINT('Ctrl Pts',(0.149366851410602,-0.038745824368944,
0.539150450521183));
#34270=CARTESIAN_POINT('Ctrl Pts',(0.123285043153097,-0.0792962514025479,
0.536517046566381));
#34271=CARTESIAN_POINT('Ctrl Pts',(0.097203234895591,-0.119846678436152,
0.533883642611579));
#34272=CARTESIAN_POINT('Ctrl Pts',(0.0491585946108714,-0.146270734537808,
0.531250238656777));
#34273=CARTESIAN_POINT('Ctrl Pts',(0.000945514053129371,-0.146581729267096,
0.528616834701974));
#34274=CARTESIAN_POINT('Ctrl Pts',(-0.0472675665046126,-0.146892723996384,
0.525983430747172));
#34275=CARTESIAN_POINT('Ctrl Pts',(-0.0956490873353763,-0.121090657353305,
0.523350026792369));
#34276=CARTESIAN_POINT('Ctrl Pts',(-0.122251838252959,-0.0808800679743115,
0.520716622837567));
#34277=CARTESIAN_POINT('Ctrl Pts',(-0.137913765110592,-0.057206752695483,
0.519166250086475));
#34278=CARTESIAN_POINT('Ctrl Pts',(-0.146027018608819,-0.0285393430688772,
0.517615877335383));
#34279=CARTESIAN_POINT('Ctrl Pts',(-0.146145057762853,6.62388175271395E-5,
0.516065504584291));
#34280=CARTESIAN_POINT('Ctrl Pts',(-0.146174937959923,9.05479403153491E-5,
0.508934495415709));
#34281=CARTESIAN_POINT('Ctrl Pts',(-0.146000998710948,-0.0303806868131737,
0.510586832933351));
#34282=CARTESIAN_POINT('Ctrl Pts',(-0.136702921110135,-0.060949146702594,
0.512239170450992));
#34283=CARTESIAN_POINT('Ctrl Pts',(-0.119053907816366,-0.0855189520167866,
0.513891507968634));
#34284=CARTESIAN_POINT('Ctrl Pts',(-0.0909051978707368,-0.124705750264253,
0.51652684903514));
#34285=CARTESIAN_POINT('Ctrl Pts',(-0.041513711866252,-0.148633411035251,
0.519162190101645));
#34286=CARTESIAN_POINT('Ctrl Pts',(0.00668497479873183,-0.146433040097983,
0.521797531168151));
#34287=CARTESIAN_POINT('Ctrl Pts',(0.0548836614637157,-0.144232669160716,
0.524432872234657));
#34288=CARTESIAN_POINT('Ctrl Pts',(0.101889548789197,-0.115904266515181,
0.527068213301163));
#34289=CARTESIAN_POINT('Ctrl Pts',(0.126350695083001,-0.0743157182057725,
0.529703554367669));
#34290=CARTESIAN_POINT('Ctrl Pts',(0.150811841376805,-0.0327271698963649,
0.532338895434175));
#34291=CARTESIAN_POINT('Ctrl Pts',(0.152728246638932,0.0221215240769157,
0.53497423650068));
#34292=CARTESIAN_POINT('Ctrl Pts',(0.131229403455446,0.0653159076268943,
0.537609577567186));
#34293=CARTESIAN_POINT('Ctrl Pts',(0.10973056027196,0.108510291176874,0.540244918633692));
#34294=CARTESIAN_POINT('Ctrl Pts',(0.0648164686428582,0.140050364303552,
0.542880259700198));
#34295=CARTESIAN_POINT('Ctrl Pts',(0.0168888935424139,0.145609372621787,
0.545515600766704));
#34296=CARTESIAN_POINT('Ctrl Pts',(-0.0310386815580289,0.151168380940021,
0.54815094183321));
#34297=CARTESIAN_POINT('Ctrl Pts',(-0.0819797401298146,0.130746324449814,
0.550786282899715));
#34298=CARTESIAN_POINT('Ctrl Pts',(-0.112794829345876,0.093619712631646,
0.553421623966221));
#34299=CARTESIAN_POINT('Ctrl Pts',(-0.134282196795419,0.0677313192961588,
0.555259247782717));
#34300=CARTESIAN_POINT('Ctrl Pts',(-0.145983763479016,0.0337207109540846,
0.557096871599213));
#34301=CARTESIAN_POINT('Ctrl Pts',(-0.146253314944083,-0.00012165943743628,
0.558934495415709));
#34302=CARTESIAN_POINT('Origin',(0.,0.,0.));
#34303=CARTESIAN_POINT('',(-0.146555285157174,5.84873774584615E-5,0.616065504584291));
#34304=CARTESIAN_POINT('',(-0.146582406651585,1.90495679610238E-5,0.608934495415709));
#34305=CARTESIAN_POINT('',(-0.14635,-1.79227059055215E-17,0.));
#34306=CARTESIAN_POINT('Ctrl Pts',(-0.146555285157174,5.84873774584615E-5,
0.616065504584291));
#34307=CARTESIAN_POINT('Ctrl Pts',(-0.146572323774182,0.00339452825839206,
0.615883391459677));
#34308=CARTESIAN_POINT('Ctrl Pts',(-0.146468182740347,0.00672948697362643,
0.615701278335063));
#34309=CARTESIAN_POINT('Ctrl Pts',(-0.146239449746585,0.0100558783590757,
0.615519165210449));
#34310=CARTESIAN_POINT('Ctrl Pts',(-0.142931910151921,0.0581563776955572,
0.612885761255647));
#34311=CARTESIAN_POINT('Ctrl Pts',(-0.113572285175357,0.10446545479915,
0.610252357300844));
#34312=CARTESIAN_POINT('Ctrl Pts',(-0.0714789213525946,0.127976017886268,
0.607618953346042));
#34313=CARTESIAN_POINT('Ctrl Pts',(-0.0293855575298321,0.151486580973386,
0.60498554939124));
#34314=CARTESIAN_POINT('Ctrl Pts',(0.0254415451391293,0.15219863004403,
0.602352145436437));
#34315=CARTESIAN_POINT('Ctrl Pts',(0.068131280382423,0.129789159736893,
0.599718741481635));
#34316=CARTESIAN_POINT('Ctrl Pts',(0.110821015625717,0.107379689429756,
0.597085337526833));
#34317=CARTESIAN_POINT('Ctrl Pts',(0.141373383443343,0.0618486997448399,
0.594451933572031));
#34318=CARTESIAN_POINT('Ctrl Pts',(0.145928975807906,0.0138503202638931,
0.591818529617228));
#34319=CARTESIAN_POINT('Ctrl Pts',(0.150484568172469,-0.0341480592170517,
0.589185125662426));
#34320=CARTESIAN_POINT('Ctrl Pts',(0.129043385083969,-0.0846138284940251,
0.586551721707624));
#34321=CARTESIAN_POINT('Ctrl Pts',(0.0913317465051492,-0.114654304027699,
0.583918317752822));
#34322=CARTESIAN_POINT('Ctrl Pts',(0.0536201079263286,-0.144694779561374,
0.58128491379802));
#34323=CARTESIAN_POINT('Ctrl Pts',(-0.000361986142813277,-0.154309961351749,
0.578651509843217));
#34324=CARTESIAN_POINT('Ctrl Pts',(-0.0461267489505717,-0.139138134179699,
0.576018105888415));
#34325=CARTESIAN_POINT('Ctrl Pts',(-0.0918915117583307,-0.123966307007649,
0.573384701933613));
#34326=CARTESIAN_POINT('Ctrl Pts',(-0.129438943304707,-0.0840074708731724,
0.57075129797881));
#34327=CARTESIAN_POINT('Ctrl Pts',(-0.141736479132229,-0.0373880707573429,
0.568117894024008));
#34328=CARTESIAN_POINT('Ctrl Pts',(-0.14493124569041,-0.0252768557512302,
0.567433764210769));
#34329=CARTESIAN_POINT('Ctrl Pts',(-0.146421886434131,-0.0127161165512012,
0.56674963439753));
#34330=CARTESIAN_POINT('Ctrl Pts',(-0.146311419053965,-0.000129619860865307,
0.566065504584291));
#34331=CARTESIAN_POINT('Ctrl Pts',(-0.146253314944083,-0.00012165943743628,
0.558934495415709));
#34332=CARTESIAN_POINT('Ctrl Pts',(-0.146370327932007,-0.0148127199255511,
0.559732212665719));
#34333=CARTESIAN_POINT('Ctrl Pts',(-0.144333034185812,-0.0294720768038573,
0.560529929915728));
#34334=CARTESIAN_POINT('Ctrl Pts',(-0.140006765979157,-0.0434215338335114,
0.561327647165738));
#34335=CARTESIAN_POINT('Ctrl Pts',(-0.125714493536039,-0.089505001334368,
0.563962988232244));
#34336=CARTESIAN_POINT('Ctrl Pts',(-0.0864408287894652,-0.127840769189951,
0.56659832929875));
#34337=CARTESIAN_POINT('Ctrl Pts',(-0.0400254307145004,-0.141015208458223,
0.569233670365256));
#34338=CARTESIAN_POINT('Ctrl Pts',(0.00638996736046498,-0.154189647726494,
0.571869011431762));
#34339=CARTESIAN_POINT('Ctrl Pts',(0.0599470987638218,-0.142202758407454,
0.574504352498268));
#34340=CARTESIAN_POINT('Ctrl Pts',(0.0963181864448715,-0.110499461900809,
0.577139693564773));
#34341=CARTESIAN_POINT('Ctrl Pts',(0.132689274125921,-0.0787961653941636,
0.579775034631279));
#34342=CARTESIAN_POINT('Ctrl Pts',(0.151874318084663,-0.0273764616999143,
0.582410375697785));
#34343=CARTESIAN_POINT('Ctrl Pts',(0.145158709082207,0.0204027767224063,
0.585045716764291));
#34344=CARTESIAN_POINT('Ctrl Pts',(0.138443100079752,0.0681820151447277,
0.587681057830797));
#34345=CARTESIAN_POINT('Ctrl Pts',(0.1058268381161,0.112320788295119,0.590316398897302));
#34346=CARTESIAN_POINT('Ctrl Pts',(0.0621255253059884,0.132769511657806,
0.592951739963808));
#34347=CARTESIAN_POINT('Ctrl Pts',(0.0184242124958778,0.153218235020492,
0.595587081030314));
#34348=CARTESIAN_POINT('Ctrl Pts',(-0.0363621511606923,0.149976908595474,
0.59822242209682));
#34349=CARTESIAN_POINT('Ctrl Pts',(-0.0773474224829438,0.124517871631514,
0.600857763163326));
#34350=CARTESIAN_POINT('Ctrl Pts',(-0.118332693805197,0.0990588346675542,
0.603493104229832));
#34351=CARTESIAN_POINT('Ctrl Pts',(-0.145516872793131,0.0513820871646532,
0.606128445296338));
#34352=CARTESIAN_POINT('Ctrl Pts',(-0.146551825250685,0.00314430216262847,
0.608763786362843));
#34353=CARTESIAN_POINT('Ctrl Pts',(-0.146574172232136,0.00210273848614761,
0.608820689380465));
#34354=CARTESIAN_POINT('Ctrl Pts',(-0.146584327751734,0.00106091323912811,
0.608877592398087));
#34355=CARTESIAN_POINT('Ctrl Pts',(-0.146582406651585,1.90495679610238E-5,
0.608934495415709));
#34356=CARTESIAN_POINT('Origin',(0.,0.,0.));
#34357=CARTESIAN_POINT('',(-0.146154441698478,7.49371236435786E-5,0.666065504584291));
#34358=CARTESIAN_POINT('',(-0.14620212788816,0.000104817362006062,0.658934495415709));
#34359=CARTESIAN_POINT('',(-0.14635,-1.79227059055215E-17,0.));
#34360=CARTESIAN_POINT('Ctrl Pts',(-0.146154441698478,7.49371236435786E-5,
0.666065504584291));
#34361=CARTESIAN_POINT('Ctrl Pts',(-0.146245091243546,0.019414808211501,
0.665017148521823));
#34362=CARTESIAN_POINT('Ctrl Pts',(-0.142674700046404,0.0387225584902945,
0.663968792459356));
#34363=CARTESIAN_POINT('Ctrl Pts',(-0.135284782149148,0.0564369123056677,
0.662920436396889));
#34364=CARTESIAN_POINT('Ctrl Pts',(-0.116721776970831,0.100934245858918,
0.660287032442087));
#34365=CARTESIAN_POINT('Ctrl Pts',(-0.074058225042023,0.13537752586737,
0.657653628487285));
#34366=CARTESIAN_POINT('Ctrl Pts',(-0.0266475060286977,0.144142317777245,
0.655020224532483));
#34367=CARTESIAN_POINT('Ctrl Pts',(0.020763212984627,0.15290710968712,0.652386820577681));
#34368=CARTESIAN_POINT('Ctrl Pts',(0.0729210990824686,0.13599341349842,
0.649753416622878));
#34369=CARTESIAN_POINT('Ctrl Pts',(0.106165877238123,0.101073754565802,
0.647120012668076));
#34370=CARTESIAN_POINT('Ctrl Pts',(0.139410655393777,0.0661540956331838,
0.644486608713273));
#34371=CARTESIAN_POINT('Ctrl Pts',(0.153742325607243,0.0132284739566488,
0.641853204758471));
#34372=CARTESIAN_POINT('Ctrl Pts',(0.142659641677727,-0.0336945691193152,
0.639219800803669));
#34373=CARTESIAN_POINT('Ctrl Pts',(0.13157695774821,-0.0806176121952798,
0.636586396848867));
#34374=CARTESIAN_POINT('Ctrl Pts',(0.09507991967571,-0.121538076670673,
0.633952992894065));
#34375=CARTESIAN_POINT('Ctrl Pts',(0.049724604077795,-0.137893296070049,
0.631319588939263));
#34376=CARTESIAN_POINT('Ctrl Pts',(0.00436928847988189,-0.154248515469425,
0.62868618498446));
#34377=CARTESIAN_POINT('Ctrl Pts',(-0.0498443046434454,-0.146038489792785,
0.626052781029658));
#34378=CARTESIAN_POINT('Ctrl Pts',(-0.0883233740987275,-0.116987516169781,
0.623419377074855));
#34379=CARTESIAN_POINT('Ctrl Pts',(-0.1241414224228,-0.0899455634453427,
0.620968086244667));
#34380=CARTESIAN_POINT('Ctrl Pts',(-0.146325940865162,-0.0448455053352938,
0.618516795414479));
#34381=CARTESIAN_POINT('Ctrl Pts',(-0.146555285157174,5.84873774584615E-5,
0.616065504584291));
#34382=CARTESIAN_POINT('Ctrl Pts',(-0.146582406651585,1.90495679610238E-5,
0.608934495415709));
#34383=CARTESIAN_POINT('Ctrl Pts',(-0.146495356123754,-0.0471907653725723,
0.611512933464593));
#34384=CARTESIAN_POINT('Ctrl Pts',(-0.121611930441545,-0.0944794748712001,
0.614091371513477));
#34385=CARTESIAN_POINT('Ctrl Pts',(-0.0826169041730041,-0.121085801253764,
0.616669809562361));
#34386=CARTESIAN_POINT('Ctrl Pts',(-0.042761304710591,-0.148279297166989,
0.619305150628866));
#34387=CARTESIAN_POINT('Ctrl Pts',(0.0118356201414113,-0.153867466492291,
0.621940491695373));
#34388=CARTESIAN_POINT('Ctrl Pts',(0.0563737778341691,-0.135311940689286,
0.624575832761878));
#34389=CARTESIAN_POINT('Ctrl Pts',(0.100911935526926,-0.116756414886282,
0.627211173828384));
#34390=CARTESIAN_POINT('Ctrl Pts',(0.135391326060439,-0.0740571939549723,
0.62984651489489));
#34391=CARTESIAN_POINT('Ctrl Pts',(0.144150040296483,-0.0266099605959858,
0.632481855961396));
#34392=CARTESIAN_POINT('Ctrl Pts',(0.152908754532526,0.0208372727630014,
0.635117197027901));
#34393=CARTESIAN_POINT('Ctrl Pts',(0.135946792471101,0.0730325185496646,
0.637752538094407));
#34394=CARTESIAN_POINT('Ctrl Pts',(0.100968951224381,0.106266622271745,
0.640387879160913));
#34395=CARTESIAN_POINT('Ctrl Pts',(0.0659911099776614,0.139500725993825,
0.643023220227419));
#34396=CARTESIAN_POINT('Ctrl Pts',(0.0129973895456473,0.153773687651321,
0.645658561293925));
#34397=CARTESIAN_POINT('Ctrl Pts',(-0.0339403566699702,0.14260216095667,
0.648293902360431));
#34398=CARTESIAN_POINT('Ctrl Pts',(-0.0808781028855877,0.131430634262018,
0.650929243426936));
#34399=CARTESIAN_POINT('Ctrl Pts',(-0.121759874884809,0.0948146192152183,
0.653564584493442));
#34400=CARTESIAN_POINT('Ctrl Pts',(-0.138015547484023,0.0493865647021963,
0.656199925559948));
#34401=CARTESIAN_POINT('Ctrl Pts',(-0.143638130564433,0.0336737106740469,
0.657111448845201));
#34402=CARTESIAN_POINT('Ctrl Pts',(-0.146314545676077,0.0169066195134479,
0.658022972130455));
#34403=CARTESIAN_POINT('Ctrl Pts',(-0.14620212788816,0.000104817362006062,
0.658934495415709));
#34404=CARTESIAN_POINT('Origin',(0.,0.,0.));
#34405=CARTESIAN_POINT('',(-0.146293122286189,-0.000127967976324597,0.716065504584291));
#34406=CARTESIAN_POINT('',(-0.146220133725287,-0.000111981377959844,0.708934495415709));
#34407=CARTESIAN_POINT('',(-0.14635,-1.79227059055215E-17,0.));
#34408=CARTESIAN_POINT('Ctrl Pts',(-0.146293122286189,-0.000127967976324597,
0.716065504584291));
#34409=CARTESIAN_POINT('Ctrl Pts',(-0.145991055868361,0.035107698155652,
0.714150905583971));
#34410=CARTESIAN_POINT('Ctrl Pts',(-0.133191339997662,0.0705402609933279,
0.71223630658365));
#34411=CARTESIAN_POINT('Ctrl Pts',(-0.110030394316881,0.0968525150836482,
0.71032170758333));
#34412=CARTESIAN_POINT('Ctrl Pts',(-0.0781740494934874,0.133043275639576,
0.707688303628528));
#34413=CARTESIAN_POINT('Ctrl Pts',(-0.0267161455114648,0.151980073612578,
0.705054899673726));
#34414=CARTESIAN_POINT('Ctrl Pts',(0.0210005740720494,0.145072648144428,
0.702421495718924));
#34415=CARTESIAN_POINT('Ctrl Pts',(0.0687172936555642,0.138165222676278,
0.699788091764121));
#34416=CARTESIAN_POINT('Ctrl Pts',(0.112692828840571,0.105413573766977,
0.697154687809319));
#34417=CARTESIAN_POINT('Ctrl Pts',(0.132978647675338,0.0616747648126076,
0.694521283854517));
#34418=CARTESIAN_POINT('Ctrl Pts',(0.153264466510106,0.0179359558582386,
0.691887879899714));
#34419=CARTESIAN_POINT('Ctrl Pts',(0.149860568994636,-0.0367900131411976,
0.689254475944912));
#34420=CARTESIAN_POINT('Ctrl Pts',(0.124311058190535,-0.0776779129690893,
0.68662107199011));
#34421=CARTESIAN_POINT('Ctrl Pts',(0.0987615473864338,-0.11856581279698,
0.683987668035308));
#34422=CARTESIAN_POINT('Ctrl Pts',(0.0510664232937013,-0.145615643453328,
0.681354264080505));
#34423=CARTESIAN_POINT('Ctrl Pts',(0.00286152734998743,-0.146556845670501,
0.678720860125703));
#34424=CARTESIAN_POINT('Ctrl Pts',(-0.0453433685937279,-0.147498047887674,
0.6760874561709));
#34425=CARTESIAN_POINT('Ctrl Pts',(-0.094058036388424,-0.122330621665673,
0.673454052216099));
#34426=CARTESIAN_POINT('Ctrl Pts',(-0.121184141071859,-0.082471215005648,
0.670820648261296));
#34427=CARTESIAN_POINT('Ctrl Pts',(-0.137511364617388,-0.0584798070786627,
0.669235600368961));
#34428=CARTESIAN_POINT('Ctrl Pts',(-0.146017385334238,-0.0291657216594994,
0.667650552476626));
#34429=CARTESIAN_POINT('Ctrl Pts',(-0.146154441698478,7.49371236435786E-5,
0.666065504584291));
#34430=CARTESIAN_POINT('Ctrl Pts',(-0.14620212788816,0.000104817362006062,
0.658934495415709));
#34431=CARTESIAN_POINT('Ctrl Pts',(-0.145989530157664,-0.0316697360413935,
0.660658313196961));
#34432=CARTESIAN_POINT('Ctrl Pts',(-0.135802925380645,-0.0635684301444077,
0.662382130978214));
#34433=CARTESIAN_POINT('Ctrl Pts',(-0.116706447513916,-0.088695711446933,
0.664105948759466));
#34434=CARTESIAN_POINT('Ctrl Pts',(-0.0875121017453893,-0.127109839103795,
0.666741289825971));
#34435=CARTESIAN_POINT('Ctrl Pts',(-0.0374938370091297,-0.149698000438276,
0.669376630892477));
#34436=CARTESIAN_POINT('Ctrl Pts',(0.0106280634930049,-0.146199755084551,
0.672011971958983));
#34437=CARTESIAN_POINT('Ctrl Pts',(0.0587499639951401,-0.142701509730827,
0.674647313025488));
#34438=CARTESIAN_POINT('Ctrl Pts',(0.104975500263151,-0.113116857688896,
0.677282654091995));
#34439=CARTESIAN_POINT('Ctrl Pts',(0.128307197060476,-0.0708843233930653,
0.679917995158501));
#34440=CARTESIAN_POINT('Ctrl Pts',(0.1516388938578,-0.0286517890972343,
0.682553336225006));
#34441=CARTESIAN_POINT('Ctrl Pts',(0.152076751184439,0.0262286274524959,
0.685188677291512));
#34442=CARTESIAN_POINT('Ctrl Pts',(0.129421876845612,0.06882806051419,0.687824018358017));
#34443=CARTESIAN_POINT('Ctrl Pts',(0.106767002506784,0.111427493575885,
0.690459359424523));
#34444=CARTESIAN_POINT('Ctrl Pts',(0.0610193965024891,0.141745943149541,
0.69309470049103));
#34445=CARTESIAN_POINT('Ctrl Pts',(0.0129594391535466,0.146011564806377,
0.695730041557535));
#34446=CARTESIAN_POINT('Ctrl Pts',(-0.0351005181953946,0.150277186463213,
0.698365382624041));
#34447=CARTESIAN_POINT('Ctrl Pts',(-0.0854728268889839,0.128489980203229,
0.701000723690547));
#34448=CARTESIAN_POINT('Ctrl Pts',(-0.115276382892,0.0905465607729482,0.703636064757053));
#34449=CARTESIAN_POINT('Ctrl Pts',(-0.135250024617843,0.0651177741718751,
0.705402208309938));
#34450=CARTESIAN_POINT('Ctrl Pts',(-0.145985488943994,0.0324326426859288,
0.707168351862824));
#34451=CARTESIAN_POINT('Ctrl Pts',(-0.146220133725287,-0.000111981377959844,
0.708934495415709));
#34452=CARTESIAN_POINT('Origin',(0.,0.,0.));
#34453=CARTESIAN_POINT('',(-0.146564965442509,4.80374956639621E-5,0.766065504584291));
#34454=CARTESIAN_POINT('',(-0.14658533994215,-4.90005960534454E-6,0.758934495415709));
#34455=CARTESIAN_POINT('',(-0.14635,-1.79227059055215E-17,0.));
#34456=CARTESIAN_POINT('Ctrl Pts',(-0.146564965442509,4.80374956639621E-5,
0.766065504584291));
#34457=CARTESIAN_POINT('Ctrl Pts',(-0.146576599691724,0.00274840678048242,
0.76591806660092));
#34458=CARTESIAN_POINT('Ctrl Pts',(-0.146508366823243,0.00544817658194007,
0.765770628617549));
#34459=CARTESIAN_POINT('Ctrl Pts',(-0.146358404344074,0.00814339894155673,
0.765623190634177));
#34460=CARTESIAN_POINT('Ctrl Pts',(-0.14367991012782,0.0562830238780745,
0.762989786679375));
#34461=CARTESIAN_POINT('Ctrl Pts',(-0.11492813804623,0.102971929623608,
0.760356382724573));
#34462=CARTESIAN_POINT('Ctrl Pts',(-0.0731456970048765,0.127030722191848,
0.757722978769771));
#34463=CARTESIAN_POINT('Ctrl Pts',(-0.031363255963523,0.151089514760089,
0.755089574814969));
#34464=CARTESIAN_POINT('Ctrl Pts',(0.023449854037593,0.152518194151036,
0.752456170860167));
#34465=CARTESIAN_POINT('Ctrl Pts',(0.0664288749466077,0.130668672151013,
0.749822766905364));
#34466=CARTESIAN_POINT('Ctrl Pts',(0.109407895855622,0.108819150150991,
0.747189362950562));
#34467=CARTESIAN_POINT('Ctrl Pts',(0.140552827672535,0.0636914267599971,
0.744555958995759));
#34468=CARTESIAN_POINT('Ctrl Pts',(0.145735458379408,0.0157566983326864,
0.741922555040957));
#34469=CARTESIAN_POINT('Ctrl Pts',(0.150918089086281,-0.0321780300946251,
0.739289151086155));
#34470=CARTESIAN_POINT('Ctrl Pts',(0.130138418683114,-0.0829197635582554,
0.736655747131352));
#34471=CARTESIAN_POINT('Ctrl Pts',(0.0928226866975336,-0.113450633258391,
0.73402234317655));
#34472=CARTESIAN_POINT('Ctrl Pts',(0.0555069547119538,-0.143981502958525,
0.731388939221748));
#34473=CARTESIAN_POINT('Ctrl Pts',(0.00165516114396223,-0.154301508895166,
0.728755535266946));
#34474=CARTESIAN_POINT('Ctrl Pts',(-0.0443040153143291,-0.139729208016517,
0.726122131312144));
#34475=CARTESIAN_POINT('Ctrl Pts',(-0.0902631917726212,-0.125156907137867,
0.723488727357341));
#34476=CARTESIAN_POINT('Ctrl Pts',(-0.128329751121212,-0.0856922994439281,
0.720855323402539));
#34477=CARTESIAN_POINT('Ctrl Pts',(-0.141235637963126,-0.0392376340275311,
0.718221919447737));
#34478=CARTESIAN_POINT('Ctrl Pts',(-0.144758384781757,-0.0265575271266455,
0.717503114493255));
#34479=CARTESIAN_POINT('Ctrl Pts',(-0.146406528193996,-0.0133566238911661,
0.716784309538773));
#34480=CARTESIAN_POINT('Ctrl Pts',(-0.146293122286189,-0.000127967976324597,
0.716065504584291));
#34481=CARTESIAN_POINT('Ctrl Pts',(-0.146220133725287,-0.000111981377959844,
0.708934495415709));
#34482=CARTESIAN_POINT('Ctrl Pts',(-0.146335612821056,-0.016128633179466,
0.709803692929329));
#34483=CARTESIAN_POINT('Ctrl Pts',(-0.143907730109974,-0.0321112532361818,
0.71067289044295));
#34484=CARTESIAN_POINT('Ctrl Pts',(-0.138785978242991,-0.047178134378496,
0.71154208795657));
#34485=CARTESIAN_POINT('Ctrl Pts',(-0.123257214278523,-0.0928597774990785,
0.714177429023076));
#34486=CARTESIAN_POINT('Ctrl Pts',(-0.0829648830371437,-0.130123431139663,
0.716812770089582));
#34487=CARTESIAN_POINT('Ctrl Pts',(-0.0362113622873864,-0.142042463234138,
0.719448111156088));
#34488=CARTESIAN_POINT('Ctrl Pts',(0.0105421584623702,-0.153961495328613,
0.722083452222593));
#34489=CARTESIAN_POINT('Ctrl Pts',(0.063756868720506,-0.140535905876979,
0.724718793289099));
#34490=CARTESIAN_POINT('Ctrl Pts',(0.0992605327204626,-0.107864131039655,
0.727354134355605));
#34491=CARTESIAN_POINT('Ctrl Pts',(0.13476419672042,-0.075192356202331,
0.729989475422111));
#34492=CARTESIAN_POINT('Ctrl Pts',(0.152556814462199,-0.0232743959793195,
0.732624816488617));
#34493=CARTESIAN_POINT('Ctrl Pts',(0.144556272029555,0.024306549251931,
0.735260157555123));
#34494=CARTESIAN_POINT('Ctrl Pts',(0.136555729596912,0.0718874944831808,
0.737895498621628));
#34495=CARTESIAN_POINT('Ctrl Pts',(0.102762026989844,0.115131424722669,
0.740530839688134));
#34496=CARTESIAN_POINT('Ctrl Pts',(0.058525606626993,0.13439522866968,0.74316618075464));
#34497=CARTESIAN_POINT('Ctrl Pts',(0.0142891862641413,0.15365903261669,
0.745801521821146));
#34498=CARTESIAN_POINT('Ctrl Pts',(-0.0403899518544944,0.148942710271224,
0.748436862887652));
#34499=CARTESIAN_POINT('Ctrl Pts',(-0.0806743706113798,0.122388602614794,
0.751072203954158));
#34500=CARTESIAN_POINT('Ctrl Pts',(-0.120735958293688,0.0959813775627587,
0.753692967774675));
#34501=CARTESIAN_POINT('Ctrl Pts',(-0.146561633397375,0.047977288078364,
0.756313731595192));
#34502=CARTESIAN_POINT('Ctrl Pts',(-0.14658533994215,-4.90005960534454E-6,
0.758934495415709));
#34503=CARTESIAN_POINT('Origin',(0.,0.,0.));
#34504=CARTESIAN_POINT('',(-0.146164975321328,8.31911013993853E-5,0.816065504584291));
#34505=CARTESIAN_POINT('',(-0.146233275186053,0.000116309547457056,0.808934495415709));
#34506=CARTESIAN_POINT('',(-0.14635,-1.79227059055215E-17,0.));
#34507=CARTESIAN_POINT('Ctrl Pts',(-0.146164975321328,8.31911013993853E-5,
0.816065504584291));
#34508=CARTESIAN_POINT('Ctrl Pts',(-0.146262710135629,0.0187799830896948,
0.815051823663067));
#34509=CARTESIAN_POINT('Ctrl Pts',(-0.142931951335767,0.037443276248974,
0.814038142741842));
#34510=CARTESIAN_POINT('Ctrl Pts',(-0.136010977838838,0.054663650141277,
0.813024461820618));
#34511=CARTESIAN_POINT('Ctrl Pts',(-0.118031238261729,0.0993998188524282,
0.810391057865816));
#34512=CARTESIAN_POINT('Ctrl Pts',(-0.0758215305972079,0.13439788253602,
0.807757653911014));
#34513=CARTESIAN_POINT('Ctrl Pts',(-0.028529425342275,0.143781679589591,
0.805124249956212));
#34514=CARTESIAN_POINT('Ctrl Pts',(0.0187626799126572,0.153165476643161,
0.80249084600141));
#34515=CARTESIAN_POINT('Ctrl Pts',(0.0711371827580015,0.136935007066712,
0.799857442046606));
#34516=CARTESIAN_POINT('Ctrl Pts',(0.104835580177757,0.102452897995539,
0.797224038091804));
#34517=CARTESIAN_POINT('Ctrl Pts',(0.138533977597513,0.0679707889243652,
0.794590634137002));
#34518=CARTESIAN_POINT('Ctrl Pts',(0.15355626959168,0.0152370403584678,
0.791957230182201));
#34519=CARTESIAN_POINT('Ctrl Pts',(0.143087905965057,-0.0318268624597296,
0.789323826227399));
#34520=CARTESIAN_POINT('Ctrl Pts',(0.132619542338435,-0.0788907652779263,
0.786690422272596));
#34521=CARTESIAN_POINT('Ctrl Pts',(0.096660523091021,-0.120284822348423,
0.784057018317793));
#34522=CARTESIAN_POINT('Ctrl Pts',(0.0515228742830193,-0.137231523355512,
0.781423614362991));
#34523=CARTESIAN_POINT('Ctrl Pts',(0.00638522547501753,-0.1541782243626,
0.778790210408188));
#34524=CARTESIAN_POINT('Ctrl Pts',(-0.0479310528935715,-0.146677569306282,
0.776156806453387));
#34525=CARTESIAN_POINT('Ctrl Pts',(-0.0867865839024083,-0.118132069714372,
0.773523402498585));
#34526=CARTESIAN_POINT('Ctrl Pts',(-0.123466686745614,-0.0911847643100577,
0.771037436527154));
#34527=CARTESIAN_POINT('Ctrl Pts',(-0.146368799251201,-0.045483147880463,
0.768551470555722));
#34528=CARTESIAN_POINT('Ctrl Pts',(-0.146564965442509,4.80374956639621E-5,
0.766065504584291));
#34529=CARTESIAN_POINT('Ctrl Pts',(-0.14658533994215,-4.90005960534454E-6,
0.758934495415709));
#34530=CARTESIAN_POINT('Ctrl Pts',(-0.146609310208618,-0.0485208624767226,
0.761584413728203));
#34531=CARTESIAN_POINT('Ctrl Pts',(-0.120122621218798,-0.0970137112575841,
0.764234332040698));
#34532=CARTESIAN_POINT('Ctrl Pts',(-0.0793243537302287,-0.123267883191947,
0.766884250353192));
#34533=CARTESIAN_POINT('Ctrl Pts',(-0.0387505182093485,-0.149377630477176,
0.769519591419698));
#34534=CARTESIAN_POINT('Ctrl Pts',(0.0159771533787021,-0.153492702582488,
0.772154932486204));
#34535=CARTESIAN_POINT('Ctrl Pts',(0.0599991778729333,-0.13374387011901,
0.77479027355271));
#34536=CARTESIAN_POINT('Ctrl Pts',(0.104021202367166,-0.113995037655531,
0.777425614619216));
#34537=CARTESIAN_POINT('Ctrl Pts',(0.13733757976758,-0.0703823006232647,
0.780060955685721));
#34538=CARTESIAN_POINT('Ctrl Pts',(0.14481468818493,-0.022716297290398,
0.782696296752227));
#34539=CARTESIAN_POINT('Ctrl Pts',(0.152291796602279,0.0249497060424673,
0.785331637818733));
#34540=CARTESIAN_POINT('Ctrl Pts',(0.133929636036564,0.0766689756759309,
0.787966978885239));
#34541=CARTESIAN_POINT('Ctrl Pts',(0.0980690284933123,0.108948564888508,
0.790602319951745));
#34542=CARTESIAN_POINT('Ctrl Pts',(0.0622084209500598,0.141228154101085,
0.793237661018251));
#34543=CARTESIAN_POINT('Ctrl Pts',(0.00884936642926935,0.154068062892775,
0.795873002084756));
#34544=CARTESIAN_POINT('Ctrl Pts',(-0.0377703306973942,0.141635893595607,
0.798508343151262));
#34545=CARTESIAN_POINT('Ctrl Pts',(-0.084390027824057,0.129203724298439,
0.801143684217768));
#34546=CARTESIAN_POINT('Ctrl Pts',(-0.124270367556593,0.0914994769124139,
0.803779025284273));
#34547=CARTESIAN_POINT('Ctrl Pts',(-0.139296118286606,0.0456499204587224,
0.806414366350779));
#34548=CARTESIAN_POINT('Ctrl Pts',(-0.144085736300807,0.0310348862098803,
0.807254409372422));
#34549=CARTESIAN_POINT('Ctrl Pts',(-0.146349920545361,0.0155922205493257,
0.808094452394066));
#34550=CARTESIAN_POINT('Ctrl Pts',(-0.146233275186053,0.000116309547457056,
0.808934495415709));
#34551=CARTESIAN_POINT('Origin',(0.,0.,0.));
#34552=CARTESIAN_POINT('',(-0.146273246343463,-0.000123611542196964,0.866065504584292));
#34553=CARTESIAN_POINT('',(-0.146190615322833,-9.92620605964336E-5,0.858934495415709));
#34554=CARTESIAN_POINT('',(-0.14635,-1.79227059055215E-17,0.));
#34555=CARTESIAN_POINT('Ctrl Pts',(-0.146273246343463,-0.000123611542196964,
0.866065504584292));
#34556=CARTESIAN_POINT('Ctrl Pts',(-0.14598570205562,0.0344841852260994,
0.864185580725214));
#34557=CARTESIAN_POINT('Ctrl Pts',(-0.13368920007778,0.0692748383916789,
0.862305656866136));
#34558=CARTESIAN_POINT('Ctrl Pts',(-0.111287960012964,0.0954050911579531,
0.860425733007059));
#34559=CARTESIAN_POINT('Ctrl Pts',(-0.0799082241293448,0.13200844115132,
0.857792329052257));
#34560=CARTESIAN_POINT('Ctrl Pts',(-0.0287004609307042,0.151617916172533,
0.855158925097454));
#34561=CARTESIAN_POINT('Ctrl Pts',(0.0191028994225217,0.145335216041435,
0.852525521142652));
#34562=CARTESIAN_POINT('Ctrl Pts',(0.0669062597757476,0.139052515910338,
0.84989211718785));
#34563=CARTESIAN_POINT('Ctrl Pts',(0.111305217283559,0.10687764062693,0.847258713233048));
#34564=CARTESIAN_POINT('Ctrl Pts',(0.132160826244895,0.0634075368078452,
0.844625309278246));
#34565=CARTESIAN_POINT('Ctrl Pts',(0.15301643520623,0.0199374329887607,
0.841991905323443));
#34566=CARTESIAN_POINT('Ctrl Pts',(0.15032869562109,-0.0348278993660004,
0.839358501368641));
#34567=CARTESIAN_POINT('Ctrl Pts',(0.12531596597325,-0.076046177073106,
0.836725097413839));
#34568=CARTESIAN_POINT('Ctrl Pts',(0.10030323632541,-0.117264454780212,
0.834091693459036));
#34569=CARTESIAN_POINT('Ctrl Pts',(0.0529655166148703,-0.144935677839662,
0.831458289504234));
#34570=CARTESIAN_POINT('Ctrl Pts',(0.00477698054298851,-0.14650698356075,
0.828824885549432));
#34571=CARTESIAN_POINT('Ctrl Pts',(-0.0434115555288926,-0.148078289281839,
0.826191481594629));
#34572=CARTESIAN_POINT('Ctrl Pts',(-0.0924509079621152,-0.123549677664568,
0.823558077639828));
#34573=CARTESIAN_POINT('Ctrl Pts',(-0.120095698433879,-0.084048234986577,
0.820924673685025));
#34574=CARTESIAN_POINT('Ctrl Pts',(-0.137099129982578,-0.059752153692848,
0.819304950651447));
#34575=CARTESIAN_POINT('Ctrl Pts',(-0.146008808497438,-0.0297917172680741,
0.817685227617869));
#34576=CARTESIAN_POINT('Ctrl Pts',(-0.146164975321328,8.31911013993853E-5,
0.816065504584291));
#34577=CARTESIAN_POINT('Ctrl Pts',(-0.146233275186053,0.000116309547457056,
0.808934495415709));
#34578=CARTESIAN_POINT('Ctrl Pts',(-0.145983986542363,-0.0329580355137906,
0.810729793460572));
#34579=CARTESIAN_POINT('Ctrl Pts',(-0.134860471440613,-0.0661842257005933,
0.812525091505434));
#34580=CARTESIAN_POINT('Ctrl Pts',(-0.114274246165196,-0.0918080661847913,
0.814320389550297));
#34581=CARTESIAN_POINT('Ctrl Pts',(-0.0840554615862833,-0.129421630853252,
0.816955730616803));
#34582=CARTESIAN_POINT('Ctrl Pts',(-0.0334467307009701,-0.150653894668816,
0.819591071683309));
#34583=CARTESIAN_POINT('Ctrl Pts',(0.0145634383780638,-0.145860313412396,
0.822226412749814));
#34584=CARTESIAN_POINT('Ctrl Pts',(0.0625736074570984,-0.141066732155975,
0.82486175381632));
#34585=CARTESIAN_POINT('Ctrl Pts',(0.107985214729854,-0.110247305827569,
0.827497094882826));
#34586=CARTESIAN_POINT('Ctrl Pts',(0.130170526119325,-0.0674014545208048,
0.830132435949332));
#34587=CARTESIAN_POINT('Ctrl Pts',(0.152355837508797,-0.0245556032140414,
0.832767777015837));
#34588=CARTESIAN_POINT('Ctrl Pts',(0.151314853014986,0.0303166730710795,
0.835403118082343));
#34589=CARTESIAN_POINT('Ctrl Pts',(0.127520386856677,0.0722902292399131,
0.838038459148849));
#34590=CARTESIAN_POINT('Ctrl Pts',(0.103725920698368,0.114263785408748,
0.840673800215355));
#34591=CARTESIAN_POINT('Ctrl Pts',(0.0571779728755602,0.143338621461295,
0.843309141281861));
#34592=CARTESIAN_POINT('Ctrl Pts',(0.00902055110528975,0.146307747926884,
0.845944482348367));
#34593=CARTESIAN_POINT('Ctrl Pts',(-0.0391368706649794,0.149276874392473,
0.848579823414872));
#34594=CARTESIAN_POINT('Ctrl Pts',(-0.088903766382711,0.126140291271107,
0.851215164481378));
#34595=CARTESIAN_POINT('Ctrl Pts',(-0.117674187241089,0.087407636925452,
0.853850505547884));
#34596=CARTESIAN_POINT('Ctrl Pts',(-0.136175085157248,0.0625004974853221,
0.855545168837159));
#34597=CARTESIAN_POINT('Ctrl Pts',(-0.145993587468369,0.0311441202011877,
0.857239832126434));
#34598=CARTESIAN_POINT('Ctrl Pts',(-0.146190615322833,-9.92620605964336E-5,
0.858934495415709));
#34599=CARTESIAN_POINT('Origin',(0.,0.,-0.0924367114736152));
#34600=CARTESIAN_POINT('',(-0.117713232580125,-9.94762513365651E-5,0.882563288526385));
#34601=CARTESIAN_POINT('',(-0.11796233779121,-2.11776828218935E-5,0.892436711473616));
#34602=CARTESIAN_POINT('',(-0.117775,-1.30487598617993E-14,-0.0924367114736152));
#34603=CARTESIAN_POINT('',(-0.11766859746431,0.00500517689819253,0.932224999999999));
#34604=CARTESIAN_POINT('Ctrl Pts',(-0.117713232580125,-9.94762513365794E-5,
0.882563288526385));
#34605=CARTESIAN_POINT('Ctrl Pts',(-0.117805978893427,-0.0112620890991194,
0.88331676862211));
#34606=CARTESIAN_POINT('Ctrl Pts',(-0.111244449407799,-0.0613316426944826,
0.886703652672637));
#34607=CARTESIAN_POINT('Ctrl Pts',(-0.0402800891732956,-0.133026134299755,
0.892723940677965));
#34608=CARTESIAN_POINT('Ctrl Pts',(0.0894243408305711,-0.10638650575871,
0.900624152542373));
#34609=CARTESIAN_POINT('Ctrl Pts',(0.137929356340621,0.0167100404698593,
0.908524364406779));
#34610=CARTESIAN_POINT('Ctrl Pts',(0.0614290966487016,0.124766721395902,
0.916424576271187));
#34611=CARTESIAN_POINT('Ctrl Pts',(-0.0710668305166857,0.11939070761148,
0.924324788135593));
#34612=CARTESIAN_POINT('Ctrl Pts',(-0.116012267804409,0.0439444575637681,
0.929591596045198));
#34613=CARTESIAN_POINT('Ctrl Pts',(-0.11766859746431,0.00500517689817995,
0.932225));
#34614=CARTESIAN_POINT('',(-0.0334019664626758,0.112939183906323,0.932224999999999));
#34615=CARTESIAN_POINT('Origin',(0.,0.,0.932225));
#34616=CARTESIAN_POINT('Ctrl Pts',(-0.11796233779121,-2.11776828218909E-5,
0.892436711473617));
#34617=CARTESIAN_POINT('Ctrl Pts',(-0.117965690360961,-0.00128932424828905,
0.892522768983215));
#34618=CARTESIAN_POINT('Ctrl Pts',(-0.117371901374032,-0.0413888390951994,
0.89524416755932));
#34619=CARTESIAN_POINT('Ctrl Pts',(-0.0720261204166176,-0.118897020856024,
0.90060090720193));
#34620=CARTESIAN_POINT('Ctrl Pts',(0.0602520802431792,-0.125231345176025,
0.908506930401448));
#34621=CARTESIAN_POINT('Ctrl Pts',(0.137949690524835,-0.017881538827179,
0.916412953600965));
#34622=CARTESIAN_POINT('Ctrl Pts',(0.0900118016872842,0.105886249500893,
0.924318976800482));
#34623=CARTESIAN_POINT('Ctrl Pts',(0.00399973323748277,0.12400080376067,
0.929589658933494));
#34624=CARTESIAN_POINT('Ctrl Pts',(-0.0334019664626807,0.112939183906322,
0.932225));
#34625=CARTESIAN_POINT('Origin',(0.,0.,-0.0924367114736152));
#34626=CARTESIAN_POINT('',(-0.117626101595281,6.69479464755203E-5,0.832563288526385));
#34627=CARTESIAN_POINT('',(-0.117646735358023,-7.98810330651378E-5,0.842436711473617));
#34628=CARTESIAN_POINT('',(-0.117775,-1.30487598617993E-14,-0.0924367114736152));
#34629=CARTESIAN_POINT('Ctrl Pts',(-0.117626101595281,6.69479464755242E-5,
0.832563288526385));
#34630=CARTESIAN_POINT('Ctrl Pts',(-0.117500426517155,-0.023974851392196,
0.834183011559963));
#34631=CARTESIAN_POINT('Ctrl Pts',(-0.0986730411655657,-0.0872854052949152,
0.838436138548343));
#34632=CARTESIAN_POINT('Ctrl Pts',(0.00452896330992775,-0.13890521184416,
0.845322669491525));
#34633=CARTESIAN_POINT('Ctrl Pts',(0.118813895436517,-0.0721000537472655,
0.853222881355933));
#34634=CARTESIAN_POINT('Ctrl Pts',(0.125302761776928,0.0601169674638447,
0.861123093220339));
#34635=CARTESIAN_POINT('Ctrl Pts',(0.0181127265090936,0.137795052940508,
0.869023305084746));
#34636=CARTESIAN_POINT('Ctrl Pts',(-0.0937244491952465,0.0949681812626695,
0.876170036853428));
#34637=CARTESIAN_POINT('Ctrl Pts',(-0.11748183163376,0.0277511097711188,
0.880683364667308));
#34638=CARTESIAN_POINT('Ctrl Pts',(-0.117713232580125,-9.94762513365794E-5,
0.882563288526385));
#34639=CARTESIAN_POINT('Ctrl Pts',(-0.117646735358023,-7.9881033065143E-5,
0.842436711473617));
#34640=CARTESIAN_POINT('Ctrl Pts',(-0.117734748084911,-0.0140363608293074,
0.843377389250847));
#34641=CARTESIAN_POINT('Ctrl Pts',(-0.108999987861276,-0.0669858868324248,
0.846953408094583));
#34642=CARTESIAN_POINT('Ctrl Pts',(-0.0306982239304521,-0.135581215292453,
0.853164768004825));
#34643=CARTESIAN_POINT('Ctrl Pts',(0.0968538014257187,-0.0997179081430208,
0.861070791204343));
#34644=CARTESIAN_POINT('Ctrl Pts',(0.136419444538435,0.0267352712365894,
0.86897681440386));
#34645=CARTESIAN_POINT('Ctrl Pts',(0.0520445414416943,0.128903423908239,
0.876882837603378));
#34646=CARTESIAN_POINT('Ctrl Pts',(-0.0781668699995673,0.11412164151165,
0.884702803293296));
#34647=CARTESIAN_POINT('Ctrl Pts',(-0.117863024541527,0.0375451567622119,
0.889887427916709));
#34648=CARTESIAN_POINT('Ctrl Pts',(-0.11796233779121,-2.11776828218909E-5,
0.892436711473617));
#34649=CARTESIAN_POINT('Origin',(0.,0.,-0.0924367114736152));
#34650=CARTESIAN_POINT('',(-0.117947993201171,3.86581212928119E-5,0.782563288526384));
#34651=CARTESIAN_POINT('',(-0.117681065835582,9.35999791555828E-5,0.792436711473616));
#34652=CARTESIAN_POINT('',(-0.117775,-1.30487598617993E-14,-0.0924367114736152));
#34653=CARTESIAN_POINT('Ctrl Pts',(-0.117947993201171,3.86581212928078E-5,
0.782563288526385));
#34654=CARTESIAN_POINT('Ctrl Pts',(-0.117790128676528,-0.0366025127545069,
0.785049254497816));
#34655=CARTESIAN_POINT('Ctrl Pts',(-0.0798361540276521,-0.112340416450435,
0.790168624424051));
#34656=CARTESIAN_POINT('Ctrl Pts',(0.0488494678181175,-0.130110898691923,
0.797921398305084));
#34657=CARTESIAN_POINT('Ctrl Pts',(0.135663410254684,-0.0301754342953877,
0.805821610169492));
#34658=CARTESIAN_POINT('Ctrl Pts',(0.0993958918478579,0.0971368425207782,
0.813721822033898));
#34659=CARTESIAN_POINT('Ctrl Pts',(-0.0270490771841315,0.136321199631122,
0.821622033898304));
#34660=CARTESIAN_POINT('Ctrl Pts',(-0.10806095418056,0.0691504233541856,
0.827902522729134));
#34661=CARTESIAN_POINT('Ctrl Pts',(-0.11770475357857,0.0151131705390384,
0.831549607605161));
#34662=CARTESIAN_POINT('Ctrl Pts',(-0.117626101595281,6.69479464755242E-5,
0.832563288526385));
#34663=CARTESIAN_POINT('Ctrl Pts',(-0.117681065835582,9.35999791555758E-5,
0.792436711473616));
#34664=CARTESIAN_POINT('Ctrl Pts',(-0.117480451076367,-0.0265229424847173,
0.794232009518479));
#34665=CARTESIAN_POINT('Ctrl Pts',(-0.0953885925249484,-0.0925118216380055,
0.798662648629848));
#34666=CARTESIAN_POINT('Ctrl Pts',(0.0138111005924944,-0.138325195186183,
0.80572862880772));
#34667=CARTESIAN_POINT('Ctrl Pts',(0.123445922182148,-0.0639194978340518,
0.813634652007238));
#34668=CARTESIAN_POINT('Ctrl Pts',(0.120932728835538,0.0685557124046954,
0.821540675206756));
#34669=CARTESIAN_POINT('Ctrl Pts',(0.0085545008581314,0.138749538494654,
0.829446698406273));
#34670=CARTESIAN_POINT('Ctrl Pts',(-0.0972993756118875,0.0895381706496827,
0.83641204382856));
#34671=CARTESIAN_POINT('Ctrl Pts',(-0.117488177410916,0.0250631961509614,
0.840742048184341));
#34672=CARTESIAN_POINT('Ctrl Pts',(-0.117646735358023,-7.9881033065143E-5,
0.842436711473617));
#34673=CARTESIAN_POINT('Origin',(0.,0.,-0.0924367114736152));
#34674=CARTESIAN_POINT('',(-0.117729227722965,-0.000102982086865302,0.732563288526385));
#34675=CARTESIAN_POINT('',(-0.117964389557135,-3.94331754086097E-6,0.742436711473616));
#34676=CARTESIAN_POINT('',(-0.117775,-1.30487598617993E-14,-0.0924367114736152));
#34677=CARTESIAN_POINT('Ctrl Pts',(-0.117729227722965,-0.000102982086865302,
0.732563288526385));
#34678=CARTESIAN_POINT('Ctrl Pts',(-0.117820491001352,-0.0107487282458691,
0.733282093480867));
#34679=CARTESIAN_POINT('Ctrl Pts',(-0.111634982628329,-0.060291927513671,
0.73663430239015));
#34680=CARTESIAN_POINT('Ctrl Pts',(-0.0420051819866054,-0.132478981273086,
0.742619915254238));
#34681=CARTESIAN_POINT('Ctrl Pts',(0.0880063312515965,-0.107563941317063,
0.750520127118644));
#34682=CARTESIAN_POINT('Ctrl Pts',(0.1381735813042,0.0149391196739674,0.758420338983051));
#34683=CARTESIAN_POINT('Ctrl Pts',(0.0629820334107182,0.123888575547709,
0.766320550847457));
#34684=CARTESIAN_POINT('Ctrl Pts',(-0.069350334823955,0.120439391087123,
0.774220762711865));
#34685=CARTESIAN_POINT('Ctrl Pts',(-0.116921686943853,0.0431900873220952,
0.77963500860484));
#34686=CARTESIAN_POINT('Ctrl Pts',(-0.117957355850309,0.00221177730489086,
0.782415850543013));
#34687=CARTESIAN_POINT('Ctrl Pts',(-0.117947993201171,3.86581212928078E-5,
0.782563288526385));
#34688=CARTESIAN_POINT('Ctrl Pts',(-0.117964389557135,-3.94331754086175E-6,
0.742436711473616));
#34689=CARTESIAN_POINT('Ctrl Pts',(-0.117964495672005,-0.000218720446770248,
0.742451288719605));
#34690=CARTESIAN_POINT('Ctrl Pts',(-0.117867006535742,-0.039261788207105,
0.745101207032099));
#34691=CARTESIAN_POINT('Ctrl Pts',(-0.0752264694457675,-0.116899882557203,
0.750386466411098));
#34692=CARTESIAN_POINT('Ctrl Pts',(0.0568996293847587,-0.126834681679914,
0.758292489610617));
#34693=CARTESIAN_POINT('Ctrl Pts',(0.137333582544999,-0.0215427765762162,
0.766198512810132));
#34694=CARTESIAN_POINT('Ctrl Pts',(0.0930027975645983,0.103320297856606,
0.774104536009652));
#34695=CARTESIAN_POINT('Ctrl Pts',(-0.035819122070238,0.13431900488649,
0.782010559209168));
#34696=CARTESIAN_POINT('Ctrl Pts',(-0.110236635830862,0.0639621230870467,
0.788121284363823));
#34697=CARTESIAN_POINT('Ctrl Pts',(-0.117774936058969,0.0125478221742061,
0.791596668451973));
#34698=CARTESIAN_POINT('Ctrl Pts',(-0.117681065835582,9.35999791555758E-5,
0.792436711473616));
#34699=CARTESIAN_POINT('Origin',(0.,0.,-0.0924367114736152));
#34700=CARTESIAN_POINT('',(-0.117617624673989,6.03055670430245E-5,0.682563288526385));
#34701=CARTESIAN_POINT('',(-0.117670490259622,-9.01168895870441E-5,0.692436711473616));
#34702=CARTESIAN_POINT('',(-0.117775,-1.30487598617993E-14,-0.0924367114736152));
#34703=CARTESIAN_POINT('Ctrl Pts',(-0.117617624673989,6.03055670430289E-5,
0.682563288526385));
#34704=CARTESIAN_POINT('Ctrl Pts',(-0.117507328717046,-0.0234710821212703,
0.68414833641872));
#34705=CARTESIAN_POINT('Ctrl Pts',(-0.0992894616255371,-0.0862548596187289,
0.688366788265857));
#34706=CARTESIAN_POINT('Ctrl Pts',(0.00271304928865532,-0.138952348570324,
0.695218644067796));
#34707=CARTESIAN_POINT('Ctrl Pts',(0.117860843754417,-0.0736473850127282,
0.703118855932203));
#34708=CARTESIAN_POINT('Ctrl Pts',(0.126078691992566,0.0584746033489104,
0.711019067796611));
#34709=CARTESIAN_POINT('Ctrl Pts',(0.0199109026571207,0.137545162630623,
0.718919279661016));
#34710=CARTESIAN_POINT('Ctrl Pts',(-0.0930178497353151,0.0959867468400004,
0.726100686570943));
#34711=CARTESIAN_POINT('Ctrl Pts',(-0.117486140108619,0.0282528811088558,
0.730648689526065));
#34712=CARTESIAN_POINT('Ctrl Pts',(-0.117729227722965,-0.000102982086865302,
0.732563288526385));
#34713=CARTESIAN_POINT('Ctrl Pts',(-0.117670490259622,-9.01168895870632E-5,
0.692436711473616));
#34714=CARTESIAN_POINT('Ctrl Pts',(-0.117763421933718,-0.0129794996427261,
0.693305908987236));
#34715=CARTESIAN_POINT('Ctrl Pts',(-0.109885703418251,-0.0648380928819097,
0.696810447567362));
#34716=CARTESIAN_POINT('Ctrl Pts',(-0.0343406886760894,-0.134704570618338,
0.702950327213994));
#34717=CARTESIAN_POINT('Ctrl Pts',(0.0941327483034478,-0.102291886006113,
0.710856350413511));
#34718=CARTESIAN_POINT('Ctrl Pts',(0.137088516418336,0.0230508765206803,
0.718762373613029));
#34719=CARTESIAN_POINT('Ctrl Pts',(0.0555021824679276,0.127452391053421,
0.726668396812546));
#34720=CARTESIAN_POINT('Ctrl Pts',(-0.0762633445254468,0.116087019895361,
0.734559842766075));
#34721=CARTESIAN_POINT('Ctrl Pts',(-0.117945311741555,0.0386096693093802,
0.739815947653099));
#34722=CARTESIAN_POINT('Ctrl Pts',(-0.117964389557135,-3.94331754086175E-6,
0.742436711473616));
#34723=CARTESIAN_POINT('Origin',(0.,0.,-0.0924367114736152));
#34724=CARTESIAN_POINT('',(-0.117940203002297,4.70676520639361E-5,0.632563288526384));
#34725=CARTESIAN_POINT('',(-0.117656000082187,8.43516556759474E-5,0.642436711473616));
#34726=CARTESIAN_POINT('',(-0.117775,-1.30487598617993E-14,-0.0924367114736152));
#34727=CARTESIAN_POINT('Ctrl Pts',(-0.117940203002297,4.7067652063935E-5,
0.632563288526384));
#34728=CARTESIAN_POINT('Ctrl Pts',(-0.117755638437952,-0.0360893706242894,
0.635014579356573));
#34729=CARTESIAN_POINT('Ctrl Pts',(-0.0807233593759693,-0.111374211355997,
0.640099274141563));
#34730=CARTESIAN_POINT('Ctrl Pts',(0.0471445089225743,-0.130738330601145,
0.647817372881356));
#34731=CARTESIAN_POINT('Ctrl Pts',(0.135257361515437,-0.0319462355497722,
0.655717584745763));
#34732=CARTESIAN_POINT('Ctrl Pts',(0.100657174442164,0.0958292702846084,
0.66361779661017));
#34733=CARTESIAN_POINT('Ctrl Pts',(-0.0252648283287276,0.136663104967713,
0.671518008474576));
#34734=CARTESIAN_POINT('Ctrl Pts',(-0.107599838532302,0.0701921319068488,
0.677833172446648));
#34735=CARTESIAN_POINT('Ctrl Pts',(-0.11769057479473,0.0156240453509343,
0.681514932463917));
#34736=CARTESIAN_POINT('Ctrl Pts',(-0.117617624673989,6.03055670430289E-5,
0.682563288526385));
#34737=CARTESIAN_POINT('Ctrl Pts',(-0.117656000082187,8.43516556759457E-5,
0.642436711473616));
#34738=CARTESIAN_POINT('Ctrl Pts',(-0.117484912294625,-0.0254861849147704,
0.644160529254868));
#34739=CARTESIAN_POINT('Ctrl Pts',(-0.0967548225821553,-0.0904011202578769,
0.648519688102626));
#34740=CARTESIAN_POINT('Ctrl Pts',(0.0100790193068892,-0.138647097388359,
0.655514188016889));
#34741=CARTESIAN_POINT('Ctrl Pts',(0.121678866262096,-0.0672224497442505,
0.663420211216407));
#34742=CARTESIAN_POINT('Ctrl Pts',(0.122735961854403,0.0652724131012164,
0.671326234415924));
#34743=CARTESIAN_POINT('Ctrl Pts',(0.0122899564463577,0.138468628991968,
0.679232257615441));
#34744=CARTESIAN_POINT('Ctrl Pts',(-0.0959511456548746,0.0916518108144888,
0.686269083301339));
#34745=CARTESIAN_POINT('Ctrl Pts',(-0.117481660132417,0.0261001331898457,
0.69067056792073));
#34746=CARTESIAN_POINT('Ctrl Pts',(-0.117670490259622,-9.01168895870632E-5,
0.692436711473616));
#34747=CARTESIAN_POINT('Origin',(0.,0.,-0.0924367114736152));
#34748=CARTESIAN_POINT('',(-0.117743952026517,-0.000104311439111954,0.582563288526385));
#34749=CARTESIAN_POINT('',(-0.11796202899481,1.53301186523688E-5,0.592436711473616));
#34750=CARTESIAN_POINT('',(-0.117775,-1.30487598617993E-14,-0.0924367114736152));
#34751=CARTESIAN_POINT('Ctrl Pts',(-0.117743952026517,-0.000104311439111965,
0.582563288526385));
#34752=CARTESIAN_POINT('Ctrl Pts',(-0.117832850528047,-0.0102332806752188,
0.583247418339623));
#34753=CARTESIAN_POINT('Ctrl Pts',(-0.112015701243022,-0.0592509231652696,
0.586564952107665));
#34754=CARTESIAN_POINT('Ctrl Pts',(-0.0437333382095171,-0.131918576929031,
0.592515889830509));
#34755=CARTESIAN_POINT('Ctrl Pts',(0.0865927525795457,-0.108705156320324,
0.600416101694915));
#34756=CARTESIAN_POINT('Ctrl Pts',(0.138357057429181,0.0131316590523252,
0.608316313559322));
#34757=CARTESIAN_POINT('Ctrl Pts',(0.0645961051971127,0.123054699232873,
0.616216525423729));
#34758=CARTESIAN_POINT('Ctrl Pts',(-0.0677700447892944,0.121335637135943,
0.624116737288135));
#34759=CARTESIAN_POINT('Ctrl Pts',(-0.116658230525945,0.0442240676066805,
0.629565658322354));
#34760=CARTESIAN_POINT('Ctrl Pts',(-0.117953914810415,0.00273174284681649,
0.63238117540177));
#34761=CARTESIAN_POINT('Ctrl Pts',(-0.117940203002297,4.7067652063935E-5,
0.632563288526384));
#34762=CARTESIAN_POINT('Ctrl Pts',(-0.11796202899481,1.53301186523688E-5,
0.592436711473616));
#34763=CARTESIAN_POINT('Ctrl Pts',(-0.11789197517919,-0.0379767160352311,
0.5950151495225));
#34764=CARTESIAN_POINT('Ctrl Pts',(-0.077400231210687,-0.114927628746102,
0.600228928637889));
#34765=CARTESIAN_POINT('Ctrl Pts',(0.0534615168199478,-0.12832174587234,
0.608078048819785));
#34766=CARTESIAN_POINT('Ctrl Pts',(0.136703270562712,-0.0252352939724056,
0.615984072019302));
#34767=CARTESIAN_POINT('Ctrl Pts',(0.0957529101571512,0.100776904302778,
0.623890095218819));
#34768=CARTESIAN_POINT('Ctrl Pts',(-0.0321870028708045,0.135235354440354,
0.631796118418337));
#34769=CARTESIAN_POINT('Ctrl Pts',(-0.109365567925802,0.0661098894434327,
0.637978323836602));
#34770=CARTESIAN_POINT('Ctrl Pts',(-0.117746468172191,0.0136055832811398,
0.641525188188362));
#34771=CARTESIAN_POINT('Ctrl Pts',(-0.117656000082187,8.43516556759457E-5,
0.642436711473616));
#34772=CARTESIAN_POINT('Origin',(0.,0.,-0.0924367114736152));
#34773=CARTESIAN_POINT('',(-0.117610072962214,5.33056148506657E-5,0.532563288526385));
#34774=CARTESIAN_POINT('',(-0.117697192808605,-9.79052972080175E-5,0.542436711473616));
#34775=CARTESIAN_POINT('',(-0.117775,-1.30487598617993E-14,-0.0924367114736152));
#34776=CARTESIAN_POINT('Ctrl Pts',(-0.117610072962214,5.330561485066E-5,
0.532563288526385));
#34777=CARTESIAN_POINT('Ctrl Pts',(-0.117515081084069,-0.02296700464597,
0.534113661277477));
#34778=CARTESIAN_POINT('Ctrl Pts',(-0.0998958154709599,-0.0852230040130838,
0.538297437983371));
#34779=CARTESIAN_POINT('Ctrl Pts',(0.000896453507092177,-0.13897594101512,
0.545114618644068));
#34780=CARTESIAN_POINT('Ctrl Pts',(0.116888066275103,-0.0751817515916976,
0.553014830508475));
#34781=CARTESIAN_POINT('Ctrl Pts',(0.126832290918542,0.0568215257651788,
0.560915042372882));
#34782=CARTESIAN_POINT('Ctrl Pts',(0.0217071709283622,0.137273138451102,
0.568815254237287));
#34783=CARTESIAN_POINT('Ctrl Pts',(-0.0923030266130234,0.097000942567024,
0.576031336288457));
#34784=CARTESIAN_POINT('Ctrl Pts',(-0.117490655726745,0.0287559098676526,
0.580614014384821));
#34785=CARTESIAN_POINT('Ctrl Pts',(-0.117743952026517,-0.000104311439111965,
0.582563288526385));
#34786=CARTESIAN_POINT('Ctrl Pts',(-0.117697192808605,-9.79052972080122E-5,
0.542436711473616));
#34787=CARTESIAN_POINT('Ctrl Pts',(-0.11779135888071,-0.011920519912767,
0.543234428723626));
#34788=CARTESIAN_POINT('Ctrl Pts',(-0.110735559311442,-0.0626905594030618,
0.546667487040141));
#34789=CARTESIAN_POINT('Ctrl Pts',(-0.0379577228913647,-0.133730383672961,
0.552735886423163));
#34790=CARTESIAN_POINT('Ctrl Pts',(0.0913424031974019,-0.104791076063462,
0.56064190962268));
#34791=CARTESIAN_POINT('Ctrl Pts',(0.137659831668342,0.0193487722984857,
0.568547932822197));
#34792=CARTESIAN_POINT('Ctrl Pts',(0.0589161298691768,0.125910658348106,
0.576453956021715));
#34793=CARTESIAN_POINT('Ctrl Pts',(-0.0733516660922674,0.11808529682354,
0.584359979221232));
#34794=CARTESIAN_POINT('Ctrl Pts',(-0.117576903938907,0.0405212291720611,
0.589687564371866));
#34795=CARTESIAN_POINT('Ctrl Pts',(-0.117963574998021,0.000853768751192661,
0.592379808455994));
#34796=CARTESIAN_POINT('Ctrl Pts',(-0.11796202899481,1.53301186523688E-5,
0.592436711473616));
#34797=CARTESIAN_POINT('Origin',(0.,0.,-0.0924367114736152));
#34798=CARTESIAN_POINT('',(-0.117931139389423,5.50751932371175E-5,0.482563288526385));
#34799=CARTESIAN_POINT('',(-0.117634119017629,7.2868354416035E-5,0.492436711473616));
#34800=CARTESIAN_POINT('',(-0.117775,-1.30487598617993E-14,-0.0924367114736152));
#34801=CARTESIAN_POINT('Ctrl Pts',(-0.117931139389423,5.50751932371233E-5,
0.482563288526385));
#34802=CARTESIAN_POINT('Ctrl Pts',(-0.117723480179333,-0.0355774509071747,
0.48497990421533));
#34803=CARTESIAN_POINT('Ctrl Pts',(-0.0815990427908323,-0.11040399129502,
0.490029923859077));
#34804=CARTESIAN_POINT('Ctrl Pts',(0.0454314893010671,-0.131343426138561,
0.497713347457628));
#34805=CARTESIAN_POINT('Ctrl Pts',(0.134828208757446,-0.0337115697229769,
0.505613559322033));
#34806=CARTESIAN_POINT('Ctrl Pts',(0.10190123992053,0.0945053073249706,
0.513513771186441));
#34807=CARTESIAN_POINT('Ctrl Pts',(-0.0234762303627364,0.136981686432473,
0.521413983050847));
#34808=CARTESIAN_POINT('Ctrl Pts',(-0.107129919570411,0.0712336270252472,
0.527763822164162));
#34809=CARTESIAN_POINT('Ctrl Pts',(-0.117676430661069,0.0161344153441048,
0.531480257322675));
#34810=CARTESIAN_POINT('Ctrl Pts',(-0.117610072962214,5.330561485066E-5,
0.532563288526385));
#34811=CARTESIAN_POINT('Ctrl Pts',(-0.117634119017629,7.28683544160419E-5,
0.492436711473616));
#34812=CARTESIAN_POINT('Ctrl Pts',(-0.117494141600147,-0.0244488239796579,
0.494089048991258));
#34813=CARTESIAN_POINT('Ctrl Pts',(-0.0980773705094754,-0.0882836093782272,
0.498376727575405));
#34814=CARTESIAN_POINT('Ctrl Pts',(0.00633962999064621,-0.138868330932566,
0.505299747226058));
#34815=CARTESIAN_POINT('Ctrl Pts',(0.119823436886959,-0.0704765792090683,
0.513205770425575));
#34816=CARTESIAN_POINT('Ctrl Pts',(0.124450111907394,0.0619416975118724,
0.521111793625093));
#34817=CARTESIAN_POINT('Ctrl Pts',(0.0160164158031762,0.138087213996209,
0.52901781682461));
#34818=CARTESIAN_POINT('Ctrl Pts',(-0.0945587588515482,0.0937580907599652,
0.536126122774119));
#34819=CARTESIAN_POINT('Ctrl Pts',(-0.117480271566393,0.0271367046984328,
0.54059908765712));
#34820=CARTESIAN_POINT('Ctrl Pts',(-0.117697192808605,-9.79052972080122E-5,
0.542436711473616));
#34821=CARTESIAN_POINT('Origin',(0.,0.,-0.0924367114736152));
#34822=CARTESIAN_POINT('',(-0.117758961667293,-0.000104950384427651,0.432563288526384));
#34823=CARTESIAN_POINT('',(-0.117952286276812,3.39956489144189E-5,0.442436711473616));
#34824=CARTESIAN_POINT('',(-0.117775,-1.30487598617993E-14,-0.0924367114736152));
#34825=CARTESIAN_POINT('Ctrl Pts',(-0.117758961667293,-0.000104950384427652,
0.432563288526384));
#34826=CARTESIAN_POINT('Ctrl Pts',(-0.117844817924839,-0.00971740507401162,
0.43321274319838));
#34827=CARTESIAN_POINT('Ctrl Pts',(-0.11238834839588,-0.0582101957930696,
0.436495601825179));
#34828=CARTESIAN_POINT('Ctrl Pts',(-0.045454021205161,-0.13133563022352,
0.44241186440678));
#34829=CARTESIAN_POINT('Ctrl Pts',(0.085164376794762,-0.109827795821861,
0.450312076271186));
#34830=CARTESIAN_POINT('Ctrl Pts',(0.138516891217783,0.0113219546585138,
0.458212288135593));
#34831=CARTESIAN_POINT('Ctrl Pts',(0.0661991384108791,0.12219979494085,
0.4661125));
#34832=CARTESIAN_POINT('Ctrl Pts',(-0.0661781734963363,0.122211149911198,
0.474012711864406));
#34833=CARTESIAN_POINT('Ctrl Pts',(-0.116387669202521,0.0452586237679377,
0.479496308039868));
#34834=CARTESIAN_POINT('Ctrl Pts',(-0.117949767953432,0.00325157581050499,
0.482346500260528));
#34835=CARTESIAN_POINT('Ctrl Pts',(-0.117931139389423,5.50751932371233E-5,
0.482563288526385));
#34836=CARTESIAN_POINT('Ctrl Pts',(-0.117952286276812,3.39956489144155E-5,
0.442436711473616));
#34837=CARTESIAN_POINT('Ctrl Pts',(-0.117810336120504,-0.0369130001778165,
0.444943669258889));
#34838=CARTESIAN_POINT('Ctrl Pts',(-0.0792807483010678,-0.11295446192069,
0.450085968110668));
#34839=CARTESIAN_POINT('Ctrl Pts',(0.0499845850166584,-0.129715633233345,
0.457863608028953));
#34840=CARTESIAN_POINT('Ctrl Pts',(0.135973695209673,-0.0289094872912353,
0.465769631228471));
#34841=CARTESIAN_POINT('Ctrl Pts',(0.0984334954810092,0.0981603342078928,
0.473675654427988));
#34842=CARTESIAN_POINT('Ctrl Pts',(-0.0285315135918273,0.136053507770195,
0.481581677627505));
#34843=CARTESIAN_POINT('Ctrl Pts',(-0.108458155672614,0.0682577387762276,
0.487835363309382));
#34844=CARTESIAN_POINT('Ctrl Pts',(-0.117717393951882,0.0146612380616908,
0.491453707924752));
#34845=CARTESIAN_POINT('Ctrl Pts',(-0.117634119017629,7.28683544160419E-5,
0.492436711473616));
#34846=CARTESIAN_POINT('Origin',(0.,0.,-0.0924367114736152));
#34847=CARTESIAN_POINT('',(-0.117603494801586,4.59807059966066E-5,0.382563288526384));
#34848=CARTESIAN_POINT('',(-0.117726185906756,-0.000103034036682964,0.392436711473616));
#34849=CARTESIAN_POINT('',(-0.117775,-1.30487598617993E-14,-0.0924367114736152));
#34850=CARTESIAN_POINT('Ctrl Pts',(-0.117603494801586,4.59807059966007E-5,
0.382563288526384));
#34851=CARTESIAN_POINT('Ctrl Pts',(-0.117523654559104,-0.0224626175592834,
0.384078986136234));
#34852=CARTESIAN_POINT('Ctrl Pts',(-0.100492247037195,-0.0841899886309759,
0.388228087700885));
#34853=CARTESIAN_POINT('Ctrl Pts',(-0.000920295459793275,-0.138975785179272,
0.395010593220339));
#34854=CARTESIAN_POINT('Ctrl Pts',(0.115895314901344,-0.0767032710765764,
0.402910805084745));
#34855=CARTESIAN_POINT('Ctrl Pts',(0.127564216682018,0.0551587384938402,
0.410811016949152));
#34856=CARTESIAN_POINT('Ctrl Pts',(0.0234997298595607,0.136977656960748,
0.418711228813559));
#34857=CARTESIAN_POINT('Ctrl Pts',(-0.0915774899741938,0.0980128855194841,
0.42596198600597));
#34858=CARTESIAN_POINT('Ctrl Pts',(-0.117496688612794,0.0292591044291153,
0.430579339243578));
#34859=CARTESIAN_POINT('Ctrl Pts',(-0.117758961667293,-0.000104950384427652,
0.432563288526384));
#34860=CARTESIAN_POINT('Ctrl Pts',(-0.117726185906756,-0.000103034036682944,
0.392436711473616));
#34861=CARTESIAN_POINT('Ctrl Pts',(-0.117818125179144,-0.0108595471866994,
0.393162948460015));
#34862=CARTESIAN_POINT('Ctrl Pts',(-0.111550100869322,-0.0605437012261054,
0.39652452651292));
#34863=CARTESIAN_POINT('Ctrl Pts',(-0.0415471952570256,-0.13265909245389,
0.40252144563233));
#34864=CARTESIAN_POINT('Ctrl Pts',(0.0884857325734624,-0.107214175253801,
0.410427468831849));
#34865=CARTESIAN_POINT('Ctrl Pts',(0.138131189387156,0.0156326185555932,
0.418333492031365));
#34866=CARTESIAN_POINT('Ctrl Pts',(0.062287297122381,0.124277499418049,
0.426239515230884));
#34867=CARTESIAN_POINT('Ctrl Pts',(-0.0701433255283678,0.120018824057881,
0.4341455384304));
#34868=CARTESIAN_POINT('Ctrl Pts',(-0.117063601095489,0.0426502166584235,
0.439544603844645));
#34869=CARTESIAN_POINT('Ctrl Pts',(-0.117959555656036,0.00192608038356173,
0.442308328192384));
#34870=CARTESIAN_POINT('Ctrl Pts',(-0.117952286276812,3.39956489144155E-5,
0.442436711473616));
#34871=CARTESIAN_POINT('Origin',(0.,0.,-0.0924367114736152));
#34872=CARTESIAN_POINT('',(-0.117920926539219,6.26243704048756E-5,0.332563288526384));
#34873=CARTESIAN_POINT('',(-0.117615878293784,5.9477676878486E-5,0.342436711473616));
#34874=CARTESIAN_POINT('',(-0.117775,-1.30487598617993E-14,-0.0924367114736152));
#34875=CARTESIAN_POINT('Ctrl Pts',(-0.117920926539219,6.26243704048737E-5,
0.332563288526384));
#34876=CARTESIAN_POINT('Ctrl Pts',(-0.117693603628949,-0.0350666637837455,
0.334945229074087));
#34877=CARTESIAN_POINT('Ctrl Pts',(-0.0824632530796663,-0.109429893167014,
0.339960573576592));
#34878=CARTESIAN_POINT('Ctrl Pts',(0.0437107063235388,-0.131926077644361,
0.347609322033898));
#34879=CARTESIAN_POINT('Ctrl Pts',(0.134376016486386,-0.0354711432460098,
0.355509533898305));
#34880=CARTESIAN_POINT('Ctrl Pts',(0.103127892463174,0.0931651952503325,
0.363409745762711));
#34881=CARTESIAN_POINT('Ctrl Pts',(-0.0216836207666979,0.137276860396698,
0.371309957627119));
#34882=CARTESIAN_POINT('Ctrl Pts',(-0.106651080731,0.0722748925449633,0.377694471881676));
#34883=CARTESIAN_POINT('Ctrl Pts',(-0.117662370625513,0.0166442803494234,
0.381445582181431));
#34884=CARTESIAN_POINT('Ctrl Pts',(-0.117603494801586,4.59807059966007E-5,
0.382563288526384));
#34885=CARTESIAN_POINT('Ctrl Pts',(-0.117615878293784,5.94776768784704E-5,
0.342436711473616));
#34886=CARTESIAN_POINT('Ctrl Pts',(-0.11750760701874,-0.0234105356203755,
0.344017568727647));
#34887=CARTESIAN_POINT('Ctrl Pts',(-0.0993568477409689,-0.0861600913990265,
0.348233767048184));
#34888=CARTESIAN_POINT('Ctrl Pts',(0.00259563734382704,-0.138988729439456,
0.355085306435226));
#34889=CARTESIAN_POINT('Ctrl Pts',(0.117881001348277,-0.0736795342380946,
0.362991329634744));
#34890=CARTESIAN_POINT('Ctrl Pts',(0.12607389627645,0.0585660048329233,
0.370897352834261));
#34891=CARTESIAN_POINT('Ctrl Pts',(0.0197312453245754,0.137605531147394,
0.378803376033779));
#34892=CARTESIAN_POINT('Ctrl Pts',(-0.0931217327741457,0.0958562111818821,
0.385983162246897));
#34893=CARTESIAN_POINT('Ctrl Pts',(-0.117484499455465,0.0281732773148422,
0.39052760739351));
#34894=CARTESIAN_POINT('Ctrl Pts',(-0.117726185906756,-0.000103034036682944,
0.392436711473616));
#34895=CARTESIAN_POINT('Origin',(0.,0.,-0.0924367114736152));
#34896=CARTESIAN_POINT('',(-0.117774170260593,-0.000104886777209015,0.282563288526384));
#34897=CARTESIAN_POINT('',(-0.11793628481875,5.1384428605368E-5,0.292436711473616));
#34898=CARTESIAN_POINT('',(-0.117775,-1.30487598617993E-14,-0.0924367114736152));
#34899=CARTESIAN_POINT('Ctrl Pts',(-0.117774170260593,-0.00010488677720901,
0.282563288526384));
#34900=CARTESIAN_POINT('Ctrl Pts',(-0.117856360533384,-0.0092011162257308,
0.283178068057138));
#34901=CARTESIAN_POINT('Ctrl Pts',(-0.112752995425492,-0.057169777637724,
0.286426251542693));
#34902=CARTESIAN_POINT('Ctrl Pts',(-0.0471669369944997,-0.130730240818604,
0.292307838983051));
#34903=CARTESIAN_POINT('Ctrl Pts',(0.0837214480778729,-0.110931667893667,
0.300208050847457));
#34904=CARTESIAN_POINT('Ctrl Pts',(0.138653055169421,0.00951031556331505,
0.308108262711865));
#34905=CARTESIAN_POINT('Ctrl Pts',(0.0677908594821406,0.121324009085596,
0.316008474576271));
#34906=CARTESIAN_POINT('Ctrl Pts',(-0.0645749936433688,0.123065779182871,
0.323908686440678));
#34907=CARTESIAN_POINT('Ctrl Pts',(-0.116109941121323,0.0462937466385656,
0.329426957757382));
#34908=CARTESIAN_POINT('Ctrl Pts',(-0.117944925204334,0.00377125198361699,
0.332311825119284));
#34909=CARTESIAN_POINT('Ctrl Pts',(-0.117920926539219,6.26243704048737E-5,
0.332563288526384));
#34910=CARTESIAN_POINT('Ctrl Pts',(-0.11793628481875,5.13844286053676E-5,
0.292436711473616));
#34911=CARTESIAN_POINT('Ctrl Pts',(-0.117738942084994,-0.0358551097426003,
0.294872188995279));
#34912=CARTESIAN_POINT('Ctrl Pts',(-0.0811119992076199,-0.110963296543085,
0.299943007583447));
#34913=CARTESIAN_POINT('Ctrl Pts',(0.046471358419155,-0.131015331511595,
0.307649167238122));
#34914=CARTESIAN_POINT('Ctrl Pts',(0.135145386671506,-0.0325626888604762,
0.315555190437639));
#34915=CARTESIAN_POINT('Ctrl Pts',(0.101042606300054,0.0954724879559945,
0.323461213637157));
#34916=CARTESIAN_POINT('Ctrl Pts',(-0.0248553070174182,0.136772869961425,
0.331367236836674));
#34917=CARTESIAN_POINT('Ctrl Pts',(-0.107513748550757,0.0704052555566997,
0.33769240278216));
#34918=CARTESIAN_POINT('Ctrl Pts',(-0.117688098797311,0.0157147489149463,
0.341382227661141));
#34919=CARTESIAN_POINT('Ctrl Pts',(-0.117615878293784,5.94776768784704E-5,
0.342436711473616));
#34920=CARTESIAN_POINT('Origin',(0.,0.,-0.0924367114736152));
#34921=CARTESIAN_POINT('',(-0.117597921122191,3.83764452643825E-5,0.232563288526384));
#34922=CARTESIAN_POINT('',(-0.117756807889117,-0.000105309437279225,0.242436711473616));
#34923=CARTESIAN_POINT('',(-0.117775,-1.30487598617993E-14,-0.0924367114736152));
#34924=CARTESIAN_POINT('Ctrl Pts',(-0.117597921122191,3.83764452643858E-5,
0.232563288526384));
#34925=CARTESIAN_POINT('Ctrl Pts',(-0.117532990113526,-0.0219578937617309,
0.234044310994991));
#34926=CARTESIAN_POINT('Ctrl Pts',(-0.101078828998682,-0.0831558954107903,
0.238158737418399));
#34927=CARTESIAN_POINT('Ctrl Pts',(-0.00273688716624997,-0.138951881091211,
0.24490656779661));
#34928=CARTESIAN_POINT('Ctrl Pts',(0.114882759277182,-0.0782116834669906,
0.252806779661017));
#34929=CARTESIAN_POINT('Ctrl Pts',(0.128274344207101,0.0534865256689417,
0.260706991525423));
#34930=CARTESIAN_POINT('Ctrl Pts',(0.0252882731449639,0.136658768658679,
0.26860720338983));
#34931=CARTESIAN_POINT('Ctrl Pts',(-0.090841176153826,0.099022467675047,
0.275892635723484));
#34932=CARTESIAN_POINT('Ctrl Pts',(-0.117504299056729,0.0297625209893518,
0.280544664102335));
#34933=CARTESIAN_POINT('Ctrl Pts',(-0.117774170260593,-0.00010488677720901,
0.282563288526384));
#34934=CARTESIAN_POINT('Ctrl Pts',(-0.117756807889117,-0.000105309437279212,
0.242436711473616));
#34935=CARTESIAN_POINT('Ctrl Pts',(-0.117843399042527,-0.00979668321532341,
0.243091468196405));
#34936=CARTESIAN_POINT('Ctrl Pts',(-0.112329964982903,-0.058397845463228,
0.246381565985699));
#34937=CARTESIAN_POINT('Ctrl Pts',(-0.0451064993838265,-0.131491474848312,
0.252307004841499));
#34938=CARTESIAN_POINT('Ctrl Pts',(0.0855648107118161,-0.1095594241143,
0.260213028041017));
#34939=CARTESIAN_POINT('Ctrl Pts',(0.138502247321704,0.0119051136596435,
0.268119051240535));
#34940=CARTESIAN_POINT('Ctrl Pts',(0.0656132363391791,0.122554100141606,
0.276025074440052));
#34941=CARTESIAN_POINT('Ctrl Pts',(-0.066884052510702,0.121865203254083,
0.283931097639569));
#34942=CARTESIAN_POINT('Ctrl Pts',(-0.1165204945288,0.0447817101515102,
0.289401643317424));
#34943=CARTESIAN_POINT('Ctrl Pts',(-0.117952479432728,0.00299799310969985,
0.292236847928773));
#34944=CARTESIAN_POINT('Ctrl Pts',(-0.11793628481875,5.13844286053676E-5,
0.292436711473616));
#34945=CARTESIAN_POINT('Origin',(0.,0.,-0.0924367114736152));
#34946=CARTESIAN_POINT('',(-0.117909687164366,6.9664588846411E-5,0.182563288526384));
#34947=CARTESIAN_POINT('',(-0.117601649275994,4.45452448404882E-5,0.192436711473616));
#34948=CARTESIAN_POINT('',(-0.117775,-1.30487598617993E-14,-0.0924367114736152));
#34949=CARTESIAN_POINT('Ctrl Pts',(-0.117909687164366,6.96645888464118E-5,
0.182563288526384));
#34950=CARTESIAN_POINT('Ctrl Pts',(-0.11766595726848,-0.0345569219122136,
0.184910553932844));
#34951=CARTESIAN_POINT('Ctrl Pts',(-0.0833160382623138,-0.10845204978507,
0.189891223294105));
#34952=CARTESIAN_POINT('Ctrl Pts',(0.0419824540321544,-0.132486185591528,
0.197505296610169));
#34953=CARTESIAN_POINT('Ctrl Pts',(0.133900861976353,-0.0372246554226585,
0.205405508474576));
#34954=CARTESIAN_POINT('Ctrl Pts',(0.10433692245731,0.0918091630494651,
0.213305720338983));
#34955=CARTESIAN_POINT('Ctrl Pts',(-0.0198873058616059,0.137548576426424,
0.221205932203389));
#34956=CARTESIAN_POINT('Ctrl Pts',(-0.10616324692175,0.0733158722115256,
0.22762512159919));
#34957=CARTESIAN_POINT('Ctrl Pts',(-0.117648443848114,0.0171536431540524,
0.231410907040188));
#34958=CARTESIAN_POINT('Ctrl Pts',(-0.117597921122191,3.83764452643858E-5,
0.232563288526384));
#34959=CARTESIAN_POINT('Ctrl Pts',(-0.117601649275994,4.45452448404882E-5,
0.192436711473616));
#34960=CARTESIAN_POINT('Ctrl Pts',(-0.11752478280801,-0.0223710360060294,
0.193946088464036));
#34961=CARTESIAN_POINT('Ctrl Pts',(-0.100593880386987,-0.0840313287987434,
0.198090806520963));
#34962=CARTESIAN_POINT('Ctrl Pts',(-0.00115024004832317,-0.139008205490464,
0.204870865644395));
#34963=CARTESIAN_POINT('Ctrl Pts',(0.115852970087698,-0.0768289890996742,
0.212776888843912));
#34964=CARTESIAN_POINT('Ctrl Pts',(0.127606135899372,0.055147786219953,
0.22068291204343));
#34965=CARTESIAN_POINT('Ctrl Pts',(0.0234317475993789,0.137023930205902,
0.228588935242947));
#34966=CARTESIAN_POINT('Ctrl Pts',(-0.0916394876575414,0.0979452740831826,
0.235840201719676));
#34967=CARTESIAN_POINT('Ctrl Pts',(-0.11749487688974,0.0292102859676066,
0.240456127129899));
#34968=CARTESIAN_POINT('Ctrl Pts',(-0.117756807889117,-0.000105309437279212,
0.242436711473616));
#34969=CARTESIAN_POINT('Origin',(0.,0.,-0.0924367114736152));
#34970=CARTESIAN_POINT('',(-0.117789487689835,-0.000104112672946744,0.132563288526384));
#34971=CARTESIAN_POINT('',(-0.117915129103549,6.69430946510577E-5,0.142436711473616));
#34972=CARTESIAN_POINT('',(-0.117775,-1.30487598617993E-14,-0.0924367114736152));
#34973=CARTESIAN_POINT('Ctrl Pts',(-0.117789487689835,-0.000104112672946739,
0.132563288526384));
#34974=CARTESIAN_POINT('Ctrl Pts',(-0.117867447370286,-0.00868443076951223,
0.133143392915894));
#34975=CARTESIAN_POINT('Ctrl Pts',(-0.113109713752316,-0.056129702894726,
0.136356901260207));
#34976=CARTESIAN_POINT('Ctrl Pts',(-0.0488717923313075,-0.130102508888041,
0.142203813559322));
#34977=CARTESIAN_POINT('Ctrl Pts',(0.0822642127117346,-0.112016585630158,
0.150104025423729));
#34978=CARTESIAN_POINT('Ctrl Pts',(0.138765526166673,0.00769705224861128,
0.158004237288135));
#34979=CARTESIAN_POINT('Ctrl Pts',(0.0693709963376258,0.12042749084372,
0.165904449152542));
#34980=CARTESIAN_POINT('Ctrl Pts',(-0.0629607791409001,0.123899379163224,
0.173804661016949));
#34981=CARTESIAN_POINT('Ctrl Pts',(-0.115824984153554,0.0473294249038356,
0.179357607474896));
#34982=CARTESIAN_POINT('Ctrl Pts',(-0.117939398554652,0.00429074720192216,
0.182277149978042));
#34983=CARTESIAN_POINT('Ctrl Pts',(-0.117909687164366,6.96645888464118E-5,
0.182563288526384));
#34984=CARTESIAN_POINT('Ctrl Pts',(-0.117915129103549,6.69430946510529E-5,
0.142436711473616));
#34985=CARTESIAN_POINT('Ctrl Pts',(-0.117677363460081,-0.0348022339441635,
0.144800708731668));
#34986=CARTESIAN_POINT('Ctrl Pts',(-0.0828943760199795,-0.108955331093341,
0.149800047056226));
#34987=CARTESIAN_POINT('Ctrl Pts',(0.0429243879661372,-0.132219897211806,
0.15743472644729));
#34988=CARTESIAN_POINT('Ctrl Pts',(0.134218946443888,-0.0361922458912883,
0.165340749646808));
#34989=CARTESIAN_POINT('Ctrl Pts',(0.103578348063976,0.0927153171784346,
0.173246772846325));
#34990=CARTESIAN_POINT('Ctrl Pts',(-0.0211610525014389,0.137392918706172,
0.181152796045843));
#34991=CARTESIAN_POINT('Ctrl Pts',(-0.106531690673769,0.0725519877028229,
0.187549442254939));
#34992=CARTESIAN_POINT('Ctrl Pts',(-0.117658990074321,0.0167661061227608,
0.19131074739753));
#34993=CARTESIAN_POINT('Ctrl Pts',(-0.117601649275994,4.45452448404882E-5,
0.192436711473616));
#34994=CARTESIAN_POINT('Origin',(0.,0.,-0.0924367114736152));
#34995=CARTESIAN_POINT('',(-0.117593357284741,3.06645980543279E-5,0.0825632885263843));
#34996=CARTESIAN_POINT('',(-0.117788324723582,-0.000104604007662518,0.0924367114736157));
#34997=CARTESIAN_POINT('',(-0.117775,-1.30487598617993E-14,-0.0924367114736152));
#34998=CARTESIAN_POINT('Ctrl Pts',(-0.117593357284741,3.06645980543228E-5,
0.0825632885263843));
#34999=CARTESIAN_POINT('Ctrl Pts',(-0.11754301899516,-0.021452746571923,
0.0840096358537477));
#35000=CARTESIAN_POINT('Ctrl Pts',(-0.101655671713158,-0.0821210291969121,
0.0880893871359134));
#35001=CARTESIAN_POINT('Ctrl Pts',(-0.0045529857407016,-0.138904079109577,
0.0948025423728811));
#35002=CARTESIAN_POINT('Ctrl Pts',(0.113850559027731,-0.0797068119457511,
0.102702754237288));
#35003=CARTESIAN_POINT('Ctrl Pts',(0.12896255920279,0.0518052156568057,
0.110602966101695));
#35004=CARTESIAN_POINT('Ctrl Pts',(0.0270724914422277,0.136316505597261,
0.118503177966102));
#35005=CARTESIAN_POINT('Ctrl Pts',(-0.0900940209439092,0.100029588267392,
0.125823285440998));
#35006=CARTESIAN_POINT('Ctrl Pts',(-0.117513546702531,0.0302662202125134,
0.130509988961092));
#35007=CARTESIAN_POINT('Ctrl Pts',(-0.117789487689835,-0.000104112672946739,
0.132563288526384));
#35008=CARTESIAN_POINT('Ctrl Pts',(-0.117788324723582,-0.00010460400766255,
0.0924367114736157));
#35009=CARTESIAN_POINT('Ctrl Pts',(-0.117866887107117,-0.00873205619380746,
0.093019987932794));
#35010=CARTESIAN_POINT('Ctrl Pts',(-0.113075788730874,-0.0562533105277103,
0.0962386054584782));
#35011=CARTESIAN_POINT('Ctrl Pts',(-0.0486330432543111,-0.130228357167641,
0.102092564050668));
#35012=CARTESIAN_POINT('Ctrl Pts',(0.0825817545836372,-0.111825131042891,
0.109998587250186));
#35013=CARTESIAN_POINT('Ctrl Pts',(0.138772738128538,0.00816897019039422,
0.117904610449703));
#35014=CARTESIAN_POINT('Ctrl Pts',(0.0688915313895657,0.120741708772585,
0.12581063364922));
#35015=CARTESIAN_POINT('Ctrl Pts',(-0.0635762130827019,0.123623095373164,
0.133716656848738));
#35016=CARTESIAN_POINT('Ctrl Pts',(-0.115947056638979,0.0469156369390546,
0.139258682790203));
#35017=CARTESIAN_POINT('Ctrl Pts',(-0.117942420266852,0.00406928923237253,
0.142165367665162));
#35018=CARTESIAN_POINT('Ctrl Pts',(-0.117915129103549,6.69430946510529E-5,
0.142436711473616));
#35019=CARTESIAN_POINT('Origin',(0.,0.,-0.0924367114736152));
#35020=CARTESIAN_POINT('',(-0.117896184020664,8.43438525025023E-5,0.0325632885263842));
#35021=CARTESIAN_POINT('',(-0.117591431864639,2.92794590778037E-5,0.0424367114736158));
#35022=CARTESIAN_POINT('',(-0.117775,-1.30487598617993E-14,-0.0924367114736152));
#35023=CARTESIAN_POINT('Ctrl Pts',(-0.117896184020664,8.43438525024954E-5,
0.0325632885263842));
#35024=CARTESIAN_POINT('Ctrl Pts',(-0.117638881596538,-0.0340384192378303,
0.0348758787916007));
#35025=CARTESIAN_POINT('Ctrl Pts',(-0.0841595758608773,-0.107483448399194,
0.0398218730116195));
#35026=CARTESIAN_POINT('Ctrl Pts',(0.040248222246223,-0.133016439153077,
0.0474012711864405));
#35027=CARTESIAN_POINT('Ctrl Pts',(0.133402197487182,-0.0389756054074351,
0.0553014830508473));
#35028=CARTESIAN_POINT('Ctrl Pts',(0.105528454455023,0.0904394425945055,
0.0632016949152541));
#35029=CARTESIAN_POINT('Ctrl Pts',(-0.0180877669633101,0.137795734956694,
0.0711019067796609));
#35030=CARTESIAN_POINT('Ctrl Pts',(-0.105666299933038,0.0743567679416689,
0.0775557713167041));
#35031=CARTESIAN_POINT('Ctrl Pts',(-0.117634671289428,0.017662685017247,
0.0813762318989454));
#35032=CARTESIAN_POINT('Ctrl Pts',(-0.117593357284741,3.06645980543228E-5,
0.0825632885263843));
#35033=CARTESIAN_POINT('Ctrl Pts',(-0.117591431864639,2.92794590778002E-5,
0.0424367114736158));
#35034=CARTESIAN_POINT('Ctrl Pts',(-0.11754501123181,-0.0213296840770181,
0.0438746082004259));
#35035=CARTESIAN_POINT('Ctrl Pts',(-0.101789620521557,-0.0818995216066154,
0.0479478459937417));
#35036=CARTESIAN_POINT('Ctrl Pts',(-0.00489492837772915,-0.138925734589418,
0.0546564248535634));
#35037=CARTESIAN_POINT('Ctrl Pts',(0.113740629398734,-0.0799231888543136,
0.062562448053081));
#35038=CARTESIAN_POINT('Ctrl Pts',(0.129045816271948,0.0516898037714297,
0.0704684712525983));
#35039=CARTESIAN_POINT('Ctrl Pts',(0.0271151839788463,0.136342686033388,
0.0783744944521158));
#35040=CARTESIAN_POINT('Ctrl Pts',(-0.0901114389347958,0.100024405106452,
0.0856972411924549));
#35041=CARTESIAN_POINT('Ctrl Pts',(-0.117511929055312,0.0302482226905713,
0.0903846468662882));
#35042=CARTESIAN_POINT('Ctrl Pts',(-0.117788324723582,-0.00010460400766255,
0.0924367114736157));
#35043=CARTESIAN_POINT('Origin',(0.,0.,0.95));
#35044=CARTESIAN_POINT('',(-0.143203996033626,-2.30855198111598E-5,0.907000235762439));
#35045=CARTESIAN_POINT('Ctrl Pts',(-0.0334019664626807,0.112939183906322,
0.932225));
#35046=CARTESIAN_POINT('Ctrl Pts',(-0.0250603177854857,0.115799805022824,
0.931847596094215));
#35047=CARTESIAN_POINT('Ctrl Pts',(-0.0164278988467134,0.117636476238285,
0.931473565046676));
#35048=CARTESIAN_POINT('Ctrl Pts',(-0.00767106646971057,0.118512486061759,
0.931100514589335));
#35049=CARTESIAN_POINT('Ctrl Pts',(-0.00420439075546036,0.118859282922739,
0.930952830483373));
#35050=CARTESIAN_POINT('Ctrl Pts',(-0.000716143526927236,0.119054988716296,
0.930805221836912));
#35051=CARTESIAN_POINT('Ctrl Pts',(0.00277797710115842,0.119101360153194,
0.930657787404542));
#35052=CARTESIAN_POINT('Ctrl Pts',(0.00969984845123832,0.119193222213692,
0.930365719018224));
#35053=CARTESIAN_POINT('Ctrl Pts',(0.0166142532722655,0.118700388967513,
0.930075608100973));
#35054=CARTESIAN_POINT('Ctrl Pts',(0.02344427759502,0.117646722051856,0.929786344238933));
#35055=CARTESIAN_POINT('Ctrl Pts',(0.0272709497102665,0.117056381869396,
0.929624277765593));
#35056=CARTESIAN_POINT('Ctrl Pts',(0.0310712076772195,0.116289673696229,
0.929462477186978));
#35057=CARTESIAN_POINT('Ctrl Pts',(0.0348314922052066,0.115348424870015,
0.929300747212246));
#35058=CARTESIAN_POINT('Ctrl Pts',(0.0378910930422447,0.114582566415658,
0.929169153668624));
#35059=CARTESIAN_POINT('Ctrl Pts',(0.04092399616764,0.113700812218856,0.929037612549819));
#35060=CARTESIAN_POINT('Ctrl Pts',(0.0439095212807944,0.11270886835725,
0.928906608402292));
#35061=CARTESIAN_POINT('Ctrl Pts',(0.0525514734098646,0.10983757066528,
0.928527401553001));
#35062=CARTESIAN_POINT('Ctrl Pts',(0.0608263773706973,0.106040058117234,
0.928151455604188));
#35063=CARTESIAN_POINT('Ctrl Pts',(0.0685605494008651,0.101344813008116,
0.927776330408337));
#35064=CARTESIAN_POINT('Ctrl Pts',(0.072435687838791,0.0989923020054058,
0.927588377249316));
#35065=CARTESIAN_POINT('Ctrl Pts',(0.0761749070710193,0.0964136602636579,
0.92740063013395));
#35066=CARTESIAN_POINT('Ctrl Pts',(0.0797540201577765,0.0936080366646606,
0.927212782134414));
#35067=CARTESIAN_POINT('Ctrl Pts',(0.0820668650566089,0.091795025432075,
0.927091393601291));
#35068=CARTESIAN_POINT('Ctrl Pts',(0.0843049421929101,0.089893314502136,
0.926970374334797));
#35069=CARTESIAN_POINT('Ctrl Pts',(0.0864667806566824,0.087910346105634,
0.926849671848167));
#35070=CARTESIAN_POINT('Ctrl Pts',(0.0931618700565369,0.0817692070177022,
0.9264758631884));
#35071=CARTESIAN_POINT('Ctrl Pts',(0.0991298287989589,0.0748505421836024,
0.926105008552812));
#35072=CARTESIAN_POINT('Ctrl Pts',(0.104322127839002,0.0673319773813505,
0.925734762248716));
#35073=CARTESIAN_POINT('Ctrl Pts',(0.106370940812892,0.0643652505050492,
0.925588667922192));
#35074=CARTESIAN_POINT('Ctrl Pts',(0.108298617033319,0.0613046783141235,
0.925442668312145));
#35075=CARTESIAN_POINT('Ctrl Pts',(0.110100560923862,0.0581597986785966,
0.925296619306966));
#35076=CARTESIAN_POINT('Ctrl Pts',(0.11158855048605,0.0555628542917283,
0.925176016553231));
#35077=CARTESIAN_POINT('Ctrl Pts',(0.112988026000293,0.0529128751968171,
0.925055591079489));
#35078=CARTESIAN_POINT('Ctrl Pts',(0.114293875604956,0.0502227205878152,
0.92493557115538));
#35079=CARTESIAN_POINT('Ctrl Pts',(0.118434599880109,0.0416924974643938,
0.924554999448279));
#35080=CARTESIAN_POINT('Ctrl Pts',(0.121649070098747,0.0327401005258095,
0.924177564198185));
#35081=CARTESIAN_POINT('Ctrl Pts',(0.123868271499824,0.0235442585075687,
0.923800796649243));
#35082=CARTESIAN_POINT('Ctrl Pts',(0.124741985203477,0.0199237970280188,
0.923652460869335));
#35083=CARTESIAN_POINT('Ctrl Pts',(0.125460929083487,0.0162653271532848,
0.923504228586243));
#35084=CARTESIAN_POINT('Ctrl Pts',(0.126018750659753,0.0125790928555092,
0.923355949140843));
#35085=CARTESIAN_POINT('Ctrl Pts',(0.126424880564737,0.00989527772751904,
0.923247992188954));
#35086=CARTESIAN_POINT('Ctrl Pts',(0.126745061646254,0.00719882962072188,
0.923140094926841));
#35087=CARTESIAN_POINT('Ctrl Pts',(0.126976603796028,0.00450277675306522,
0.923032557085152));
#35088=CARTESIAN_POINT('Ctrl Pts',(0.12757677314312,-0.00248553311139155,
0.922753813382129));
#35089=CARTESIAN_POINT('Ctrl Pts',(0.127585234929588,-0.00948784607823892,
0.922476804764986));
#35090=CARTESIAN_POINT('Ctrl Pts',(0.126969800827767,-0.0164342950540157,
0.922200564268829));
#35091=CARTESIAN_POINT('Ctrl Pts',(0.126365890166078,-0.0232506781321251,
0.921929496123068));
#35092=CARTESIAN_POINT('Ctrl Pts',(0.125161228392162,-0.0300136540166471,
0.921659167602865));
#35093=CARTESIAN_POINT('Ctrl Pts',(0.123399407242885,-0.0366692095497128,
0.921388665049245));
#35094=CARTESIAN_POINT('Ctrl Pts',(0.122693706044386,-0.0393351064361743,
0.921280314677605));
#35095=CARTESIAN_POINT('Ctrl Pts',(0.121898903213358,-0.0419812756064514,
0.921172034233936));
#35096=CARTESIAN_POINT('Ctrl Pts',(0.121020997998916,-0.0445959600773696,
0.921064109665588));
#35097=CARTESIAN_POINT('Ctrl Pts',(0.118352374694664,-0.0525439797468811,
0.920736044615448));
#35098=CARTESIAN_POINT('Ctrl Pts',(0.11491247387436,-0.0602240203343106,
0.920410355973602));
#35099=CARTESIAN_POINT('Ctrl Pts',(0.110787244183297,-0.067540847099726,
0.920085467703143));
#35100=CARTESIAN_POINT('Ctrl Pts',(0.108602638591366,-0.0714156327150692,
0.919913416014983));
#35101=CARTESIAN_POINT('Ctrl Pts',(0.106225299026755,-0.0751884756223749,
0.919741588788067));
#35102=CARTESIAN_POINT('Ctrl Pts',(0.103664831029184,-0.0788439383503402,
0.919569751954905));
#35103=CARTESIAN_POINT('Ctrl Pts',(0.101376332819864,-0.0821111222851215,
0.919416167420609));
#35104=CARTESIAN_POINT('Ctrl Pts',(0.0989387376213173,-0.0852871325232165,
0.919262431231772));
#35105=CARTESIAN_POINT('Ctrl Pts',(0.0963759957044455,-0.088340202919688,
0.919109404658397));
#35106=CARTESIAN_POINT('Ctrl Pts',(0.0909694481938422,-0.0947811832006395,
0.918786568623332));
#35107=CARTESIAN_POINT('Ctrl Pts',(0.0849957607581912,-0.100695240401247,
0.918466028662098));
#35108=CARTESIAN_POINT('Ctrl Pts',(0.0785257616471073,-0.105984325129946,
0.918146284163942));
#35109=CARTESIAN_POINT('Ctrl Pts',(0.0742361136603187,-0.109491019840235,
0.917934291655249));
#35110=CARTESIAN_POINT('Ctrl Pts',(0.0697277556719998,-0.112722769515888,
0.917722648813756));
#35111=CARTESIAN_POINT('Ctrl Pts',(0.0650165017469215,-0.115645838880061,
0.917510918298299));
#35112=CARTESIAN_POINT('Ctrl Pts',(0.0626218558869296,-0.117131582604068,
0.917403299475299));
#35113=CARTESIAN_POINT('Ctrl Pts',(0.0601741524651638,-0.118537526250906,
0.917295638036625));
#35114=CARTESIAN_POINT('Ctrl Pts',(0.0576864529767728,-0.119853555264988,
0.917188346403244));
#35115=CARTESIAN_POINT('Ctrl Pts',(0.0492417976832846,-0.12432090006769,
0.916824138079852));
#35116=CARTESIAN_POINT('Ctrl Pts',(0.0403105010214407,-0.127774185485052,
0.916462909477301));
#35117=CARTESIAN_POINT('Ctrl Pts',(0.0310751541446225,-0.130251129571305,
0.916102510949096));
#35118=CARTESIAN_POINT('Ctrl Pts',(0.0264632552530831,-0.131488052865922,
0.91592253702988));
#35119=CARTESIAN_POINT('Ctrl Pts',(0.0217750625284288,-0.132480793424065,
0.915742770110557));
#35120=CARTESIAN_POINT('Ctrl Pts',(0.0170316000051624,-0.133229777506063,
0.915562942492132));
#35121=CARTESIAN_POINT('Ctrl Pts',(0.0138158762359995,-0.133737534424853,
0.91544103240133));
#35122=CARTESIAN_POINT('Ctrl Pts',(0.0105740209053218,-0.134132938348625,
0.915319069467609));
#35123=CARTESIAN_POINT('Ctrl Pts',(0.0073287749381158,-0.134414943979412,
0.91519757274014));
#35124=CARTESIAN_POINT('Ctrl Pts',(-0.00265707911089655,-0.135282695483764,
0.91482371861623));
#35125=CARTESIAN_POINT('Ctrl Pts',(-0.0127097596984602,-0.135087239355917,
0.914452927180717));
#35126=CARTESIAN_POINT('Ctrl Pts',(-0.0226366995613315,-0.13384562451132,
0.914082871556714));
#35127=CARTESIAN_POINT('Ctrl Pts',(-0.0278509024051071,-0.133193456598246,
0.913888496944428));
#35128=CARTESIAN_POINT('Ctrl Pts',(-0.0330306231776361,-0.132251796770583,
0.913694325339435));
#35129=CARTESIAN_POINT('Ctrl Pts',(-0.0381476304341873,-0.131017345860063,
0.913500019539069));
#35130=CARTESIAN_POINT('Ctrl Pts',(-0.0414017963667409,-0.130232295556825,
0.913376450569093));
#35131=CARTESIAN_POINT('Ctrl Pts',(-0.0446227244193663,-0.129330489295675,
0.913253123242388));
#35132=CARTESIAN_POINT('Ctrl Pts',(-0.0477977620148837,-0.128314174106561,
0.913130170982833));
#35133=CARTESIAN_POINT('Ctrl Pts',(-0.0560508514351662,-0.125672397471604,
0.912810572879819));
#35134=CARTESIAN_POINT('Ctrl Pts',(-0.0640066574241223,-0.122256042832264,
0.912493045231938));
#35135=CARTESIAN_POINT('Ctrl Pts',(-0.0715409466919047,-0.118061015146759,
0.912176128537659));
#35136=CARTESIAN_POINT('Ctrl Pts',(-0.0762921378140006,-0.11541559265395,
0.911976277996913));
#35137=CARTESIAN_POINT('Ctrl Pts',(-0.080875618778813,-0.112459902541578,
0.911776670412738));
#35138=CARTESIAN_POINT('Ctrl Pts',(-0.0852772318261866,-0.109220115387155,
0.911576939781678));
#35139=CARTESIAN_POINT('Ctrl Pts',(-0.0875530243079477,-0.107545028738423,
0.911473671851569));
#35140=CARTESIAN_POINT('Ctrl Pts',(-0.0897785308463731,-0.105794887026521,
0.911370439409319));
#35141=CARTESIAN_POINT('Ctrl Pts',(-0.0919449058640415,-0.10397965349885,
0.911267529872683));
#35142=CARTESIAN_POINT('Ctrl Pts',(-0.0992562147283688,-0.0978534136403538,
0.910920220011141));
#35143=CARTESIAN_POINT('Ctrl Pts',(-0.105919754790705,-0.0909713378622389,
0.910575510440108));
#35144=CARTESIAN_POINT('Ctrl Pts',(-0.111868517901189,-0.0834835697610656,
0.910231536759666));
#35145=CARTESIAN_POINT('Ctrl Pts',(-0.115372944257836,-0.0790725129751651,
0.910028901285812));
#35146=CARTESIAN_POINT('Ctrl Pts',(-0.118628912335923,-0.0744505089078481,
0.909826521196012));
#35147=CARTESIAN_POINT('Ctrl Pts',(-0.121618006629831,-0.0696436476859399,
0.90962401532803));
#35148=CARTESIAN_POINT('Ctrl Pts',(-0.123117391998195,-0.0672324365713985,
0.90952243461307));
#35149=CARTESIAN_POINT('Ctrl Pts',(-0.124548834320201,-0.0647754742963825,
0.909420860177745));
#35150=CARTESIAN_POINT('Ctrl Pts',(-0.125905418138961,-0.0622851116177192,
0.9093196043405));
#35151=CARTESIAN_POINT('Ctrl Pts',(-0.130761030150815,-0.0533713719953201,
0.908957179953008));
#35152=CARTESIAN_POINT('Ctrl Pts',(-0.134679363933253,-0.0440025983801541,
0.908597596571227));
#35153=CARTESIAN_POINT('Ctrl Pts',(-0.13756687326497,-0.0343371686472044,
0.908238737834252));
#35154=CARTESIAN_POINT('Ctrl Pts',(-0.139097796244526,-0.0292126731787653,
0.908048475215596));
#35155=CARTESIAN_POINT('Ctrl Pts',(-0.14033830847868,-0.0240043037722782,
0.907858416294146));
#35156=CARTESIAN_POINT('Ctrl Pts',(-0.14126916593033,-0.0187337321988357,
0.90766824565692));
#35157=CARTESIAN_POINT('Ctrl Pts',(-0.141766581419635,-0.0159173354095375,
0.907566625564177));
#35158=CARTESIAN_POINT('Ctrl Pts',(-0.142175147764435,-0.0130838950804596,
0.90746500095103));
#35159=CARTESIAN_POINT('Ctrl Pts',(-0.142491067194012,-0.010247236235083,
0.907363696319434));
#35160=CARTESIAN_POINT('Ctrl Pts',(-0.142699030773042,-0.00837991922086784,
0.907297009462638));
#35161=CARTESIAN_POINT('Ctrl Pts',(-0.142867069971313,-0.00651002641398622,
0.907230418639425));
#35162=CARTESIAN_POINT('Ctrl Pts',(-0.142994592382579,-0.00463854690639179,
0.907163910672075));
#35163=CARTESIAN_POINT('Ctrl Pts',(-0.143099304951117,-0.00310181760319464,
0.907109298937397));
#35164=CARTESIAN_POINT('Ctrl Pts',(-0.143176698406437,-0.00156401794929073,
0.907054743068754));
#35165=CARTESIAN_POINT('Ctrl Pts',(-0.143227225569541,-2.57112916194508E-5,
0.907000235770274));
#35166=CARTESIAN_POINT('',(-0.00156150813732516,0.146115848505824,0.90365));
#35167=CARTESIAN_POINT('Ctrl Pts',(-0.00156268643911937,0.146080787864432,
0.90365));
#35168=CARTESIAN_POINT('Ctrl Pts',(-0.0117053345256504,0.14465327094795,
0.904950888122905));
#35169=CARTESIAN_POINT('Ctrl Pts',(-0.0216455209286645,0.142222180286059,
0.906261527257655));
#35170=CARTESIAN_POINT('Ctrl Pts',(-0.0312038210265984,0.138800205489803,
0.907591018110418));
#35171=CARTESIAN_POINT('Ctrl Pts',(-0.0379790896742497,0.136374586047791,
0.908533409288742));
#35172=CARTESIAN_POINT('Ctrl Pts',(-0.0445622616029078,0.133450051590279,
0.909485272488055));
#35173=CARTESIAN_POINT('Ctrl Pts',(-0.0508780053273359,0.130018961446113,
0.910449848959387));
#35174=CARTESIAN_POINT('Ctrl Pts',(-0.0536010334441123,0.128539649532677,
0.910865725373444));
#35175=CARTESIAN_POINT('Ctrl Pts',(-0.0562660125378511,0.126970478129068,
0.911282720586817));
#35176=CARTESIAN_POINT('Ctrl Pts',(-0.058866712211968,0.125312368815247,
0.911700977969885));
#35177=CARTESIAN_POINT('Ctrl Pts',(-0.0626444387166601,0.12290383100335,
0.912308530628704));
#35178=CARTESIAN_POINT('Ctrl Pts',(-0.0662873724862372,0.120307303169936,
0.912918858991888));
#35179=CARTESIAN_POINT('Ctrl Pts',(-0.069778152687478,0.117522359853825,
0.913532898033536));
#35180=CARTESIAN_POINT('Ctrl Pts',(-0.0759775260377567,0.112576501798998,
0.914623386993416));
#35181=CARTESIAN_POINT('Ctrl Pts',(-0.081698277829649,0.107036582207071,
0.915725579133695));
#35182=CARTESIAN_POINT('Ctrl Pts',(-0.0868900966390514,0.100989570353443,
0.916844711368391));
#35183=CARTESIAN_POINT('Ctrl Pts',(-0.0896166640492451,0.0978138845187795,
0.917432441717011));
#35184=CARTESIAN_POINT('Ctrl Pts',(-0.0921993947360654,0.0944939977198656,
0.918025537507845));
#35185=CARTESIAN_POINT('Ctrl Pts',(-0.0946128443867119,0.0910668838926417,
0.918620601845101));
#35186=CARTESIAN_POINT('Ctrl Pts',(-0.0989927195077328,0.0848474334123951,
0.919700511461385));
#35187=CARTESIAN_POINT('Ctrl Pts',(-0.102828650181205,0.0782631455551165,
0.92078926141647));
#35188=CARTESIAN_POINT('Ctrl Pts',(-0.106079098770626,0.0713949254017264,
0.921892245864136));
#35189=CARTESIAN_POINT('Ctrl Pts',(-0.108178735463834,0.0669583786746003,
0.922604721866953));
#35190=CARTESIAN_POINT('Ctrl Pts',(-0.110033655020259,0.062403198537532,
0.923323137285097));
#35191=CARTESIAN_POINT('Ctrl Pts',(-0.111627678155428,0.0577512547785083,
0.92404894598959));
#35192=CARTESIAN_POINT('Ctrl Pts',(-0.112967174079103,0.0538421147134128,
0.924658860475512));
#35193=CARTESIAN_POINT('Ctrl Pts',(-0.114123078730198,0.049859612891567,
0.925274762706783));
#35194=CARTESIAN_POINT('Ctrl Pts',(-0.11507803961208,0.0458466780964684,
0.925893033154576));
#35195=CARTESIAN_POINT('Ctrl Pts',(-0.117097308962912,0.0373613082845972,
0.92720036897266));
#35196=CARTESIAN_POINT('Ctrl Pts',(-0.118230954345967,0.0287177049851521,
0.928521669794669));
#35197=CARTESIAN_POINT('Ctrl Pts',(-0.118391771793402,0.020045083810393,
0.929866742826164));
#35198=CARTESIAN_POINT('Ctrl Pts',(-0.11848473133085,0.0150319284238029,
0.930644254028062));
#35199=CARTESIAN_POINT('Ctrl Pts',(-0.118251755364909,0.0100092161799773,
0.931429708350036));
#35200=CARTESIAN_POINT('Ctrl Pts',(-0.11766859746431,0.00500517689817996,
0.932225));
#35201=CARTESIAN_POINT('',(-0.115101970897782,0.0902398078595341,0.90365));
#35202=CARTESIAN_POINT('Origin',(0.,0.,0.90365));
#35203=CARTESIAN_POINT('Ctrl Pts',(-0.143227225569541,-2.57112916194508E-5,
0.907000235770274));
#35204=CARTESIAN_POINT('Ctrl Pts',(-0.143488833522934,0.00793898000868948,
0.90671802038504));
#35205=CARTESIAN_POINT('Ctrl Pts',(-0.143031870701996,0.0159171358242676,
0.906437106818573));
#35206=CARTESIAN_POINT('Ctrl Pts',(-0.141906651187533,0.0238323323994448,
0.906156482679268));
#35207=CARTESIAN_POINT('Ctrl Pts',(-0.141282697379586,0.0282214466835871,
0.906000871709079));
#35208=CARTESIAN_POINT('Ctrl Pts',(-0.140452894046849,0.0325912439394045,
0.905845349734719));
#35209=CARTESIAN_POINT('Ctrl Pts',(-0.139423292881505,0.0369284672537908,
0.905689744135006));
#35210=CARTESIAN_POINT('Ctrl Pts',(-0.13875911501036,0.0397263348598034,
0.905589365658919));
#35211=CARTESIAN_POINT('Ctrl Pts',(-0.138011948498085,0.0425090563696419,
0.905489007617642));
#35212=CARTESIAN_POINT('Ctrl Pts',(-0.13718658538945,0.0452640319758816,
0.905388954073411));
#35213=CARTESIAN_POINT('Ctrl Pts',(-0.134156179660795,0.0553792088866476,
0.905021597172627));
#35214=CARTESIAN_POINT('Ctrl Pts',(-0.130067939373984,0.0651554859252432,
0.904657113682601));
#35215=CARTESIAN_POINT('Ctrl Pts',(-0.125020727014944,0.07442120635967,
0.904293300817012));
#35216=CARTESIAN_POINT('Ctrl Pts',(-0.122044721725445,0.0798845851641063,
0.904078784578074));
#35217=CARTESIAN_POINT('Ctrl Pts',(-0.118734281499311,0.0851703778496932,
0.903864501493536));
#35218=CARTESIAN_POINT('Ctrl Pts',(-0.115101970897782,0.0902398078595341,
0.90365));
#35219=CARTESIAN_POINT('',(-0.05,-6.12323399573676E-18,1.));
#35220=CARTESIAN_POINT('',(-0.1,-1.22464679914735E-17,0.95));
#35221=CARTESIAN_POINT('Origin',(0.,0.,1.));
#35222=CARTESIAN_POINT('Ctrl Pts',(0.0850780204044548,-0.119080027477571,
-0.0164977839420937));
#35223=CARTESIAN_POINT('Ctrl Pts',(0.124484376148786,-0.090925728145445,
-0.0138643799872915));
#35224=CARTESIAN_POINT('Ctrl Pts',(0.17250686669983,0.00706609547096537,
-0.00859757207768696));
#35225=CARTESIAN_POINT('Ctrl Pts',(0.0881701387729916,0.148625694711589,
-0.000697360213280174));
#35226=CARTESIAN_POINT('Ctrl Pts',(-0.0762274913006873,0.154908116339636,
0.00720285165112661));
#35227=CARTESIAN_POINT('Ctrl Pts',(-0.171431501518862,0.0208683089584473,
0.0151030635155334));
#35228=CARTESIAN_POINT('Ctrl Pts',(-0.111122107950137,-0.132218525770778,
0.0230032753799401));
#35229=CARTESIAN_POINT('Ctrl Pts',(0.050013392704176,-0.165289372702636,
0.030903487244347));
#35230=CARTESIAN_POINT('Ctrl Pts',(0.165768725130536,-0.0484320089270095,
0.0388036991087536));
#35231=CARTESIAN_POINT('Ctrl Pts',(0.131132152914396,0.112382189969905,
0.0467039109731606));
#35232=CARTESIAN_POINT('Ctrl Pts',(-0.0224762869461261,0.171228238683186,
0.0546041228375672));
#35233=CARTESIAN_POINT('Ctrl Pts',(-0.155692220471689,0.0747310615070771,
0.062504334701974));
#35234=CARTESIAN_POINT('Ctrl Pts',(-0.147655869299913,-0.0895687367181161,
0.0704045465663809));
#35235=CARTESIAN_POINT('Ctrl Pts',(-0.00565764774487061,-0.172605493336333,
0.0783047584307876));
#35236=CARTESIAN_POINT('Ctrl Pts',(0.141473396847448,-0.0990455693335685,
0.0862049702951944));
#35237=CARTESIAN_POINT('Ctrl Pts',(0.160251925615185,0.0643743860018943,
0.0941051821596012));
#35238=CARTESIAN_POINT('Ctrl Pts',(0.0336409180434769,0.169390113302136,
0.102005394024008));
#35239=CARTESIAN_POINT('Ctrl Pts',(-0.123490994764231,0.120725758497873,
0.109905605888415));
#35240=CARTESIAN_POINT('Ctrl Pts',(-0.168584982150601,-0.0374678050106281,
0.117805817752822));
#35241=CARTESIAN_POINT('Ctrl Pts',(-0.0607292448116094,-0.16166845405022,
0.125706029617228));
#35242=CARTESIAN_POINT('Ctrl Pts',(0.102223455999678,-0.139194458136055,
0.133606241481635));
#35243=CARTESIAN_POINT('Ctrl Pts',(0.172433324173149,0.00956453913465353,
0.141506453346042));
#35244=CARTESIAN_POINT('Ctrl Pts',(0.086202040450112,0.149646047845283,
0.149406665210448));
#35245=CARTESIAN_POINT('Ctrl Pts',(-0.0782365529804317,0.153960298370095,
0.157306877074856));
#35246=CARTESIAN_POINT('Ctrl Pts',(-0.171694572067167,0.0185931582621336,
0.165207088939262));
#35247=CARTESIAN_POINT('Ctrl Pts',(-0.109381677027807,-0.133642733856025,
0.173107300803669));
#35248=CARTESIAN_POINT('Ctrl Pts',(0.052168390130379,-0.164630467088263,
0.181007512668076));
#35249=CARTESIAN_POINT('Ctrl Pts',(0.166388377416592,-0.04625623707159,
0.188907724532483));
#35250=CARTESIAN_POINT('Ctrl Pts',(0.129651527078137,0.114084236996722,
0.19680793639689));
#35251=CARTESIAN_POINT('Ctrl Pts',(-0.0247124365344563,0.170921113648968,
0.204708148261296));
#35252=CARTESIAN_POINT('Ctrl Pts',(-0.156655896226217,0.072688800963294,
0.212608360125703));
#35253=CARTESIAN_POINT('Ctrl Pts',(-0.146472369316595,-0.0914908554698463,
0.22050857199011));
#35254=CARTESIAN_POINT('Ctrl Pts',(-0.00340092071136592,-0.172664893209074,
0.228408783854516));
#35255=CARTESIAN_POINT('Ctrl Pts',(0.142756033285632,-0.0971876873308804,
0.236308995718923));
#35256=CARTESIAN_POINT('Ctrl Pts',(0.159396733387471,0.0664636215805494,
0.24420920758333));
#35257=CARTESIAN_POINT('Ctrl Pts',(0.0314238061962717,0.169815417475675,
0.252109419447737));
#35258=CARTESIAN_POINT('Ctrl Pts',(-0.12505855466298,0.119101173436036,
0.260009631312144));
#35259=CARTESIAN_POINT('Ctrl Pts',(-0.168080803576887,-0.0396683132637571,
0.26790984317655));
#35260=CARTESIAN_POINT('Ctrl Pts',(-0.0586107512557457,-0.162448488590979,
0.275810055040957));
#35261=CARTESIAN_POINT('Ctrl Pts',(0.104034251124571,-0.137846313701876,
0.283710266905363));
#35262=CARTESIAN_POINT('Ctrl Pts',(0.172293565052386,0.0118177430073507,
0.291610478769771));
#35263=CARTESIAN_POINT('Ctrl Pts',(0.084238525028331,0.150760082612412,
0.299510690634177));
#35264=CARTESIAN_POINT('Ctrl Pts',(-0.0802424140921812,0.15292444732255,
0.307410902498584));
#35265=CARTESIAN_POINT('Ctrl Pts',(-0.171922949352315,0.0163472044781485,
0.315311114362991));
#35266=CARTESIAN_POINT('Ctrl Pts',(-0.107625373942229,-0.135061136127476,
0.323211326227398));
#35267=CARTESIAN_POINT('Ctrl Pts',(0.0543159572952621,-0.163934463708362,
0.331111538091804));
#35268=CARTESIAN_POINT('Ctrl Pts',(0.166978815646636,-0.0440772813759624,
0.339011749956212));
#35269=CARTESIAN_POINT('Ctrl Pts',(0.128149157817753,0.11576927467532,0.346911961820618));
#35270=CARTESIAN_POINT('Ctrl Pts',(-0.0269445799125943,0.17058347288522,
0.354812173685025));
#35271=CARTESIAN_POINT('Ctrl Pts',(-0.157592688461949,0.070634808356674,
0.362712385549432));
#35272=CARTESIAN_POINT('Ctrl Pts',(-0.145263900126163,-0.0933977030145032,
0.370612597413839));
#35273=CARTESIAN_POINT('Ctrl Pts',(-0.00114358090037083,-0.172694596994154,
0.378512809278245));
#35274=CARTESIAN_POINT('Ctrl Pts',(0.144014258847901,-0.0953132984254496,
0.386413021142653));
#35275=CARTESIAN_POINT('Ctrl Pts',(0.15851431213257,0.0685415527792242,
0.394313233007058));
#35276=CARTESIAN_POINT('Ctrl Pts',(0.0292013200165327,0.170211675620508,
0.402213444871466));
#35277=CARTESIAN_POINT('Ctrl Pts',(-0.126604742061452,0.117456250986493,
0.410113656735872));
#35278=CARTESIAN_POINT('Ctrl Pts',(-0.167547904549645,-0.0418620507055259,
0.418013868600279));
#35279=CARTESIAN_POINT('Ctrl Pts',(-0.0564822415909637,-0.163200759781041,
0.425914080464686));
#35280=CARTESIAN_POINT('Ctrl Pts',(0.105827268468801,-0.136474616162425,
0.433814292329093));
#35281=CARTESIAN_POINT('Ctrl Pts',(0.172124364506242,0.0140689285864832,
0.441714504193499));
#35282=CARTESIAN_POINT('Ctrl Pts',(0.0822606147860967,0.15184835482567,
0.449614716057907));
#35283=CARTESIAN_POINT('Ctrl Pts',(-0.0822345632875265,0.151862464780335,
0.457514927922313));
#35284=CARTESIAN_POINT('Ctrl Pts',(-0.172121948383532,0.0140984571108209,
0.465415139786721));
#35285=CARTESIAN_POINT('Ctrl Pts',(-0.105850679763545,-0.13645645899643,
0.473315351651126));
#35286=CARTESIAN_POINT('Ctrl Pts',(0.0564542429141223,-0.163210447169421,
0.481215563515534));
#35287=CARTESIAN_POINT('Ctrl Pts',(0.167540720455548,-0.0418907937079863,
0.48911577537994));
#35288=CARTESIAN_POINT('Ctrl Pts',(0.126624890361875,0.117434529628606,
0.497015987244348));
#35289=CARTESIAN_POINT('Ctrl Pts',(-0.0291721189860838,0.170216682737359,
0.504916199108753));
#35290=CARTESIAN_POINT('Ctrl Pts',(-0.158502551179345,0.068568745634494,
0.512816410973161));
#35291=CARTESIAN_POINT('Ctrl Pts',(-0.14403060816614,-0.0952885907102249,
0.520716622837567));
#35292=CARTESIAN_POINT('Ctrl Pts',(0.00111395432615138,-0.172694790639464,
0.528616834701974));
#35293=CARTESIAN_POINT('Ctrl Pts',(0.145247875180311,-0.0934226223344961,
0.536517046566381));
#35294=CARTESIAN_POINT('Ctrl Pts',(0.157604803871184,0.0706077715621608,
0.544417258430788));
#35295=CARTESIAN_POINT('Ctrl Pts',(0.0269738439003715,0.170578847907609,
0.552317470295194));
#35296=CARTESIAN_POINT('Ctrl Pts',(-0.128129295177092,0.11579125755285,
0.560217682159602));
#35297=CARTESIAN_POINT('Ctrl Pts',(-0.166986374851081,-0.0440486347386962,
0.568117894024008));
#35298=CARTESIAN_POINT('Ctrl Pts',(-0.0543440802119571,-0.163925143142123,
0.576018105888415));
#35299=CARTESIAN_POINT('Ctrl Pts',(0.107602201995467,-0.135079597771001,
0.583918317752822));
#35300=CARTESIAN_POINT('Ctrl Pts',(0.171925751260969,0.0163177100599224,
0.591818529617229));
#35301=CARTESIAN_POINT('Ctrl Pts',(0.0802686478080903,0.152910679114674,
0.599718741481635));
#35302=CARTESIAN_POINT('Ctrl Pts',(-0.0842126601987931,0.150774531902743,
0.607618953346042));
#35303=CARTESIAN_POINT('Ctrl Pts',(-0.172291535128485,0.0118473005919646,
0.615519165210449));
#35304=CARTESIAN_POINT('Ctrl Pts',(-0.104057897766774,-0.137828464116146,
0.623419377074855));
#35305=CARTESIAN_POINT('Ctrl Pts',(0.0585828816032124,-0.162458541146064,
0.631319588939263));
#35306=CARTESIAN_POINT('Ctrl Pts',(0.168073995820709,-0.0396971477198862,
0.639219800803669));
#35307=CARTESIAN_POINT('Ctrl Pts',(0.12507898518031,0.119079717309719,0.647120012668075));
#35308=CARTESIAN_POINT('Ctrl Pts',(-0.0313946731132146,0.169820805875821,
0.655020224532484));
#35309=CARTESIAN_POINT('Ctrl Pts',(-0.159385328899637,0.0664909658504678,
0.662920436396888));
#35310=CARTESIAN_POINT('Ctrl Pts',(-0.142772704183121,-0.0971631954436711,
0.670820648261297));
#35311=CARTESIAN_POINT('Ctrl Pts',(0.00337129920097031,-0.172665474109675,
0.678720860125702));
#35312=CARTESIAN_POINT('Ctrl Pts',(0.146456671479165,-0.0915159821406338,
0.68662107199011));
#35313=CARTESIAN_POINT('Ctrl Pts',(0.156668364025577,0.0726619248576747,
0.694521283854517));
#35314=CARTESIAN_POINT('Ctrl Pts',(0.0247417584705585,0.17091687158558,
0.702421495718924));
#35315=CARTESIAN_POINT('Ctrl Pts',(-0.129631953475511,0.114106477666574,
0.71032170758333));
#35316=CARTESIAN_POINT('Ctrl Pts',(-0.166396310469803,-0.0462276917499887,
0.718221919447737));
#35317=CARTESIAN_POINT('Ctrl Pts',(-0.0521966324240299,-0.164621514831807,
0.726122131312144));
#35318=CARTESIAN_POINT('Ctrl Pts',(0.109358748279947,-0.133661497021884,
0.73402234317655));
#35319=CARTESIAN_POINT('Ctrl Pts',(0.171697759489448,0.0185637033690059,
0.741922555040957));
#35320=CARTESIAN_POINT('Ctrl Pts',(0.0782629640387094,0.153946873541983,
0.749822766905365));
#35321=CARTESIAN_POINT('Ctrl Pts',(-0.0861763659646394,0.149660835369141,
0.75772297876977));
#35322=CARTESIAN_POINT('Ctrl Pts',(-0.17243168220941,0.00959411813254083,
0.765623190634177));
#35323=CARTESIAN_POINT('Ctrl Pts',(-0.102247331262163,-0.139176914249964,
0.773523402498585));
#35324=CARTESIAN_POINT('Ctrl Pts',(0.0607015038436091,-0.161678879418918,
0.78142361436299));
#35325=CARTESIAN_POINT('Ctrl Pts',(0.168578561585846,-0.0374967082074332,
0.7893238262274));
#35326=CARTESIAN_POINT('Ctrl Pts',(0.123511685603348,0.120704537490262,
0.797224038091803));
#35327=CARTESIAN_POINT('Ctrl Pts',(-0.0336118229326868,0.169395946219611,
0.805124249956213));
#35328=CARTESIAN_POINT('Ctrl Pts',(-0.16024094592625,0.0644017551688373,
0.813024461820617));
#35329=CARTESIAN_POINT('Ctrl Pts',(-0.141490260395339,-0.0990210660472952,
0.820924673685026));
#35330=CARTESIAN_POINT('Ctrl Pts',(0.0056277969043301,-0.172606900899112,
0.828824885549431));
#35331=CARTESIAN_POINT('Ctrl Pts',(0.147640956035951,-0.0895932317207615,
0.836725097413839));
#35332=CARTESIAN_POINT('Ctrl Pts',(0.15570417479137,0.0747027653435218,
0.844625309278246));
#35333=CARTESIAN_POINT('Ctrl Pts',(0.022507302267937,0.171227391193745,
0.852525521142652));
#35334=CARTESIAN_POINT('Ctrl Pts',(-0.131115987327984,0.112398966130108,
0.860425733007058));
#35335=CARTESIAN_POINT('Ctrl Pts',(-0.16577111303378,-0.0483927087664539,
0.868325944871467));
#35336=CARTESIAN_POINT('Ctrl Pts',(-0.050052991301314,-0.165301420121155,
0.876226156735872));
#35337=CARTESIAN_POINT('Ctrl Pts',(0.111120800514148,-0.132198387754511,
0.884126368600279));
#35338=CARTESIAN_POINT('Ctrl Pts',(0.171394279774569,0.0207642914265632,
0.892026580464686));
#35339=CARTESIAN_POINT('Ctrl Pts',(0.0763332480962674,0.155038078338273,
0.899926792329093));
#35340=CARTESIAN_POINT('Ctrl Pts',(-0.0883093241020301,0.148357716484315,
0.9078270041935));
#35341=CARTESIAN_POINT('Ctrl Pts',(-0.14415958729081,0.0546064221138428,
0.913093812103104));
#35342=CARTESIAN_POINT('Ctrl Pts',(-0.146217781693074,0.00621955117001918,
0.915727216057906));
#35343=CARTESIAN_POINT('Ctrl Pts',(0.0795408277542851,-0.111329858282328,
-0.0109985226280626));
#35344=CARTESIAN_POINT('Ctrl Pts',(0.116382471927282,-0.0850079450187934,
-0.00836511867326029));
#35345=CARTESIAN_POINT('Ctrl Pts',(0.161279480944341,0.00660620780878029,
-0.00309831076365578));
#35346=CARTESIAN_POINT('Ctrl Pts',(0.0824316996078882,0.138952584071836,
0.00480190110075102));
#35347=CARTESIAN_POINT('Ctrl Pts',(-0.0712663238620885,0.144826122433691,
0.0127021129651578));
#35348=CARTESIAN_POINT('Ctrl Pts',(-0.160274104511912,0.0195101221266785,
0.0206023248295645));
#35349=CARTESIAN_POINT('Ctrl Pts',(-0.103889869629501,-0.123613254448834,
0.0285025366939713));
#35350=CARTESIAN_POINT('Ctrl Pts',(0.0467583358848584,-0.154531728186116,
0.0364027485583782));
#35351=CARTESIAN_POINT('Ctrl Pts',(0.154979882582751,-0.0452798744204848,
0.0443029604227849));
#35352=CARTESIAN_POINT('Ctrl Pts',(0.122597586761272,0.105067940844772,
0.0522031722871918));
#35353=CARTESIAN_POINT('Ctrl Pts',(-0.0210134469518542,0.160084070774355,
0.0601033841515984));
#35354=CARTESIAN_POINT('Ctrl Pts',(-0.145559194164939,0.0698672872613988,
0.0680035960160053));
#35355=CARTESIAN_POINT('Ctrl Pts',(-0.138045878489652,-0.0837392716191075,
0.0759038078804119));
#35356=CARTESIAN_POINT('Ctrl Pts',(-0.00528942707681416,-0.16137168859408,
0.083804019744819));
#35357=CARTESIAN_POINT('Ctrl Pts',(0.132265784240875,-0.0925993168709629,
0.0917042316092254));
#35358=CARTESIAN_POINT('Ctrl Pts',(0.149822136811053,0.0601846625535317,
0.0996044434736326));
#35359=CARTESIAN_POINT('Ctrl Pts',(0.0314514425097271,0.15836557740051,
0.107504655338039));
#35360=CARTESIAN_POINT('Ctrl Pts',(-0.115453743482173,0.112868479032945,
0.115404867202446));
#35361=CARTESIAN_POINT('Ctrl Pts',(-0.157612847166081,-0.0350292615003714,
0.123305079066853));
#35362=CARTESIAN_POINT('Ctrl Pts',(-0.0567767606515088,-0.151146472329493,
0.13120529093126));
#35363=CARTESIAN_POINT('Ctrl Pts',(0.0955703749036966,-0.130135167300756,
0.139105502795666));
#35364=CARTESIAN_POINT('Ctrl Pts',(0.161210724837657,0.00894204350597287,
0.147005714660073));
#35365=CARTESIAN_POINT('Ctrl Pts',(0.0805916924126166,0.139906528844762,
0.15490592652448));
#35366=CARTESIAN_POINT('Ctrl Pts',(-0.0731446283672545,0.143939991967805,
0.162806138388887));
#35367=CARTESIAN_POINT('Ctrl Pts',(-0.160520053454664,0.0173830466635891,
0.170706350253294));
#35368=CARTESIAN_POINT('Ctrl Pts',(-0.102262712397196,-0.124944769797408,
0.1786065621177));
#35369=CARTESIAN_POINT('Ctrl Pts',(0.0487730780976374,-0.153915706589351,
0.186506773982107));
#35370=CARTESIAN_POINT('Ctrl Pts',(0.155559205603179,-0.0432457098552795,
0.194406985846514));
#35371=CARTESIAN_POINT('Ctrl Pts',(0.121213325537862,0.106659212347636,
0.202307197710921));
#35372=CARTESIAN_POINT('Ctrl Pts',(-0.0231040596435062,0.159796934574786,
0.210207409575327));
#35373=CARTESIAN_POINT('Ctrl Pts',(-0.146460150332438,0.0679579445972159,
0.218107621439734));
#35374=CARTESIAN_POINT('Ctrl Pts',(-0.136939405068282,-0.0855362917640029,
0.226007833304141));
#35375=CARTESIAN_POINT('Ctrl Pts',(-0.00317957619632727,-0.16142722250312,
0.233908045168548));
#35376=CARTESIAN_POINT('Ctrl Pts',(0.133464941949482,-0.0908623527095838,
0.241808257032955));
#35377=CARTESIAN_POINT('Ctrl Pts',(0.149022603660681,0.0621379229433468,
0.249708468897361));
#35378=CARTESIAN_POINT('Ctrl Pts',(0.0293786285125025,0.158763201203343,
0.257608680761768));
#35379=CARTESIAN_POINT('Ctrl Pts',(-0.11691928077733,0.111349627983502,
0.265508892626175));
#35380=CARTESIAN_POINT('Ctrl Pts',(-0.157141482401145,-0.0370865525269131,
0.273409104490581));
#35381=CARTESIAN_POINT('Ctrl Pts',(-0.0547961465019971,-0.15187573933352,
0.281309316354988));
#35382=CARTESIAN_POINT('Ctrl Pts',(0.0972633167756718,-0.12887476509914,
0.289209528219395));
#35383=CARTESIAN_POINT('Ctrl Pts',(0.161080061758064,0.0110486005260055,
0.297109740083802));
#35384=CARTESIAN_POINT('Ctrl Pts',(0.0787559698462676,0.140948058103473,
0.305009951948209));
#35385=CARTESIAN_POINT('Ctrl Pts',(-0.0750199406092437,0.142971557942657,
0.312910163812615));
#35386=CARTESIAN_POINT('Ctrl Pts',(-0.160733567100311,0.0152832678696448,
0.320810375677022));
#35387=CARTESIAN_POINT('Ctrl Pts',(-0.100620716020809,-0.12627085719605,
0.328710587541429));
#35388=CARTESIAN_POINT('Ctrl Pts',(0.050780873638021,-0.153265001687028,
0.336610799405836));
#35389=CARTESIAN_POINT('Ctrl Pts',(0.156111215926553,-0.0412085686659782,
0.344511011270243));
#35390=CARTESIAN_POINT('Ctrl Pts',(0.119808736032893,0.108234581533658,
0.35241122313465));
#35391=CARTESIAN_POINT('Ctrl Pts',(-0.0251909268639622,0.15948126872238,
0.360311434999056));
#35392=CARTESIAN_POINT('Ctrl Pts',(-0.147335972660104,0.066037633436295,
0.368211646863463));
#35393=CARTESIAN_POINT('Ctrl Pts',(-0.135809587528269,-0.0873190346085379,
0.37611185872787));
#35394=CARTESIAN_POINT('Ctrl Pts',(-0.00106915242017828,-0.16145499305586,
0.384012070592276));
#35395=CARTESIAN_POINT('Ctrl Pts',(0.134641277532382,-0.0891099559758252,
0.391912282456683));
#35396=CARTESIAN_POINT('Ctrl Pts',(0.148197613649053,0.0640806146840961,
0.39981249432109));
#35397=CARTESIAN_POINT('Ctrl Pts',(0.0273007899642087,0.159133669400588,
0.407712706185496));
#35398=CARTESIAN_POINT('Ctrl Pts',(-0.118364836573682,0.109811763178865,
0.415612918049904));
#35399=CARTESIAN_POINT('Ctrl Pts',(-0.156643266416161,-0.0391375134115731,
0.42351312991431));
#35400=CARTESIAN_POINT('Ctrl Pts',(-0.0528061681290295,-0.152579049928534,
0.431413341778717));
#35401=CARTESIAN_POINT('Ctrl Pts',(0.0989396379107883,-0.12759234271557,
0.439313553643124));
#35402=CARTESIAN_POINT('Ctrl Pts',(0.160921873410089,0.0131532706104934,
0.447213765507531));
#35403=CARTESIAN_POINT('Ctrl Pts',(0.0769067893276909,0.14196550153073,
0.455113977371937));
#35404=CARTESIAN_POINT('Ctrl Pts',(-0.0768824333571298,0.14197869315729,
0.463014189236344));
#35405=CARTESIAN_POINT('Ctrl Pts',(-0.160919614537593,0.0131808773091078,
0.470914401100751));
#35406=CARTESIAN_POINT('Ctrl Pts',(-0.098961525511766,-0.127575367285184,
0.478814612965158));
#35407=CARTESIAN_POINT('Ctrl Pts',(0.0527799917097706,-0.152588106825801,
0.486714824829564));
#35408=CARTESIAN_POINT('Ctrl Pts',(0.156636549889514,-0.0391643857129832,
0.494615036693972));
#35409=CARTESIAN_POINT('Ctrl Pts',(0.118383673548094,0.109791455527395,
0.502515248558378));
#35410=CARTESIAN_POINT('Ctrl Pts',(-0.027273489444968,0.15913835063573,
0.510415460422786));
#35411=CARTESIAN_POINT('Ctrl Pts',(-0.14818661814222,0.0641060377276359,
0.518315672287191));
#35412=CARTESIAN_POINT('Ctrl Pts',(-0.13465656277644,-0.0890868563302129,
0.526215884151598));
#35413=CARTESIAN_POINT('Ctrl Pts',(0.00104145405313166,-0.161455174098016,
0.534116096016006));
#35414=CARTESIAN_POINT('Ctrl Pts',(0.135794605545242,-0.0873423320868967,
0.542016307880412));
#35415=CARTESIAN_POINT('Ctrl Pts',(0.147347299553637,0.0660123562965002,
0.549916519744819));
#35416=CARTESIAN_POINT('Ctrl Pts',(0.025218286243035,0.15947694475544,0.557816731609225));
#35417=CARTESIAN_POINT('Ctrl Pts',(-0.119790166126449,0.108255133684104,
0.565716943473633));
#35418=CARTESIAN_POINT('Ctrl Pts',(-0.156118283149977,-0.0411817864579589,
0.573617155338038));
#35419=CARTESIAN_POINT('Ctrl Pts',(-0.0508071662111437,-0.153256287737759,
0.581517367202447));
#35420=CARTESIAN_POINT('Ctrl Pts',(0.10059905219016,-0.126288117287442,
0.589417579066852));
#35421=CARTESIAN_POINT('Ctrl Pts',(0.160736186650373,0.0152556930573902,
0.597317790931261));
#35422=CARTESIAN_POINT('Ctrl Pts',(0.0750444669377644,0.14295868582074,
0.605218002795666));
#35423=CARTESIAN_POINT('Ctrl Pts',(-0.0787317883956269,0.140961566980476,
0.613118214660074));
#35424=CARTESIAN_POINT('Ctrl Pts',(-0.161078163949129,0.0110762343935455,
0.62101842652448));
#35425=CARTESIAN_POINT('Ctrl Pts',(-0.097285424406824,-0.128858077230555,
0.628918638388887));
#35426=CARTESIAN_POINT('Ctrl Pts',(0.0547700907096662,-0.151885137631092,
0.636818850253293));
#35427=CARTESIAN_POINT('Ctrl Pts',(0.157135117718952,-0.037113510329848,
0.644719062117701));
#35428=CARTESIAN_POINT('Ctrl Pts',(0.116938381600928,0.111329568301349,
0.652619273982107));
#35429=CARTESIAN_POINT('Ctrl Pts',(-0.0293513915183856,0.158768238906452,
0.660519485846514));
#35430=CARTESIAN_POINT('Ctrl Pts',(-0.149011941419152,0.0621634875469089,
0.668419697710921));
#35431=CARTESIAN_POINT('Ctrl Pts',(-0.133480527843221,-0.0908394548451002,
0.676319909575327));
#35432=CARTESIAN_POINT('Ctrl Pts',(0.00315188256353199,-0.161427765596558,
0.684220121439734));
#35433=CARTESIAN_POINT('Ctrl Pts',(0.136924728904249,-0.0855597830979986,
0.692120333304141));
#35434=CARTESIAN_POINT('Ctrl Pts',(0.14647180668124,0.0679328176880866,
0.700020545168548));
#35435=CARTESIAN_POINT('Ctrl Pts',(0.0231314731994126,0.159792968600594,
0.707920757032954));
#35436=CARTESIAN_POINT('Ctrl Pts',(-0.121195025857785,0.106680005512326,
0.715820968897362));
#35437=CARTESIAN_POINT('Ctrl Pts',(-0.155566622343907,-0.0432190223689262,
0.723721180761768));
#35438=CARTESIAN_POINT('Ctrl Pts',(-0.0487994822782217,-0.1539073369789,
0.731621392626175));
#35439=CARTESIAN_POINT('Ctrl Pts',(0.102241275937164,-0.124962311786944,
0.739521604490582));
#35440=CARTESIAN_POINT('Ctrl Pts',(0.160523033427699,0.0173555088039932,
0.747421816354988));
#35441=CARTESIAN_POINT('Ctrl Pts',(0.0731693204960455,0.143927440877225,
0.755322028219396));
#35442=CARTESIAN_POINT('Ctrl Pts',(-0.0805676889177445,0.139920353941802,
0.763222240083802));
#35443=CARTESIAN_POINT('Ctrl Pts',(-0.161209189739,0.00896969739313117,
0.771122451948209));
#35444=CARTESIAN_POINT('Ctrl Pts',(-0.0955926962756769,-0.130118765235746,
0.779022663812615));
#35445=CARTESIAN_POINT('Ctrl Pts',(0.0567508251684453,-0.151156219176586,
0.786922875677023));
#35446=CARTESIAN_POINT('Ctrl Pts',(0.157606844475459,-0.0350562835700847,
0.794823087541428));
#35447=CARTESIAN_POINT('Ctrl Pts',(0.115473087684851,0.112848639167101,
0.802723299405837));
#35448=CARTESIAN_POINT('Ctrl Pts',(-0.0314242410165019,0.158371030690115,
0.810623511270242));
#35449=CARTESIAN_POINT('Ctrl Pts',(-0.149811871720937,0.0602102504337274,
0.81852372313465));
#35450=CARTESIAN_POINT('Ctrl Pts',(-0.132281550246616,-0.0925764083493082,
0.826423934999057));
#35451=CARTESIAN_POINT('Ctrl Pts',(0.00526151903952945,-0.161373004547461,
0.834324146863462));
#35452=CARTESIAN_POINT('Ctrl Pts',(0.138031935836139,-0.0837621723962628,
0.842224358727871));
#35453=CARTESIAN_POINT('Ctrl Pts',(0.145570370453223,0.0698408327169628,
0.850124570592276));
#35454=CARTESIAN_POINT('Ctrl Pts',(0.0210424436816558,0.160083278442666,
0.858024782456684));
#35455=CARTESIAN_POINT('Ctrl Pts',(-0.122582473291093,0.105083625150338,
0.86592499432109));
#35456=CARTESIAN_POINT('Ctrl Pts',(-0.154982115072408,-0.0452431320599261,
0.873825206185497));
#35457=CARTESIAN_POINT('Ctrl Pts',(-0.0467953572586411,-0.154542991514022,
0.881725418049904));
#35458=CARTESIAN_POINT('Ctrl Pts',(0.103888647286289,-0.123594427089244,
0.88962562991431));
#35459=CARTESIAN_POINT('Ctrl Pts',(0.160239305296586,0.0194128744409952,
0.897525841778718));
#35460=CARTESIAN_POINT('Ctrl Pts',(0.0713651976137454,0.14494762602415,
0.905426053643123));
#35461=CARTESIAN_POINT('Ctrl Pts',(-0.0825618262402486,0.138702046860037,
0.913326265507531));
#35462=CARTESIAN_POINT('Ctrl Pts',(-0.134777147462009,0.0510524339304846,
0.918593073417135));
#35463=CARTESIAN_POINT('Ctrl Pts',(-0.136701386950153,0.00581475974607277,
0.921226477371938));
#35464=CARTESIAN_POINT('Ctrl Pts',(0.0740036351041154,-0.103579689087084,
-0.00549926131403137));
#35465=CARTESIAN_POINT('Ctrl Pts',(0.108280567705778,-0.0790901618921417,
-0.00286585735922911));
#35466=CARTESIAN_POINT('Ctrl Pts',(0.150052095188851,0.00614632014659505,
0.00240095055037541));
#35467=CARTESIAN_POINT('Ctrl Pts',(0.0766932604427849,0.129279473432083,
0.0103011624147822));
#35468=CARTESIAN_POINT('Ctrl Pts',(-0.0663051564234898,0.134744128527746,
0.018201374279189));
#35469=CARTESIAN_POINT('Ctrl Pts',(-0.149116707504962,0.0181519352949098,
0.0261015861435957));
#35470=CARTESIAN_POINT('Ctrl Pts',(-0.0966576313088641,-0.115007983126889,
0.0340017980080025));
#35471=CARTESIAN_POINT('Ctrl Pts',(0.0435032790655407,-0.143774083669597,
0.0419020098724094));
#35472=CARTESIAN_POINT('Ctrl Pts',(0.144191040034967,-0.04212773991396,
0.0498022217368161));
#35473=CARTESIAN_POINT('Ctrl Pts',(0.114063020608148,0.0977536917196387,
0.0577024336012229));
#35474=CARTESIAN_POINT('Ctrl Pts',(-0.0195506069575822,0.148939902865525,
0.0656026454656297));
#35475=CARTESIAN_POINT('Ctrl Pts',(-0.13542616785819,0.0650035130157202,
0.0735028573300364));
#35476=CARTESIAN_POINT('Ctrl Pts',(-0.12843588767939,-0.0779098065200985,
0.0814030691944432));
#35477=CARTESIAN_POINT('Ctrl Pts',(-0.00492120640875794,-0.150137883851829,
0.0893032810588501));
#35478=CARTESIAN_POINT('Ctrl Pts',(0.123058171634303,-0.0861530644083569,
0.0972034929232567));
#35479=CARTESIAN_POINT('Ctrl Pts',(0.139392348006922,0.0559949391051687,
0.105103704787664));
#35480=CARTESIAN_POINT('Ctrl Pts',(0.0292619669759775,0.147341041498886,
0.11300391665207));
#35481=CARTESIAN_POINT('Ctrl Pts',(-0.107416492200115,0.105011199568016,
0.120904128516477));
#35482=CARTESIAN_POINT('Ctrl Pts',(-0.146640712181561,-0.0325907179901145,
0.128804340380884));
#35483=CARTESIAN_POINT('Ctrl Pts',(-0.0528242764914083,-0.140624490608767,
0.136704552245291));
#35484=CARTESIAN_POINT('Ctrl Pts',(0.0889172938077157,-0.121075876465457,
0.144604764109697));
#35485=CARTESIAN_POINT('Ctrl Pts',(0.149988125502165,0.00831954787729212,
0.152504975974104));
#35486=CARTESIAN_POINT('Ctrl Pts',(0.0749813443751213,0.130167009844241,
0.160405187838511));
#35487=CARTESIAN_POINT('Ctrl Pts',(-0.0680527037540773,0.133919685565514,
0.168305399702918));
#35488=CARTESIAN_POINT('Ctrl Pts',(-0.149345534842162,0.0161729350650448,
0.176205611567325));
#35489=CARTESIAN_POINT('Ctrl Pts',(-0.0951437477665844,-0.116246805738792,
0.184105823431731));
#35490=CARTESIAN_POINT('Ctrl Pts',(0.0453777660648959,-0.143200946090439,
0.192006035296138));
#35491=CARTESIAN_POINT('Ctrl Pts',(0.144730033789766,-0.040235182638969,
0.199906247160545));
#35492=CARTESIAN_POINT('Ctrl Pts',(0.112775123997586,0.0992341876985505,
0.207806459024951));
#35493=CARTESIAN_POINT('Ctrl Pts',(-0.021495682752556,0.148672755500605,
0.215706670889359));
#35494=CARTESIAN_POINT('Ctrl Pts',(-0.136264404438658,0.063227088231138,
0.223606882753765));
#35495=CARTESIAN_POINT('Ctrl Pts',(-0.127406440819969,-0.0795817280581598,
0.231507094618172));
#35496=CARTESIAN_POINT('Ctrl Pts',(-0.00295823168128856,-0.150189551797165,
0.239407306482579));
#35497=CARTESIAN_POINT('Ctrl Pts',(0.124173850613332,-0.0845370180882872,
0.247307518346986));
#35498=CARTESIAN_POINT('Ctrl Pts',(0.138648473933891,0.0578122243061442,
0.255207730211393));
#35499=CARTESIAN_POINT('Ctrl Pts',(0.0273334508287331,0.147710984931011,
0.263107942075799));
#35500=CARTESIAN_POINT('Ctrl Pts',(-0.108780006891681,0.103598082530968,
0.271008153940206));
#35501=CARTESIAN_POINT('Ctrl Pts',(-0.146202161225402,-0.0345047917900689,
0.278908365804612));
#35502=CARTESIAN_POINT('Ctrl Pts',(-0.0509815417482485,-0.141302990076062,
0.28680857766902));
#35503=CARTESIAN_POINT('Ctrl Pts',(0.0904923824267724,-0.119903216496403,
0.294708789533426));
#35504=CARTESIAN_POINT('Ctrl Pts',(0.149866558463742,0.0102794580446603,
0.302609001397833));
#35505=CARTESIAN_POINT('Ctrl Pts',(0.0732734146642041,0.131136033594535,
0.31050921326224));
#35506=CARTESIAN_POINT('Ctrl Pts',(-0.0697974671263062,0.133018668562764,
0.318409425126647));
#35507=CARTESIAN_POINT('Ctrl Pts',(-0.149544184848307,0.0142193312611412,
0.326309636991054));
#35508=CARTESIAN_POINT('Ctrl Pts',(-0.0936160580993886,-0.117480578264625,
0.33420984885546));
#35509=CARTESIAN_POINT('Ctrl Pts',(0.0472457899807798,-0.142595539665694,
0.342110060719868));
#35510=CARTESIAN_POINT('Ctrl Pts',(0.14524361620647,-0.0383398559559941,
0.350010272584273));
#35511=CARTESIAN_POINT('Ctrl Pts',(0.111468314248034,0.100699888391995,
0.357910484448681));
#35512=CARTESIAN_POINT('Ctrl Pts',(-0.02343727381533,0.148379064559539,
0.365810696313087));
#35513=CARTESIAN_POINT('Ctrl Pts',(-0.137079256858259,0.0614404585159162,
0.373710908177495));
#35514=CARTESIAN_POINT('Ctrl Pts',(-0.126355274930375,-0.0812403662025727,
0.381611120041901));
#35515=CARTESIAN_POINT('Ctrl Pts',(-0.000994723939985704,-0.150215389117566,
0.389511331906308));
#35516=CARTESIAN_POINT('Ctrl Pts',(0.125268296216863,-0.0829066135262008,
0.397411543770714));
#35517=CARTESIAN_POINT('Ctrl Pts',(0.137880915165535,0.0596196765889682,
0.405311755635121));
#35518=CARTESIAN_POINT('Ctrl Pts',(0.0254002599118846,0.148055663180668,
0.413211967499528));
#35519=CARTESIAN_POINT('Ctrl Pts',(-0.110124931085911,0.102167275371236,
0.421112179363935));
#35520=CARTESIAN_POINT('Ctrl Pts',(-0.145738628282677,-0.0364129761176204,
0.429012391228342));
#35521=CARTESIAN_POINT('Ctrl Pts',(-0.0491300946670952,-0.141957340076027,
0.436912603092748));
#35522=CARTESIAN_POINT('Ctrl Pts',(0.0920520073527751,-0.118710069268716,
0.444812814957155));
#35523=CARTESIAN_POINT('Ctrl Pts',(0.149719382313936,0.0122376126345037,
0.452713026821562));
#35524=CARTESIAN_POINT('Ctrl Pts',(0.0715529638692849,0.13208264823579,
0.460613238685969));
#35525=CARTESIAN_POINT('Ctrl Pts',(-0.071530303426733,0.132094921534244,
0.468513450550375));
#35526=CARTESIAN_POINT('Ctrl Pts',(-0.149717280691655,0.0122632975073946,
0.476413662414783));
#35527=CARTESIAN_POINT('Ctrl Pts',(-0.0920723712599867,-0.118694275573937,
0.484313874279189));
#35528=CARTESIAN_POINT('Ctrl Pts',(0.0491057405054188,-0.141965766482181,
0.492214086143596));
#35529=CARTESIAN_POINT('Ctrl Pts',(0.14573237932348,-0.03643797771798,0.500114298008002));
#35530=CARTESIAN_POINT('Ctrl Pts',(0.110142456734312,0.102148381426183,
0.50801450987241));
#35531=CARTESIAN_POINT('Ctrl Pts',(-0.0253748599038521,0.148060018534101,
0.515914721736816));
#35532=CARTESIAN_POINT('Ctrl Pts',(-0.137870685105096,0.0596433298207777,
0.523814933601224));
#35533=CARTESIAN_POINT('Ctrl Pts',(-0.125282517386741,-0.0828851219502007,
0.531715145465628));
#35534=CARTESIAN_POINT('Ctrl Pts',(0.00096895378011186,-0.150215557556568,
0.539615357330038));
#35535=CARTESIAN_POINT('Ctrl Pts',(0.126341335910172,-0.0812620418392971,
0.547515569194442));
#35536=CARTESIAN_POINT('Ctrl Pts',(0.137089795236089,0.0614169410308395,
0.55541578105885));
#35537=CARTESIAN_POINT('Ctrl Pts',(0.0234627285856986,0.148375041603271,
0.563315992923257));
#35538=CARTESIAN_POINT('Ctrl Pts',(-0.111451037075805,0.100719009815358,
0.571216204787664));
#35539=CARTESIAN_POINT('Ctrl Pts',(-0.145250191448873,-0.0383149381772212,
0.57911641665207));
#35540=CARTESIAN_POINT('Ctrl Pts',(-0.0472702522103304,-0.142587432333395,
0.587016628516477));
#35541=CARTESIAN_POINT('Ctrl Pts',(0.0935959023848529,-0.117496636803883,
0.594916840380884));
#35542=CARTESIAN_POINT('Ctrl Pts',(0.149546622039777,0.0141936760548576,
0.60281705224529));
#35543=CARTESIAN_POINT('Ctrl Pts',(0.0698202860674386,0.133006692526806,
0.610717264109698));
#35544=CARTESIAN_POINT('Ctrl Pts',(-0.0732509165924606,0.13114860205821,
0.618617475974104));
#35545=CARTESIAN_POINT('Ctrl Pts',(-0.149864792769772,0.0103051681951267,
0.626517687838512));
#35546=CARTESIAN_POINT('Ctrl Pts',(-0.0905129510468744,-0.119887690344964,
0.634417899702917));
#35547=CARTESIAN_POINT('Ctrl Pts',(0.0509572998161204,-0.141311734116118,
0.642318111567325));
#35548=CARTESIAN_POINT('Ctrl Pts',(0.146196239617194,-0.0345298729398102,
0.650218323431731));
#35549=CARTESIAN_POINT('Ctrl Pts',(0.108797778021546,0.103579419292979,
0.658118535296138));
#35550=CARTESIAN_POINT('Ctrl Pts',(-0.0273081099235566,0.147715671937082,
0.666018747160545));
#35551=CARTESIAN_POINT('Ctrl Pts',(-0.138638553938667,0.0578360092433499,
0.673918959024952));
#35552=CARTESIAN_POINT('Ctrl Pts',(-0.124188351503322,-0.0845157142465292,
0.681819170889359));
#35553=CARTESIAN_POINT('Ctrl Pts',(0.00293246592609361,-0.150190057083441,
0.689719382753765));
#35554=CARTESIAN_POINT('Ctrl Pts',(0.127392786329333,-0.0796035840553634,
0.697619594618173));
#35555=CARTESIAN_POINT('Ctrl Pts',(0.136275249336903,0.0632037105184985,
0.705519806482578));
#35556=CARTESIAN_POINT('Ctrl Pts',(0.0215211879282666,0.148669065615609,
0.713420018346986));
#35557=CARTESIAN_POINT('Ctrl Pts',(-0.11275809824006,0.0992535333580773,
0.721320230211393));
#35558=CARTESIAN_POINT('Ctrl Pts',(-0.144736934218011,-0.0402103529878636,
0.729220442075799));
#35559=CARTESIAN_POINT('Ctrl Pts',(-0.0454023321324136,-0.143193159125993,
0.737120653940206));
#35560=CARTESIAN_POINT('Ctrl Pts',(0.0951238035943801,-0.116263126552003,
0.745020865804613));
#35561=CARTESIAN_POINT('Ctrl Pts',(0.149348307365949,0.0161473142389802,
0.75292107766902));
#35562=CARTESIAN_POINT('Ctrl Pts',(0.0680756769533821,0.133908008212467,
0.760821289533426));
#35563=CARTESIAN_POINT('Ctrl Pts',(-0.0749590118708499,0.130179872514462,
0.768721501397833));
#35564=CARTESIAN_POINT('Ctrl Pts',(-0.149986697268588,0.00834527665372157,
0.77662171326224));
#35565=CARTESIAN_POINT('Ctrl Pts',(-0.0889380612891912,-0.121060616221528,
0.784521925126647));
#35566=CARTESIAN_POINT('Ctrl Pts',(0.0528001464932815,-0.140633558934255,
0.792422136991054));
#35567=CARTESIAN_POINT('Ctrl Pts',(0.146635127365071,-0.0326158589327362,
0.80032234885546));
#35568=CARTESIAN_POINT('Ctrl Pts',(0.107434489766355,0.104992740843939,
0.808222560719866));
#35569=CARTESIAN_POINT('Ctrl Pts',(-0.0292366591003167,0.147346115160618,
0.816122772584275));
#35570=CARTESIAN_POINT('Ctrl Pts',(-0.139382797515625,0.0560187456986177,
0.82402298444868));
#35571=CARTESIAN_POINT('Ctrl Pts',(-0.123072840097892,-0.0861317506513214,
0.831923196313088));
#35572=CARTESIAN_POINT('Ctrl Pts',(0.00489524117472862,-0.150139108195811,
0.839823408177494));
#35573=CARTESIAN_POINT('Ctrl Pts',(0.128422915636328,-0.0779311130717641,
0.847723620041902));
#35574=CARTESIAN_POINT('Ctrl Pts',(0.135436566115076,0.0649789000904037,
0.855623831906308));
#35575=CARTESIAN_POINT('Ctrl Pts',(0.0195775850953746,0.148939165691587,
0.863524043770715));
#35576=CARTESIAN_POINT('Ctrl Pts',(-0.114048959254202,0.0977682841705676,
0.871424255635121));
#35577=CARTESIAN_POINT('Ctrl Pts',(-0.144193117111036,-0.0420935553533985,
0.879324467499528));
#35578=CARTESIAN_POINT('Ctrl Pts',(-0.0435377232159684,-0.143784562906888,
0.887224679363934));
#35579=CARTESIAN_POINT('Ctrl Pts',(0.09665649405843,-0.114990466423977,
0.895124891228342));
#35580=CARTESIAN_POINT('Ctrl Pts',(0.149084330818603,0.0180614574554272,
0.903025103092748));
#35581=CARTESIAN_POINT('Ctrl Pts',(0.0663971471312236,0.134857173710026,
0.910925314957155));
#35582=CARTESIAN_POINT('Ctrl Pts',(-0.0768143283784672,0.129046377235758,
0.918825526821562));
#35583=CARTESIAN_POINT('Ctrl Pts',(-0.125394707633209,0.0474984457471263,
0.924092334731166));
#35584=CARTESIAN_POINT('Ctrl Pts',(-0.127184992207232,0.00540996832212636,
0.926725738685969));
#35585=CARTESIAN_POINT('Ctrl Pts',(0.0684664424539458,-0.0958295198918399,
-1.80411241501588E-16));
#35586=CARTESIAN_POINT('Ctrl Pts',(0.100178663484274,-0.0731723787654901,
0.00263340395480208));
#35587=CARTESIAN_POINT('Ctrl Pts',(0.138824709433362,0.00568643248440989,
0.00790021186440659));
#35588=CARTESIAN_POINT('Ctrl Pts',(0.0709548212776815,0.119606362792331,
0.0158004237288134));
#35589=CARTESIAN_POINT('Ctrl Pts',(-0.0613439889848912,0.1246621346218,
0.0237006355932201));
#35590=CARTESIAN_POINT('Ctrl Pts',(-0.137959310498012,0.016793748463141,
0.0316008474576269));
#35591=CARTESIAN_POINT('Ctrl Pts',(-0.0894253929882274,-0.106402711804945,
0.0395010593220337));
#35592=CARTESIAN_POINT('Ctrl Pts',(0.040248222246223,-0.133016439153077,
0.0474012711864405));
#35593=CARTESIAN_POINT('Ctrl Pts',(0.133402197487182,-0.0389756054074351,
0.0553014830508473));
#35594=CARTESIAN_POINT('Ctrl Pts',(0.105528454455023,0.0904394425945055,
0.0632016949152541));
#35595=CARTESIAN_POINT('Ctrl Pts',(-0.0180877669633101,0.137795734956694,
0.0711019067796609));
#35596=CARTESIAN_POINT('Ctrl Pts',(-0.125293141551441,0.0601397387700418,
0.0790021186440675));
#35597=CARTESIAN_POINT('Ctrl Pts',(-0.118825896869129,-0.0720803414210898,
0.0869023305084746));
#35598=CARTESIAN_POINT('Ctrl Pts',(-0.0045529857407016,-0.138904079109577,
0.0948025423728811));
#35599=CARTESIAN_POINT('Ctrl Pts',(0.113850559027731,-0.0797068119457511,
0.102702754237288));
#35600=CARTESIAN_POINT('Ctrl Pts',(0.12896255920279,0.0518052156568057,
0.110602966101695));
#35601=CARTESIAN_POINT('Ctrl Pts',(0.0270724914422277,0.136316505597261,
0.118503177966102));
#35602=CARTESIAN_POINT('Ctrl Pts',(-0.0993792409180562,0.0971539201030866,
0.126403389830508));
#35603=CARTESIAN_POINT('Ctrl Pts',(-0.135668577197041,-0.0301521744798576,
0.134303601694915));
#35604=CARTESIAN_POINT('Ctrl Pts',(-0.0488717923313075,-0.130102508888041,
0.142203813559322));
#35605=CARTESIAN_POINT('Ctrl Pts',(0.0822642127117346,-0.112016585630158,
0.150104025423729));
#35606=CARTESIAN_POINT('Ctrl Pts',(0.138765526166673,0.00769705224861128,
0.158004237288135));
#35607=CARTESIAN_POINT('Ctrl Pts',(0.0693709963376258,0.12042749084372,
0.165904449152542));
#35608=CARTESIAN_POINT('Ctrl Pts',(-0.0629607791409001,0.123899379163224,
0.173804661016949));
#35609=CARTESIAN_POINT('Ctrl Pts',(-0.138171016229659,0.0149628234665004,
0.181704872881356));
#35610=CARTESIAN_POINT('Ctrl Pts',(-0.088024783135973,-0.107548841680175,
0.189605084745762));
#35611=CARTESIAN_POINT('Ctrl Pts',(0.0419824540321544,-0.132486185591528,
0.197505296610169));
#35612=CARTESIAN_POINT('Ctrl Pts',(0.133900861976353,-0.0372246554226585,
0.205405508474576));
#35613=CARTESIAN_POINT('Ctrl Pts',(0.10433692245731,0.0918091630494651,
0.213305720338983));
#35614=CARTESIAN_POINT('Ctrl Pts',(-0.0198873058616059,0.137548576426424,
0.221205932203389));
#35615=CARTESIAN_POINT('Ctrl Pts',(-0.126068658544878,0.0584962318650602,
0.229106144067797));
#35616=CARTESIAN_POINT('Ctrl Pts',(-0.117873476571655,-0.0736271643523165,
0.237006355932203));
#35617=CARTESIAN_POINT('Ctrl Pts',(-0.00273688716624997,-0.138951881091211,
0.24490656779661));
#35618=CARTESIAN_POINT('Ctrl Pts',(0.114882759277182,-0.0782116834669906,
0.252806779661017));
#35619=CARTESIAN_POINT('Ctrl Pts',(0.128274344207101,0.0534865256689417,
0.260706991525423));
#35620=CARTESIAN_POINT('Ctrl Pts',(0.0252882731449639,0.136658768658679,
0.26860720338983));
#35621=CARTESIAN_POINT('Ctrl Pts',(-0.100640733006032,0.0958465370784341,
0.276507415254237));
#35622=CARTESIAN_POINT('Ctrl Pts',(-0.13526284004966,-0.0319230310532247,
0.284407627118644));
#35623=CARTESIAN_POINT('Ctrl Pts',(-0.0471669369944997,-0.130730240818604,
0.292307838983051));
#35624=CARTESIAN_POINT('Ctrl Pts',(0.0837214480778729,-0.110931667893667,
0.300208050847457));
#35625=CARTESIAN_POINT('Ctrl Pts',(0.138653055169421,0.00951031556331505,
0.308108262711865));
#35626=CARTESIAN_POINT('Ctrl Pts',(0.0677908594821406,0.121324009085596,
0.316008474576271));
#35627=CARTESIAN_POINT('Ctrl Pts',(-0.0645749936433688,0.123065779182871,
0.323908686440678));
#35628=CARTESIAN_POINT('Ctrl Pts',(-0.138354802596303,0.0131553946526375,
0.331808898305084));
#35629=CARTESIAN_POINT('Ctrl Pts',(-0.0866114001779684,-0.108690299333199,
0.339709110169492));
#35630=CARTESIAN_POINT('Ctrl Pts',(0.0437107063235388,-0.131926077644361,
0.347609322033898));
#35631=CARTESIAN_POINT('Ctrl Pts',(0.134376016486386,-0.0354711432460098,
0.355509533898305));
#35632=CARTESIAN_POINT('Ctrl Pts',(0.103127892463174,0.0931651952503325,
0.363409745762711));
#35633=CARTESIAN_POINT('Ctrl Pts',(-0.0216836207666979,0.137276860396698,
0.371309957627119));
#35634=CARTESIAN_POINT('Ctrl Pts',(-0.126822541056414,0.0568432835955372,
0.379210169491525));
#35635=CARTESIAN_POINT('Ctrl Pts',(-0.116900962332481,-0.0751616977966073,
0.387110381355933));
#35636=CARTESIAN_POINT('Ctrl Pts',(-0.000920295459793275,-0.138975785179272,
0.395010593220339));
#35637=CARTESIAN_POINT('Ctrl Pts',(0.115895314901344,-0.0767032710765764,
0.402910805084745));
#35638=CARTESIAN_POINT('Ctrl Pts',(0.127564216682018,0.0551587384938402,
0.410811016949152));
#35639=CARTESIAN_POINT('Ctrl Pts',(0.0234997298595607,0.136977656960748,
0.418711228813559));
#35640=CARTESIAN_POINT('Ctrl Pts',(-0.10188502559814,0.0945227875636074,
0.426611440677966));
#35641=CARTESIAN_POINT('Ctrl Pts',(-0.134833990149192,-0.0336884388236675,
0.434511652542373));
#35642=CARTESIAN_POINT('Ctrl Pts',(-0.045454021205161,-0.13133563022352,
0.44241186440678));
#35643=CARTESIAN_POINT('Ctrl Pts',(0.085164376794762,-0.109827795821861,
0.450312076271186));
#35644=CARTESIAN_POINT('Ctrl Pts',(0.138516891217783,0.0113219546585138,
0.458212288135593));
#35645=CARTESIAN_POINT('Ctrl Pts',(0.0661991384108791,0.12219979494085,
0.4661125));
#35646=CARTESIAN_POINT('Ctrl Pts',(-0.0661781734963363,0.122211149911198,
0.474012711864406));
#35647=CARTESIAN_POINT('Ctrl Pts',(-0.138514946845716,0.0113457177056816,
0.481912923728814));
#35648=CARTESIAN_POINT('Ctrl Pts',(-0.0851832170082076,-0.109813183862691,
0.48981313559322));
#35649=CARTESIAN_POINT('Ctrl Pts',(0.0454314893010671,-0.131343426138561,
0.497713347457628));
#35650=CARTESIAN_POINT('Ctrl Pts',(0.134828208757446,-0.0337115697229769,
0.505613559322033));
#35651=CARTESIAN_POINT('Ctrl Pts',(0.10190123992053,0.0945053073249706,
0.513513771186441));
#35652=CARTESIAN_POINT('Ctrl Pts',(-0.0234762303627364,0.136981686432473,
0.521413983050847));
#35653=CARTESIAN_POINT('Ctrl Pts',(-0.127554752067971,0.0551806219139196,
0.529314194915254));
#35654=CARTESIAN_POINT('Ctrl Pts',(-0.115908471997041,-0.0766833875701887,
0.537214406779661));
#35655=CARTESIAN_POINT('Ctrl Pts',(0.000896453507092177,-0.13897594101512,
0.545114618644068));
#35656=CARTESIAN_POINT('Ctrl Pts',(0.116888066275103,-0.0751817515916976,
0.553014830508475));
#35657=CARTESIAN_POINT('Ctrl Pts',(0.126832290918542,0.0568215257651788,
0.560915042372882));
#35658=CARTESIAN_POINT('Ctrl Pts',(0.0217071709283622,0.137273138451102,
0.568815254237287));
#35659=CARTESIAN_POINT('Ctrl Pts',(-0.103111908025161,0.0931828859466119,
0.576715466101696));
#35660=CARTESIAN_POINT('Ctrl Pts',(-0.134382099747769,-0.0354480898964837,
0.584615677966101));
#35661=CARTESIAN_POINT('Ctrl Pts',(-0.0437333382095171,-0.131918576929031,
0.592515889830509));
#35662=CARTESIAN_POINT('Ctrl Pts',(0.0865927525795457,-0.108705156320324,
0.600416101694915));
#35663=CARTESIAN_POINT('Ctrl Pts',(0.138357057429181,0.0131316590523252,
0.608316313559322));
#35664=CARTESIAN_POINT('Ctrl Pts',(0.0645961051971127,0.123054699232873,
0.616216525423729));
#35665=CARTESIAN_POINT('Ctrl Pts',(-0.0677700447892944,0.121335637135943,
0.624116737288135));
#35666=CARTESIAN_POINT('Ctrl Pts',(-0.138651421590416,0.00953410199670787,
0.632016949152542));
#35667=CARTESIAN_POINT('Ctrl Pts',(-0.0837404776869246,-0.110917303459374,
0.639917161016949));
#35668=CARTESIAN_POINT('Ctrl Pts',(0.0471445089225743,-0.130738330601145,
0.647817372881356));
#35669=CARTESIAN_POINT('Ctrl Pts',(0.135257361515437,-0.0319462355497722,
0.655717584745763));
#35670=CARTESIAN_POINT('Ctrl Pts',(0.100657174442164,0.0958292702846084,
0.66361779661017));
#35671=CARTESIAN_POINT('Ctrl Pts',(-0.0252648283287276,0.136663104967713,
0.671518008474576));
#35672=CARTESIAN_POINT('Ctrl Pts',(-0.128265166458182,0.0535085309397911,
0.679418220338983));
#35673=CARTESIAN_POINT('Ctrl Pts',(-0.114896175163422,-0.0781919736479584,
0.68731843220339));
#35674=CARTESIAN_POINT('Ctrl Pts',(0.00271304928865532,-0.138952348570324,
0.695218644067796));
#35675=CARTESIAN_POINT('Ctrl Pts',(0.117860843754417,-0.0736473850127282,
0.703118855932203));
#35676=CARTESIAN_POINT('Ctrl Pts',(0.126078691992566,0.0584746033489104,
0.711019067796611));
#35677=CARTESIAN_POINT('Ctrl Pts',(0.0199109026571207,0.137545162630623,
0.718919279661016));
#35678=CARTESIAN_POINT('Ctrl Pts',(-0.104321170622334,0.0918270612038291,
0.726819491525424));
#35679=CARTESIAN_POINT('Ctrl Pts',(-0.133907246092115,-0.0372016836068011,
0.73471970338983));
#35680=CARTESIAN_POINT('Ctrl Pts',(-0.0420051819866054,-0.132478981273086,
0.742619915254238));
#35681=CARTESIAN_POINT('Ctrl Pts',(0.0880063312515965,-0.107563941317063,
0.750520127118644));
#35682=CARTESIAN_POINT('Ctrl Pts',(0.1381735813042,0.0149391196739674,0.758420338983051));
#35683=CARTESIAN_POINT('Ctrl Pts',(0.0629820334107182,0.123888575547709,
0.766320550847457));
#35684=CARTESIAN_POINT('Ctrl Pts',(-0.069350334823955,0.120439391087123,
0.774220762711865));
#35685=CARTESIAN_POINT('Ctrl Pts',(-0.138764204798178,0.00772085591431189,
0.78212097457627));
#35686=CARTESIAN_POINT('Ctrl Pts',(-0.0822834263027052,-0.112002467207309,
0.790021186440679));
#35687=CARTESIAN_POINT('Ctrl Pts',(0.0488494678181175,-0.130110898691923,
0.797921398305084));
#35688=CARTESIAN_POINT('Ctrl Pts',(0.135663410254684,-0.0301754342953877,
0.805821610169492));
#35689=CARTESIAN_POINT('Ctrl Pts',(0.0993958918478579,0.0971368425207782,
0.813721822033898));
#35690=CARTESIAN_POINT('Ctrl Pts',(-0.0270490771841315,0.136321199631122,
0.821622033898304));
#35691=CARTESIAN_POINT('Ctrl Pts',(-0.128953723310312,0.0518272409635079,
0.829522245762713));
#35692=CARTESIAN_POINT('Ctrl Pts',(-0.113864129949169,-0.0796870929533346,
0.837422457627119));
#35693=CARTESIAN_POINT('Ctrl Pts',(0.00452896330992775,-0.13890521184416,
0.845322669491525));
#35694=CARTESIAN_POINT('Ctrl Pts',(0.118813895436517,-0.0721000537472655,
0.853222881355933));
#35695=CARTESIAN_POINT('Ctrl Pts',(0.125302761776928,0.0601169674638447,
0.861123093220339));
#35696=CARTESIAN_POINT('Ctrl Pts',(0.0181127265090936,0.137795052940508,
0.869023305084746));
#35697=CARTESIAN_POINT('Ctrl Pts',(-0.105515445217312,0.0904529431907972,
0.876923516949153));
#35698=CARTESIAN_POINT('Ctrl Pts',(-0.133404119149664,-0.0389439786468707,
0.88482372881356));
#35699=CARTESIAN_POINT('Ctrl Pts',(-0.0402800891732956,-0.133026134299755,
0.892723940677965));
#35700=CARTESIAN_POINT('Ctrl Pts',(0.0894243408305711,-0.10638650575871,
0.900624152542373));
#35701=CARTESIAN_POINT('Ctrl Pts',(0.137929356340621,0.0167100404698593,
0.908524364406779));
#35702=CARTESIAN_POINT('Ctrl Pts',(0.0614290966487016,0.124766721395902,
0.916424576271187));
#35703=CARTESIAN_POINT('Ctrl Pts',(-0.0710668305166857,0.11939070761148,
0.924324788135593));
#35704=CARTESIAN_POINT('Ctrl Pts',(-0.116012267804409,0.0439444575637681,
0.929591596045198));
#35705=CARTESIAN_POINT('Ctrl Pts',(-0.11766859746431,0.00500517689817995,
0.932225));
#35706=CARTESIAN_POINT('',(0.0684664424539459,-0.0958295198918398,0.));
#35707=CARTESIAN_POINT('Ctrl Pts',(0.0684664424539458,-0.0958295198918399,
-1.80411241501588E-16));
#35708=CARTESIAN_POINT('Ctrl Pts',(0.100178663484274,-0.0731723787654901,
0.00263340395480208));
#35709=CARTESIAN_POINT('Ctrl Pts',(0.138824709433362,0.00568643248440989,
0.00790021186440659));
#35710=CARTESIAN_POINT('Ctrl Pts',(0.0709548212776815,0.119606362792331,
0.0158004237288134));
#35711=CARTESIAN_POINT('Ctrl Pts',(-0.0613439889848912,0.1246621346218,
0.0237006355932201));
#35712=CARTESIAN_POINT('Ctrl Pts',(-0.115532083261749,0.0483695320037083,
0.0292882571924104));
#35713=CARTESIAN_POINT('Ctrl Pts',(-0.117931878255507,0.00481801833454289,
0.0322424748367984));
#35714=CARTESIAN_POINT('Ctrl Pts',(-0.117896184020664,8.43438525024954E-5,
0.0325632885263842));
#35715=CARTESIAN_POINT('Ctrl Pts',(0.0635538308725813,0.132076982143461,
2.60208521396521E-18));
#35716=CARTESIAN_POINT('Ctrl Pts',(0.0672186180130936,0.129896798349724,
2.66126088244575E-18));
#35717=CARTESIAN_POINT('Ctrl Pts',(0.0707747244255609,0.12755097155874,
-6.59520968701772E-18));
#35718=CARTESIAN_POINT('Ctrl Pts',(0.0742090918971922,0.125038932664582,
-4.55364912443912E-18));
#35719=CARTESIAN_POINT('Ctrl Pts',(0.080224006754745,0.120639374320277,
-2.50552574932592E-18));
#35720=CARTESIAN_POINT('Ctrl Pts',(0.0858662145577153,0.115730301363634,
1.59702880631994E-17));
#35721=CARTESIAN_POINT('Ctrl Pts',(0.0911015321007297,0.110378142457541,
2.25514051876985E-17));
#35722=CARTESIAN_POINT('Ctrl Pts',(0.0937720491785869,0.107648025011046,
2.59084099019214E-17));
#35723=CARTESIAN_POINT('Ctrl Pts',(0.0963357255281008,0.104802798728268,
-1.64960383635052E-18));
#35724=CARTESIAN_POINT('Ctrl Pts',(0.0987794574485338,0.101861414187154,
-4.33680868994202E-19));
#35725=CARTESIAN_POINT('Ctrl Pts',(0.10293496714428,0.0968596577026072,
1.63396805676607E-18));
#35726=CARTESIAN_POINT('Ctrl Pts',(0.106751261320725,0.0915729561578743,
3.03784192455847E-17));
#35727=CARTESIAN_POINT('Ctrl Pts',(0.110204305377691,0.08604549563647,2.73218947466347E-17));
#35728=CARTESIAN_POINT('Ctrl Pts',(0.111935557805272,0.0832741931890737,
2.57894452987073E-17));
#35729=CARTESIAN_POINT('Ctrl Pts',(0.113575375365209,0.0804423219653594,
5.7323915193469E-18));
#35730=CARTESIAN_POINT('Ctrl Pts',(0.115119932079619,0.077555293108205,
9.54097911787244E-18));
#35731=CARTESIAN_POINT('Ctrl Pts',(0.116773389847001,0.0744647103902093,
1.36180963184181E-17));
#35732=CARTESIAN_POINT('Ctrl Pts',(0.118313357645953,0.0713188633723711,
-9.33067413676427E-18));
#35733=CARTESIAN_POINT('Ctrl Pts',(0.119735247150481,0.0681278580844796,
-4.33680868994202E-18));
#35734=CARTESIAN_POINT('Ctrl Pts',(0.123742606948277,0.059134538797346,
9.73757301374157E-18));
#35735=CARTESIAN_POINT('Ctrl Pts',(0.126819919828835,0.0497749725291024,
2.44496492997929E-17));
#35736=CARTESIAN_POINT('Ctrl Pts',(0.128866909768778,0.040203097865136,
1.21430643318376E-17));
#35737=CARTESIAN_POINT('Ctrl Pts',(0.129678753995803,0.0364068548860612,
7.26222453596554E-18));
#35738=CARTESIAN_POINT('Ctrl Pts',(0.130327963181773,0.0325772120613575,
7.16378425601151E-18));
#35739=CARTESIAN_POINT('Ctrl Pts',(0.130805907644987,0.0287241348669356,
3.46944695195361E-18));
#35740=CARTESIAN_POINT('Ctrl Pts',(0.131145551201884,0.0259860074399329,
8.44125478642762E-19));
#35741=CARTESIAN_POINT('Ctrl Pts',(0.131398222957245,0.023238193513084,
1.89851870451249E-17));
#35742=CARTESIAN_POINT('Ctrl Pts',(0.131560851492827,0.0204930145081475,
1.56125112837913E-17));
#35743=CARTESIAN_POINT('Ctrl Pts',(0.131856680066531,0.0154994112226654,
9.47746335708933E-18));
#35744=CARTESIAN_POINT('Ctrl Pts',(0.131855937211452,0.0105061465300757,
1.21882171850414E-17));
#35745=CARTESIAN_POINT('Ctrl Pts',(0.131544012134307,0.00553446959878105,
1.73472347597681E-17));
#35746=CARTESIAN_POINT('Ctrl Pts',(0.131183605376493,-0.00020994178392047,
2.50428281171472E-17));
#35747=CARTESIAN_POINT('Ctrl Pts',(0.130407809774817,-0.00592569963173127,
6.69723701682335E-18));
#35748=CARTESIAN_POINT('Ctrl Pts',(0.129236296320737,-0.0115776207498215,
6.93889390390723E-18));
#35749=CARTESIAN_POINT('Ctrl Pts',(0.128494418700647,-0.0151567804883794,
7.09192657770507E-18));
#35750=CARTESIAN_POINT('Ctrl Pts',(0.127593716302061,-0.0187102876496501,
1.81123981287573E-17));
#35751=CARTESIAN_POINT('Ctrl Pts',(0.126538054496122,-0.0222283432593045,
1.73472347597681E-17));
#35752=CARTESIAN_POINT('Ctrl Pts',(0.125628643409289,-0.0252590096692432,
1.66880766401104E-17));
#35753=CARTESIAN_POINT('Ctrl Pts',(0.124606340862147,-0.0282558643089978,
1.76789329645073E-17));
#35754=CARTESIAN_POINT('Ctrl Pts',(0.123476980164864,-0.0312080791264482,
1.38777878078145E-17));
#35755=CARTESIAN_POINT('Ctrl Pts',(0.120897724271906,-0.0379504046593839,
5.19665867965098E-18));
#35756=CARTESIAN_POINT('Ctrl Pts',(0.117758352703866,-0.0444696874516502,
3.23003755723985E-17));
#35757=CARTESIAN_POINT('Ctrl Pts',(0.114097802370374,-0.050694248232474,
2.94902990916057E-17));
#35758=CARTESIAN_POINT('Ctrl Pts',(0.11100985408088,-0.0559451313142133,
2.71197891759751E-17));
#35759=CARTESIAN_POINT('Ctrl Pts',(0.107550620981395,-0.0609862743257036,
5.91633367061488E-18));
#35760=CARTESIAN_POINT('Ctrl Pts',(0.103737131336817,-0.0657661572550731,
2.08166817117217E-17));
#35761=CARTESIAN_POINT('Ctrl Pts',(0.10192691642303,-0.0680351067400168,
2.78896869532561E-17));
#35762=CARTESIAN_POINT('Ctrl Pts',(0.10004287794431,-0.0702374362624183,
3.79094719020518E-18));
#35763=CARTESIAN_POINT('Ctrl Pts',(0.098088083467589,-0.0723681596371707,
3.46944695195361E-18));
#35764=CARTESIAN_POINT('Ctrl Pts',(0.092197190805992,-0.078789224788366,
2.50058632912494E-18));
#35765=CARTESIAN_POINT('Ctrl Pts',(0.0856641330198359,-0.0845647204793276,
-6.81778632605364E-18));
#35766=CARTESIAN_POINT('Ctrl Pts',(0.0785460746715851,-0.0895442682019542,
-6.93889390390723E-18));
#35767=CARTESIAN_POINT('Ctrl Pts',(0.0753062120776356,-0.0918107641495869,
-6.9940173507989E-18));
#35768=CARTESIAN_POINT('Ctrl Pts',(0.0719448689431282,-0.0939117521002605,
3.85531108019535E-18));
#35769=CARTESIAN_POINT('Ctrl Pts',(0.068466442453948,-0.0958295198918383,
3.46944695195361E-18));
#35770=CARTESIAN_POINT('Ctrl Pts',(-0.00156268643912563,0.146080787864432,
0.903650000000001));
#35771=CARTESIAN_POINT('Ctrl Pts',(0.0213629386064158,0.146372019480346,
0.902408930776365));
#35772=CARTESIAN_POINT('Ctrl Pts',(0.0443374951530579,0.14156774719521,
0.901167861552729));
#35773=CARTESIAN_POINT('Ctrl Pts',(0.0647363246762687,0.131545720210662,
0.899926792329093));
#35774=CARTESIAN_POINT('Ctrl Pts',(0.108020258655701,0.110280149367703,
0.897293388374291));
#35775=CARTESIAN_POINT('Ctrl Pts',(0.139707269215135,0.0655222203971333,
0.894659984419488));
#35776=CARTESIAN_POINT('Ctrl Pts',(0.145505194618115,0.0176494760483365,
0.892026580464686));
#35777=CARTESIAN_POINT('Ctrl Pts',(0.151303120021096,-0.0302232683004618,
0.889393176509884));
#35778=CARTESIAN_POINT('Ctrl Pts',(0.131211960267621,-0.0812108280274876,
0.886759772555081));
#35779=CARTESIAN_POINT('Ctrl Pts',(0.0943040817549728,-0.112221779952107,
0.884126368600279));
#35780=CARTESIAN_POINT('Ctrl Pts',(0.0573962032423251,-0.143232731876727,
0.881492964645477));
#35781=CARTESIAN_POINT('Ctrl Pts',(0.0036716059705044,-0.15426707599894,
0.878859560690674));
#35782=CARTESIAN_POINT('Ctrl Pts',(-0.0424770462874833,-0.140299462834264,
0.876226156735872));
#35783=CARTESIAN_POINT('Ctrl Pts',(-0.0886256985454704,-0.126331849669587,
0.87359275278107));
#35784=CARTESIAN_POINT('Ctrl Pts',(-0.127198405789625,-0.0873622792180203,
0.870959348826268));
#35785=CARTESIAN_POINT('Ctrl Pts',(-0.140708905127403,-0.0410788815094769,
0.868325944871466));
#35786=CARTESIAN_POINT('Ctrl Pts',(-0.144574583355673,-0.027836090226996,
0.867572464775741));
#35787=CARTESIAN_POINT('Ctrl Pts',(-0.146388495105525,-0.0139945382267495,
0.866818984680017));
#35788=CARTESIAN_POINT('Ctrl Pts',(-0.146273246343463,-0.000123611542196964,
0.866065504584292));
#35789=CARTESIAN_POINT('Origin',(0.,0.,-0.0924367114736152));
#35790=CARTESIAN_POINT('',(-0.0684664424539439,-0.0958295198918412,0.));
#35791=CARTESIAN_POINT('Ctrl Pts',(-0.0686121729278148,-0.0959472995825297,
4.17959937493162E-17));
#35792=CARTESIAN_POINT('Ctrl Pts',(-0.0396139635805184,-0.116414379406814,
0.00240676188548629));
#35793=CARTESIAN_POINT('Ctrl Pts',(0.042075530384929,-0.130578648252184,
0.00744886483747836));
#35794=CARTESIAN_POINT('Ctrl Pts',(0.133186295059001,-0.0398205273591854,
0.0151263088559762));
#35795=CARTESIAN_POINT('Ctrl Pts',(0.106043485420733,0.0899039768168324,
0.0230323320554937));
#35796=CARTESIAN_POINT('Ctrl Pts',(-0.0174538572390982,0.137906280269365,
0.0309383552550111));
#35797=CARTESIAN_POINT('Ctrl Pts',(-0.105510720744521,0.0746991700253994,
0.0374064817277185));
#35798=CARTESIAN_POINT('Ctrl Pts',(-0.11763008980369,0.0178164887288322,
0.0412392671339201));
#35799=CARTESIAN_POINT('Ctrl Pts',(-0.117591431864639,2.92794590778002E-5,
0.0424367114736158));
#35800=CARTESIAN_POINT('Origin',(0.,0.,0.));
#35801=CARTESIAN_POINT('Ctrl Pts',(-0.0510216505388444,0.106149619882937,
-0.0164977839420935));
#35802=CARTESIAN_POINT('Ctrl Pts',(-0.0861748725546967,0.0892529469510397,
-0.0138624428755877));
#35803=CARTESIAN_POINT('Ctrl Pts',(-0.137790539141881,0.0181049606281334,
-0.0085917607425761));
#35804=CARTESIAN_POINT('Ctrl Pts',(-0.0902797247787074,-0.10582739645577,
-0.000685737543058663));
#35805=CARTESIAN_POINT('Ctrl Pts',(0.0393629057248093,-0.133280773711466,
0.00722028565645879));
#35806=CARTESIAN_POINT('Ctrl Pts',(0.133186295059001,-0.0398205273591854,
0.0151263088559762));
#35807=CARTESIAN_POINT('Ctrl Pts',(0.106043485420733,0.0899039768168324,
0.0230323320554937));
#35808=CARTESIAN_POINT('Ctrl Pts',(-0.0174538572390982,0.137906280269365,
0.0309383552550111));
#35809=CARTESIAN_POINT('Ctrl Pts',(-0.125086200033906,0.0606479146403327,
0.0388443784545286));
#35810=CARTESIAN_POINT('Ctrl Pts',(-0.119084788854313,-0.0717206569949895,
0.046750401654046));
#35811=CARTESIAN_POINT('Ctrl Pts',(-0.00489492837772915,-0.138925734589418,
0.0546564248535634));
#35812=CARTESIAN_POINT('Ctrl Pts',(0.113740629398734,-0.0799231888543136,
0.062562448053081));
#35813=CARTESIAN_POINT('Ctrl Pts',(0.129045816271948,0.0516898037714297,
0.0704684712525983));
#35814=CARTESIAN_POINT('Ctrl Pts',(0.0271151839788463,0.136342686033388,
0.0783744944521158));
#35815=CARTESIAN_POINT('Ctrl Pts',(-0.0994488545192835,0.097131556418157,
0.0862805176516332));
#35816=CARTESIAN_POINT('Ctrl Pts',(-0.135665746467832,-0.0303218706918135,
0.0941865408511506));
#35817=CARTESIAN_POINT('Ctrl Pts',(-0.0486330432543111,-0.130228357167641,
0.102092564050668));
#35818=CARTESIAN_POINT('Ctrl Pts',(0.0825817545836372,-0.111825131042891,
0.109998587250186));
#35819=CARTESIAN_POINT('Ctrl Pts',(0.138772738128538,0.00816897019039422,
0.117904610449703));
#35820=CARTESIAN_POINT('Ctrl Pts',(0.0688915313895657,0.120741708772585,
0.12581063364922));
#35821=CARTESIAN_POINT('Ctrl Pts',(-0.0635762130827019,0.123623095373164,
0.133716656848738));
#35822=CARTESIAN_POINT('Ctrl Pts',(-0.138286275523292,0.014195432572335,
0.141622680048255));
#35823=CARTESIAN_POINT('Ctrl Pts',(-0.0873660952430369,-0.108128486159945,
0.149528703247773));
#35824=CARTESIAN_POINT('Ctrl Pts',(0.0429243879661372,-0.132219897211806,
0.15743472644729));
#35825=CARTESIAN_POINT('Ctrl Pts',(0.134218946443888,-0.0361922458912883,
0.165340749646808));
#35826=CARTESIAN_POINT('Ctrl Pts',(0.103578348063976,0.0927153171784346,
0.173246772846325));
#35827=CARTESIAN_POINT('Ctrl Pts',(-0.0211610525014389,0.137392918706172,
0.181152796045843));
#35828=CARTESIAN_POINT('Ctrl Pts',(-0.126676071448117,0.0572518747851005,
0.18905881924536));
#35829=CARTESIAN_POINT('Ctrl Pts',(-0.117108480713923,-0.074901321664099,
0.196964842444878));
#35830=CARTESIAN_POINT('Ctrl Pts',(-0.00115024004832317,-0.139008205490464,
0.204870865644395));
#35831=CARTESIAN_POINT('Ctrl Pts',(0.115852970087698,-0.0768289890996742,
0.212776888843912));
#35832=CARTESIAN_POINT('Ctrl Pts',(0.127606135899372,0.055147786219953,
0.22068291204343));
#35833=CARTESIAN_POINT('Ctrl Pts',(0.0234317475993789,0.137023930205902,
0.228588935242947));
#35834=CARTESIAN_POINT('Ctrl Pts',(-0.102029902232137,0.0944166473397004,
0.236494958442465));
#35835=CARTESIAN_POINT('Ctrl Pts',(-0.134799481036655,-0.0339662208175969,
0.244400981641982));
#35836=CARTESIAN_POINT('Ctrl Pts',(-0.0451064993838265,-0.131491474848312,
0.252307004841499));
#35837=CARTESIAN_POINT('Ctrl Pts',(0.0855648107118161,-0.1095594241143,
0.260213028041017));
#35838=CARTESIAN_POINT('Ctrl Pts',(0.138502247321704,0.0119051136596435,
0.268119051240535));
#35839=CARTESIAN_POINT('Ctrl Pts',(0.0656132363391791,0.122554100141606,
0.276025074440052));
#35840=CARTESIAN_POINT('Ctrl Pts',(-0.066884052510702,0.121865203254083,
0.283931097639569));
#35841=CARTESIAN_POINT('Ctrl Pts',(-0.138618553097211,0.010464271673199,
0.291837120839087));
#35842=CARTESIAN_POINT('Ctrl Pts',(-0.0844209446825288,-0.110443235842333,
0.299743144038604));
#35843=CARTESIAN_POINT('Ctrl Pts',(0.046471358419155,-0.131015331511595,
0.307649167238122));
#35844=CARTESIAN_POINT('Ctrl Pts',(0.135145386671506,-0.0325626888604762,
0.315555190437639));
#35845=CARTESIAN_POINT('Ctrl Pts',(0.101042606300054,0.0954724879559945,
0.323461213637157));
#35846=CARTESIAN_POINT('Ctrl Pts',(-0.0248553070174182,0.136772869961425,
0.331367236836674));
#35847=CARTESIAN_POINT('Ctrl Pts',(-0.12817268430534,0.0538179081940093,
0.339273260036191));
#35848=CARTESIAN_POINT('Ctrl Pts',(-0.115047809886908,-0.0780295180341452,
0.347179283235709));
#35849=CARTESIAN_POINT('Ctrl Pts',(0.00259563734382704,-0.138988729439456,
0.355085306435226));
#35850=CARTESIAN_POINT('Ctrl Pts',(0.117881001348277,-0.0736795342380946,
0.362991329634744));
#35851=CARTESIAN_POINT('Ctrl Pts',(0.12607389627645,0.0585660048329233,
0.370897352834261));
#35852=CARTESIAN_POINT('Ctrl Pts',(0.0197312453245754,0.137605531147394,
0.378803376033779));
#35853=CARTESIAN_POINT('Ctrl Pts',(-0.104536836829869,0.0916332580999962,
0.386709399233296));
#35854=CARTESIAN_POINT('Ctrl Pts',(-0.133835349354862,-0.0375859482716227,
0.394615422432814));
#35855=CARTESIAN_POINT('Ctrl Pts',(-0.0415471952570256,-0.13265909245389,
0.40252144563233));
#35856=CARTESIAN_POINT('Ctrl Pts',(0.0884857325734624,-0.107214175253801,
0.410427468831849));
#35857=CARTESIAN_POINT('Ctrl Pts',(0.138131189387156,0.0156326185555932,
0.418333492031365));
#35858=CARTESIAN_POINT('Ctrl Pts',(0.062287297122381,0.124277499418049,
0.426239515230884));
#35859=CARTESIAN_POINT('Ctrl Pts',(-0.0701433255283678,0.120018824057881,
0.4341455384304));
#35860=CARTESIAN_POINT('Ctrl Pts',(-0.138850177307333,0.00672551158926456,
0.442051561629919));
#35861=CARTESIAN_POINT('Ctrl Pts',(-0.0814144942465354,-0.11267779005197,
0.449957584829435));
#35862=CARTESIAN_POINT('Ctrl Pts',(0.0499845850166584,-0.129715633233345,
0.457863608028953));
#35863=CARTESIAN_POINT('Ctrl Pts',(0.135973695209673,-0.0289094872912353,
0.465769631228471));
#35864=CARTESIAN_POINT('Ctrl Pts',(0.0984334954810092,0.0981603342078928,
0.473675654427988));
#35865=CARTESIAN_POINT('Ctrl Pts',(-0.0285315135918273,0.136053507770195,
0.481581677627505));
#35866=CARTESIAN_POINT('Ctrl Pts',(-0.129576228451988,0.0503448633385094,
0.489487700827023));
#35867=CARTESIAN_POINT('Ctrl Pts',(-0.112903600569895,-0.0811010556205559,
0.49739372402654));
#35868=CARTESIAN_POINT('Ctrl Pts',(0.00633962999064621,-0.138868330932566,
0.505299747226058));
#35869=CARTESIAN_POINT('Ctrl Pts',(0.119823436886959,-0.0704765792090683,
0.513205770425575));
#35870=CARTESIAN_POINT('Ctrl Pts',(0.124450111907394,0.0619416975118724,
0.521111793625093));
#35871=CARTESIAN_POINT('Ctrl Pts',(0.0160164158031762,0.138087213996209,
0.52901781682461));
#35872=CARTESIAN_POINT('Ctrl Pts',(-0.106967865166254,0.0887833321417318,
0.536923840024128));
#35873=CARTESIAN_POINT('Ctrl Pts',(-0.132774037183017,-0.0411783838262002,
0.544829863223645));
#35874=CARTESIAN_POINT('Ctrl Pts',(-0.0379577228913647,-0.133730383672961,
0.552735886423163));
#35875=CARTESIAN_POINT('Ctrl Pts',(0.0913424031974019,-0.104791076063462,
0.56064190962268));
#35876=CARTESIAN_POINT('Ctrl Pts',(0.137659831668342,0.0193487722984857,
0.568547932822197));
#35877=CARTESIAN_POINT('Ctrl Pts',(0.0589161298691768,0.125910658348106,
0.576453956021715));
#35878=CARTESIAN_POINT('Ctrl Pts',(-0.0733516660922674,0.11808529682354,
0.584359979221232));
#35879=CARTESIAN_POINT('Ctrl Pts',(-0.138980979661871,0.00298186797856315,
0.59226600242075));
#35880=CARTESIAN_POINT('Ctrl Pts',(-0.0783489271385985,-0.114830526693234,
0.600172025620267));
#35881=CARTESIAN_POINT('Ctrl Pts',(0.0534615168199478,-0.12832174587234,
0.608078048819785));
#35882=CARTESIAN_POINT('Ctrl Pts',(0.136703270562712,-0.0252352939724056,
0.615984072019302));
#35883=CARTESIAN_POINT('Ctrl Pts',(0.0957529101571512,0.100776904302778,
0.623890095218819));
#35884=CARTESIAN_POINT('Ctrl Pts',(-0.0321870028708045,0.135235354440354,
0.631796118418337));
#35885=CARTESIAN_POINT('Ctrl Pts',(-0.130885684740464,0.0468352620836017,
0.639702141617854));
#35886=CARTESIAN_POINT('Ctrl Pts',(-0.110677409719003,-0.0841137041290149,
0.647608164817372));
#35887=CARTESIAN_POINT('Ctrl Pts',(0.0100790193068892,-0.138647097388359,
0.655514188016889));
#35888=CARTESIAN_POINT('Ctrl Pts',(0.121678866262096,-0.0672224497442505,
0.663420211216407));
#35889=CARTESIAN_POINT('Ctrl Pts',(0.122735961854403,0.0652724131012164,
0.671326234415924));
#35890=CARTESIAN_POINT('Ctrl Pts',(0.0122899564463577,0.138468628991968,
0.679232257615441));
#35891=CARTESIAN_POINT('Ctrl Pts',(-0.109321222024174,0.0858689388531973,
0.687138280814959));
#35892=CARTESIAN_POINT('Ctrl Pts',(-0.131616315159593,-0.0447409189438641,
0.695044304014476));
#35893=CARTESIAN_POINT('Ctrl Pts',(-0.0343406886760894,-0.134704570618338,
0.702950327213994));
#35894=CARTESIAN_POINT('Ctrl Pts',(0.0941327483034478,-0.102291886006113,
0.710856350413511));
#35895=CARTESIAN_POINT('Ctrl Pts',(0.137088516418336,0.0230508765206803,
0.718762373613029));
#35896=CARTESIAN_POINT('Ctrl Pts',(0.0555021824679276,0.127452391053421,
0.726668396812546));
#35897=CARTESIAN_POINT('Ctrl Pts',(-0.0765067445957343,0.116066025541209,
0.734574420012063));
#35898=CARTESIAN_POINT('Ctrl Pts',(-0.139010865120405,-0.000763940859230431,
0.742480443211581));
#35899=CARTESIAN_POINT('Ctrl Pts',(-0.0752264694457675,-0.116899882557203,
0.750386466411098));
#35900=CARTESIAN_POINT('Ctrl Pts',(0.0568996293847587,-0.126834681679914,
0.758292489610617));
#35901=CARTESIAN_POINT('Ctrl Pts',(0.137333582544999,-0.0215427765762162,
0.766198512810132));
#35902=CARTESIAN_POINT('Ctrl Pts',(0.0930027975645983,0.103320297856606,
0.774104536009652));
#35903=CARTESIAN_POINT('Ctrl Pts',(-0.035819122070238,0.13431900488649,
0.782010559209168));
#35904=CARTESIAN_POINT('Ctrl Pts',(-0.13210009942588,0.0432916512297215,
0.789916582408685));
#35905=CARTESIAN_POINT('Ctrl Pts',(-0.108370859366875,-0.0870652729953126,
0.797822605608204));
#35906=CARTESIAN_POINT('Ctrl Pts',(0.0138111005924944,-0.138325195186183,
0.80572862880772));
#35907=CARTESIAN_POINT('Ctrl Pts',(0.123445922182148,-0.0639194978340518,
0.813634652007238));
#35908=CARTESIAN_POINT('Ctrl Pts',(0.120932728835538,0.0685557124046954,
0.821540675206756));
#35909=CARTESIAN_POINT('Ctrl Pts',(0.0085545008581314,0.138749538494654,
0.829446698406273));
#35910=CARTESIAN_POINT('Ctrl Pts',(-0.111595061352101,0.0828921197631381,
0.837352721605791));
#35911=CARTESIAN_POINT('Ctrl Pts',(-0.130363284584795,-0.0482708249720888,
0.845258744805308));
#35912=CARTESIAN_POINT('Ctrl Pts',(-0.0306982239304521,-0.135581215292453,
0.853164768004825));
#35913=CARTESIAN_POINT('Ctrl Pts',(0.0968538014257187,-0.0997179081430208,
0.861070791204343));
#35914=CARTESIAN_POINT('Ctrl Pts',(0.136419444538435,0.0267352712365894,
0.86897681440386));
#35915=CARTESIAN_POINT('Ctrl Pts',(0.0520445414416943,0.128903423908239,
0.876882837603378));
#35916=CARTESIAN_POINT('Ctrl Pts',(-0.0795998263876522,0.113958970288921,
0.884788860802895));
#35917=CARTESIAN_POINT('Ctrl Pts',(-0.138952053011478,-0.00450253390371847,
0.892694884002413));
#35918=CARTESIAN_POINT('Ctrl Pts',(-0.0720261204166176,-0.118897020856024,
0.90060090720193));
#35919=CARTESIAN_POINT('Ctrl Pts',(0.0602520802431792,-0.125231345176025,
0.908506930401448));
#35920=CARTESIAN_POINT('Ctrl Pts',(0.137949690524835,-0.017881538827179,
0.916412953600965));
#35921=CARTESIAN_POINT('Ctrl Pts',(0.0900118016872842,0.105886249500893,
0.924318976800482));
#35922=CARTESIAN_POINT('Ctrl Pts',(0.00399973323748277,0.12400080376067,
0.929589658933494));
#35923=CARTESIAN_POINT('Ctrl Pts',(-0.0334019664626807,0.112939183906322,
0.932225));
#35924=CARTESIAN_POINT('Ctrl Pts',(-0.0551480035117367,0.114734422509853,
-0.0109985226280624));
#35925=CARTESIAN_POINT('Ctrl Pts',(-0.0931442265014884,0.0964712387762041,
-0.00836318156155655));
#35926=CARTESIAN_POINT('Ctrl Pts',(-0.148934286841532,0.0195691911522949,
-0.00309249942854491));
#35927=CARTESIAN_POINT('Ctrl Pts',(-0.097581056797534,-0.114386139408358,
0.00481352377097251));
#35928=CARTESIAN_POINT('Ctrl Pts',(0.0425463629697991,-0.144059796166161,
0.01271954697049));
#35929=CARTESIAN_POINT('Ctrl Pts',(0.143957676595294,-0.0430409945474375,
0.0206255701700074));
#35930=CARTESIAN_POINT('Ctrl Pts',(0.114619704470892,0.0971749203887298,
0.0285315933695248));
#35931=CARTESIAN_POINT('Ctrl Pts',(-0.0188654300703636,0.149059388480494,
0.0364376165690423));
#35932=CARTESIAN_POINT('Ctrl Pts',(-0.13520249003877,0.065552787380297,
0.0443436397685597));
#35933=CARTESIAN_POINT('Ctrl Pts',(-0.128715717437097,-0.0775210327782809,
0.0522496629680772));
#35934=CARTESIAN_POINT('Ctrl Pts',(-0.0052908035023142,-0.150161290708834,
0.0601556861675946));
#35935=CARTESIAN_POINT('Ctrl Pts',(0.122939351496148,-0.0863869407017978,
0.0680617093671122));
#35936=CARTESIAN_POINT('Ctrl Pts',(0.139482338453993,0.0558701933356218,
0.0759677325666295));
#35937=CARTESIAN_POINT('Ctrl Pts',(0.0293081122522375,0.147369339265975,
0.0838737557661469));
#35938=CARTESIAN_POINT('Ctrl Pts',(-0.10749173576994,0.104987027230155,
0.0917797789656645));
#35939=CARTESIAN_POINT('Ctrl Pts',(-0.146637652518404,-0.032774138306667,
0.0996858021651818));
#35940=CARTESIAN_POINT('Ctrl Pts',(-0.0525662186905025,-0.140760516811213,
0.107591825364699));
#35941=CARTESIAN_POINT('Ctrl Pts',(0.089260516735274,-0.120868938074804,
0.115497848564217));
#35942=CARTESIAN_POINT('Ctrl Pts',(0.149995920728193,0.0088296319697477,
0.123403871763734));
#35943=CARTESIAN_POINT('Ctrl Pts',(0.0744631029156597,0.130506640006368,
0.131309894963252));
#35944=CARTESIAN_POINT('Ctrl Pts',(-0.0687179106383172,0.133621057448557,
0.139215918162769));
#35945=CARTESIAN_POINT('Ctrl Pts',(-0.149470115679177,0.0153434817784622,
0.147121941362287));
#35946=CARTESIAN_POINT('Ctrl Pts',(-0.0944317887874227,-0.116873328704402,
0.155027964561804));
#35947=CARTESIAN_POINT('Ctrl Pts',(0.0463958784809096,-0.142913121758123,
0.162933987761322));
#35948=CARTESIAN_POINT('Ctrl Pts',(0.145073843195134,-0.0391192774524402,
0.170840010960839));
#35949=CARTESIAN_POINT('Ctrl Pts',(0.111955200242363,0.10021362663396,0.178746034160356));
#35950=CARTESIAN_POINT('Ctrl Pts',(-0.0228724430773341,0.148504509032441,
0.186652057359874));
#35951=CARTESIAN_POINT('Ctrl Pts',(-0.136920941586459,0.0618820943336314,
0.194558080559391));
#35952=CARTESIAN_POINT('Ctrl Pts',(-0.12657957626731,-0.0809589322677961,
0.202464103758909));
#35953=CARTESIAN_POINT('Ctrl Pts',(-0.00124326519339163,-0.150250431406802,
0.210370126958426));
#35954=CARTESIAN_POINT('Ctrl Pts',(0.125222526785514,-0.0830424989377088,
0.218276150157944));
#35955=CARTESIAN_POINT('Ctrl Pts',(0.137926224580685,0.0596078385548706,
0.226182173357461));
#35956=CARTESIAN_POINT('Ctrl Pts',(0.0253267796170755,0.148105678753651,
0.234088196556978));
#35957=CARTESIAN_POINT('Ctrl Pts',(-0.110281524552332,0.102052551104597,
0.241994219756496));
#35958=CARTESIAN_POINT('Ctrl Pts',(-0.145701328261229,-0.036713223605009,
0.249900242956013));
#35959=CARTESIAN_POINT('Ctrl Pts',(-0.0487544671752176,-0.142125788564551,
0.25780626615553));
#35960=CARTESIAN_POINT('Ctrl Pts',(0.0924848261822464,-0.11841999312036,
0.265712289355049));
#35961=CARTESIAN_POINT('Ctrl Pts',(0.149703554099366,0.012867934356803,
0.273618312554565));
#35962=CARTESIAN_POINT('Ctrl Pts',(0.0709196772318203,0.132465607709839,
0.281524335754083));
#35963=CARTESIAN_POINT('Ctrl Pts',(-0.0722932700879834,0.131720996597282,
0.289430358953601));
#35964=CARTESIAN_POINT('Ctrl Pts',(-0.149829266052005,0.0113105649246307,
0.297336382153118));
#35965=CARTESIAN_POINT('Ctrl Pts',(-0.0912484505038084,-0.119375282723234,
0.305242405352635));
#35966=CARTESIAN_POINT('Ctrl Pts',(0.0502297085693762,-0.141611137350254,
0.313148428552153));
#35967=CARTESIAN_POINT('Ctrl Pts',(0.14607520885827,-0.0351961816339526,
0.32105445175167));
#35968=CARTESIAN_POINT('Ctrl Pts',(0.109214381507085,0.103193782354472,
0.328960474951188));
#35969=CARTESIAN_POINT('Ctrl Pts',(-0.0268654687609187,0.147834314125149,
0.336866498150705));
#35970=CARTESIAN_POINT('Ctrl Pts',(-0.13853859233343,0.0581704072434516,
0.344772521350223));
#35971=CARTESIAN_POINT('Ctrl Pts',(-0.124352249616671,-0.0843401201082281,
0.35267854454974));
#35972=CARTESIAN_POINT('Ctrl Pts',(0.00280555834318869,-0.150229380238954,
0.360584567749258));
#35973=CARTESIAN_POINT('Ctrl Pts',(0.127414574159504,-0.0796383333348297,
0.368490590948775));
#35974=CARTESIAN_POINT('Ctrl Pts',(0.136270065769409,0.0633025040563021,
0.376396614148293));
#35975=CARTESIAN_POINT('Ctrl Pts',(0.0213270008899901,0.148734316408943,
0.38430263734781));
#35976=CARTESIAN_POINT('Ctrl Pts',(-0.112991206354848,0.0990440565156409,
0.392208660547328));
#35977=CARTESIAN_POINT('Ctrl Pts',(-0.144659222864564,-0.0406256948841215,
0.400114683746845));
#35978=CARTESIAN_POINT('Ctrl Pts',(-0.0449073059326639,-0.143387836717301,
0.408020706946362));
#35979=CARTESIAN_POINT('Ctrl Pts',(0.0956419762819073,-0.115885073316145,
0.41592673014588));
#35980=CARTESIAN_POINT('Ctrl Pts',(0.149302487021736,0.0168968995298395,
0.423832753345397));
#35981=CARTESIAN_POINT('Ctrl Pts',(0.0673247541811015,0.134328386125389,
0.431738776544915));
#35982=CARTESIAN_POINT('Ctrl Pts',(-0.0758161353407861,0.129725292316436,
0.439644799744432));
#35983=CARTESIAN_POINT('Ctrl Pts',(-0.150079622765641,0.007269434305358,
0.447550822943949));
#35984=CARTESIAN_POINT('Ctrl Pts',(-0.0879988547449296,-0.121790555496631,
0.455456846143467));
#35985=CARTESIAN_POINT('Ctrl Pts',(0.0540270657832349,-0.140206326560007,
0.463362869342984));
#35986=CARTESIAN_POINT('Ctrl Pts',(0.146970506475833,-0.0312475290356562,
0.471268892542502));
#35987=CARTESIAN_POINT('Ctrl Pts',(0.106394260027447,0.106099006959581,
0.479174915742019));
#35988=CARTESIAN_POINT('Ctrl Pts',(-0.0308389868837996,0.147056773841187,
0.487080938941536));
#35989=CARTESIAN_POINT('Ctrl Pts',(-0.140055647479839,0.0544164814518564,
0.494986962141054));
#35990=CARTESIAN_POINT('Ctrl Pts',(-0.122034628338338,-0.0876600669114554,
0.502892985340571));
#35991=CARTESIAN_POINT('Ctrl Pts',(0.00685234470650933,-0.150099244557128,
0.51079900854009));
#35992=CARTESIAN_POINT('Ctrl Pts',(0.129514103296199,-0.076176340762594,
0.518705031739606));
#35993=CARTESIAN_POINT('Ctrl Pts',(0.134514958571949,0.066951204357981,
0.526611054939125));
#35994=CARTESIAN_POINT('Ctrl Pts',(0.0173117362067031,0.149254955140882,
0.534517078138641));
#35995=CARTESIAN_POINT('Ctrl Pts',(-0.11561884301137,0.0959636440810236,
0.542423101338159));
#35996=CARTESIAN_POINT('Ctrl Pts',(-0.143512077549549,-0.0445086670437286,
0.550329124537675));
#35997=CARTESIAN_POINT('Ctrl Pts',(-0.0410275366085405,-0.144545768130486,
0.558235147737195));
#35998=CARTESIAN_POINT('Ctrl Pts',(0.098729678853994,-0.113266007071779,
0.56614117093671));
#35999=CARTESIAN_POINT('Ctrl Pts',(0.14879300846003,0.0209135955304358,
0.57404719413623));
#36000=CARTESIAN_POINT('Ctrl Pts',(0.0636809452969333,0.136093626047241,
0.581953217335745));
#36001=CARTESIAN_POINT('Ctrl Pts',(-0.0792839490005986,0.127635391939178,
0.589859240535265));
#36002=CARTESIAN_POINT('Ctrl Pts',(-0.150221003701602,0.00322302520629366,
0.59776526373478));
#36003=CARTESIAN_POINT('Ctrl Pts',(-0.0846853612799296,-0.124117393742718,
0.605671286934299));
#36004=CARTESIAN_POINT('Ctrl Pts',(0.0577851928777687,-0.138699709187424,
0.613577310133815));
#36005=CARTESIAN_POINT('Ctrl Pts',(0.147759085906459,-0.0272761869894916,
0.621483333333334));
#36006=CARTESIAN_POINT('Ctrl Pts',(0.103496883574659,0.108927190980628,
0.62938935653285));
#36007=CARTESIAN_POINT('Ctrl Pts',(-0.0347901122093251,0.146172452729842,
0.637295379732368));
#36008=CARTESIAN_POINT('Ctrl Pts',(-0.141471005454986,0.0506230427785409,
0.645201402931886));
#36009=CARTESIAN_POINT('Ctrl Pts',(-0.119628395306551,-0.0909163620091147,
0.653107426131403));
#36010=CARTESIAN_POINT('Ctrl Pts',(0.0108941554469695,-0.149860118849825,
0.661013449330921));
#36011=CARTESIAN_POINT('Ctrl Pts',(0.131519589685118,-0.0726590350451557,
0.668919472530437));
#36012=CARTESIAN_POINT('Ctrl Pts',(0.132662177406628,0.0705512900682209,
0.676825495729956));
#36013=CARTESIAN_POINT('Ctrl Pts',(0.0132839011303035,0.149667216902378,
0.684731518929473));
#36014=CARTESIAN_POINT('Ctrl Pts',(-0.118162526543641,0.0928135505498801,
0.69263754212899));
#36015=CARTESIAN_POINT('Ctrl Pts',(-0.142260725279696,-0.0483593205820741,
0.700543565328508));
#36016=CARTESIAN_POINT('Ctrl Pts',(-0.0371179763826477,-0.145598742005641,
0.708449588528025));
#36017=CARTESIAN_POINT('Ctrl Pts',(0.101745691861845,-0.110564696145857,
0.716355611727543));
#36018=CARTESIAN_POINT('Ctrl Pts',(0.148175488346884,0.0249151057616852,
0.72426163492706));
#36019=CARTESIAN_POINT('Ctrl Pts',(0.0599908964395442,0.137760045689666,
0.732167658126578));
#36020=CARTESIAN_POINT('Ctrl Pts',(-0.0826941930548661,0.125452813002725,
0.740073681326094));
#36021=CARTESIAN_POINT('Ctrl Pts',(-0.150253306133115,-0.000825724231627113,
0.747979704525614));
#36022=CARTESIAN_POINT('Ctrl Pts',(-0.081310376229644,-0.126354107828757,
0.755885727725129));
#36023=CARTESIAN_POINT('Ctrl Pts',(0.0615013612454227,-0.137092379349209,
0.763791750924648));
#36024=CARTESIAN_POINT('Ctrl Pts',(0.148440374085997,-0.0232850389144764,
0.771697774124165));
#36025=CARTESIAN_POINT('Ctrl Pts',(0.100524356866682,0.111676280340869,
0.779603797323682));
#36026=CARTESIAN_POINT('Ctrl Pts',(-0.0387159774106656,0.145181993819149,
0.7875098205232));
#36027=CARTESIAN_POINT('Ctrl Pts',(-0.142783635380297,0.0467928439952764,
0.795415843722717));
#36028=CARTESIAN_POINT('Ctrl Pts',(-0.117135303735115,-0.0941066376761042,
0.803321866922235));
#36029=CARTESIAN_POINT('Ctrl Pts',(0.0149280671231108,-0.149512182952249,
0.811227890121752));
#36030=CARTESIAN_POINT('Ctrl Pts',(0.133429555455635,-0.0690889583890887,
0.819133913321269));
#36031=CARTESIAN_POINT('Ctrl Pts',(0.13071310873075,0.0741001247218646,
0.827039936520788));
#36032=CARTESIAN_POINT('Ctrl Pts',(0.00924634225633868,0.149970844834382,
0.834945959720303));
#36033=CARTESIAN_POINT('Ctrl Pts',(-0.120620261601548,0.0895959825586721,
0.842851982919823));
#36034=CARTESIAN_POINT('Ctrl Pts',(-0.140906356422368,-0.0521747061680897,
0.850758006119338));
#36035=CARTESIAN_POINT('Ctrl Pts',(-0.0331809289437206,-0.146546284922345,
0.858664029318857));
#36036=CARTESIAN_POINT('Ctrl Pts',(0.104686808927989,-0.107782548984136,
0.866570052518374));
#36037=CARTESIAN_POINT('Ctrl Pts',(0.147452305580495,0.0288974742383162,
0.874476075717892));
#36038=CARTESIAN_POINT('Ctrl Pts',(0.0562536202549592,0.139328430172098,
0.882382098917409));
#36039=CARTESIAN_POINT('Ctrl Pts',(-0.0860374264415029,0.123175350607342,
0.890288122116927));
#36040=CARTESIAN_POINT('Ctrl Pts',(-0.150189737621406,-0.00486667430221375,
0.898194145316444));
#36041=CARTESIAN_POINT('Ctrl Pts',(-0.0778512004163494,-0.128512763786642,
0.906100168515961));
#36042=CARTESIAN_POINT('Ctrl Pts',(0.0651249400548213,-0.135359373728788,
0.914006191715479));
#36043=CARTESIAN_POINT('Ctrl Pts',(0.149106309520794,-0.0193277002139675,
0.921912214914997));
#36044=CARTESIAN_POINT('Ctrl Pts',(0.0972914655469444,0.114449752166959,
0.929818238114513));
#36045=CARTESIAN_POINT('Ctrl Pts',(0.00432320985889779,0.134029312831529,
0.935088920247525));
#36046=CARTESIAN_POINT('Ctrl Pts',(-0.0361033354336585,0.122073089461047,
0.937724261314031));
#36047=CARTESIAN_POINT('Ctrl Pts',(-0.0592743564846289,0.123319225136769,
-0.00549926131403118));
#36048=CARTESIAN_POINT('Ctrl Pts',(-0.10011358044828,0.103689530601369,
-0.00286392024752536));
#36049=CARTESIAN_POINT('Ctrl Pts',(-0.160078034541183,0.0210334216764563,
0.00240676188548625));
#36050=CARTESIAN_POINT('Ctrl Pts',(-0.104882388816361,-0.122944882360947,
0.0103127850850037));
#36051=CARTESIAN_POINT('Ctrl Pts',(0.0457298202147887,-0.154838818620857,
0.0182188082845211));
#36052=CARTESIAN_POINT('Ctrl Pts',(0.154729058131587,-0.0462614617356896,
0.0261248314840386));
#36053=CARTESIAN_POINT('Ctrl Pts',(0.123195923521052,0.104445863960627,
0.034030854683556));
#36054=CARTESIAN_POINT('Ctrl Pts',(-0.0202770029016287,0.160212496691623,
0.0419368778830735));
#36055=CARTESIAN_POINT('Ctrl Pts',(-0.145318780043635,0.0704576601202616,
0.049842901082591));
#36056=CARTESIAN_POINT('Ctrl Pts',(-0.138346646019881,-0.0833214085615725,
0.0577489242821084));
#36057=CARTESIAN_POINT('Ctrl Pts',(-0.00568667862689953,-0.16139684682825,
0.0656549474816259));
#36058=CARTESIAN_POINT('Ctrl Pts',(0.132138073593561,-0.0928506925492821,
0.0735609706811433));
#36059=CARTESIAN_POINT('Ctrl Pts',(0.149918860636037,0.060050582899814,
0.0814669938806607));
#36060=CARTESIAN_POINT('Ctrl Pts',(0.031501040525629,0.158395992498563,
0.0893730170801781));
#36061=CARTESIAN_POINT('Ctrl Pts',(-0.115534617020597,0.112842498042153,
0.0972790402796957));
#36062=CARTESIAN_POINT('Ctrl Pts',(-0.157609558568976,-0.0352264059215207,
0.105185063479213));
#36063=CARTESIAN_POINT('Ctrl Pts',(-0.0564993941266941,-0.151292676454786,
0.113091086678731));
#36064=CARTESIAN_POINT('Ctrl Pts',(0.0959392788869109,-0.129912745106718,
0.120997109878248));
#36065=CARTESIAN_POINT('Ctrl Pts',(0.161219103327847,0.00949029374910116,
0.128903133077765));
#36066=CARTESIAN_POINT('Ctrl Pts',(0.0800346744417541,0.140271571240151,
0.136809156277283));
#36067=CARTESIAN_POINT('Ctrl Pts',(-0.0738596081939327,0.143619019523951,
0.1447151794768));
#36068=CARTESIAN_POINT('Ctrl Pts',(-0.160653955835061,0.0164915309845896,
0.152621202676318));
#36069=CARTESIAN_POINT('Ctrl Pts',(-0.101497482331809,-0.125618171248858,
0.160527225875835));
#36070=CARTESIAN_POINT('Ctrl Pts',(0.0498673689956821,-0.15360634630444,
0.168433249075353));
#36071=CARTESIAN_POINT('Ctrl Pts',(0.15592873994638,-0.0420463090135921,
0.17633927227487));
#36072=CARTESIAN_POINT('Ctrl Pts',(0.120332052420749,0.107711936089485,
0.184245295474388));
#36073=CARTESIAN_POINT('Ctrl Pts',(-0.0245838336532294,0.15961609935871,
0.192151318673905));
#36074=CARTESIAN_POINT('Ctrl Pts',(-0.147165811724802,0.0665123138821622,
0.200057341873423));
#36075=CARTESIAN_POINT('Ctrl Pts',(-0.136050671820698,-0.0870165428714931,
0.20796336507294));
#36076=CARTESIAN_POINT('Ctrl Pts',(-0.00133629033845999,-0.16149265732314,
0.215869388272457));
#36077=CARTESIAN_POINT('Ctrl Pts',(0.134592083483329,-0.0892560087757434,
0.223775411471975));
#36078=CARTESIAN_POINT('Ctrl Pts',(0.148246313261997,0.0640678908897882,
0.231681434671492));
#36079=CARTESIAN_POINT('Ctrl Pts',(0.0272218116347722,0.159187427301401,
0.23958745787101));
#36080=CARTESIAN_POINT('Ctrl Pts',(-0.118533146872527,0.109688454869495,
0.247493481070527));
#36081=CARTESIAN_POINT('Ctrl Pts',(-0.156603175485803,-0.0394602263924212,
0.255399504270045));
#36082=CARTESIAN_POINT('Ctrl Pts',(-0.0524024349666086,-0.152760102280791,
0.263305527469562));
#36083=CARTESIAN_POINT('Ctrl Pts',(0.0994048416526766,-0.127280562126421,
0.27121155066908));
#36084=CARTESIAN_POINT('Ctrl Pts',(0.160904860877029,0.0138307550539624,
0.279117573868597));
#36085=CARTESIAN_POINT('Ctrl Pts',(0.0762261181244613,0.142377115278073,
0.287023597068114));
#36086=CARTESIAN_POINT('Ctrl Pts',(-0.0777024876652646,0.141576789940481,
0.294929620267632));
#36087=CARTESIAN_POINT('Ctrl Pts',(-0.1610399790068,0.0121568581760624,
0.302835643467149));
#36088=CARTESIAN_POINT('Ctrl Pts',(-0.098075956325088,-0.128307329604135,
0.310741666666667));
#36089=CARTESIAN_POINT('Ctrl Pts',(0.0539880587195976,-0.152206943188912,
0.318647689866184));
#36090=CARTESIAN_POINT('Ctrl Pts',(0.157005031045033,-0.037829674407429,
0.326553713065702));
#36091=CARTESIAN_POINT('Ctrl Pts',(0.117386156714116,0.11091507675295,0.334459736265219));
#36092=CARTESIAN_POINT('Ctrl Pts',(-0.0288756305044191,0.158895758288873,
0.342365759464736));
#36093=CARTESIAN_POINT('Ctrl Pts',(-0.14890450036152,0.0625229062928939,
0.350271782664254));
#36094=CARTESIAN_POINT('Ctrl Pts',(-0.133656689346435,-0.0906507221823109,
0.358177805863771));
#36095=CARTESIAN_POINT('Ctrl Pts',(0.0030154793425501,-0.161470031038451,
0.366083829063289));
#36096=CARTESIAN_POINT('Ctrl Pts',(0.136948146970731,-0.0855971324315648,
0.373989852262806));
#36097=CARTESIAN_POINT('Ctrl Pts',(0.146466235262368,0.0680390032796811,
0.381895875462324));
#36098=CARTESIAN_POINT('Ctrl Pts',(0.0229227564554051,0.159863101670492,
0.389801898661841));
#36099=CARTESIAN_POINT('Ctrl Pts',(-0.121445575879827,0.106454854931286,
0.397707921861359));
#36100=CARTESIAN_POINT('Ctrl Pts',(-0.155483096374265,-0.0436654414966204,
0.405613945060876));
#36101=CARTESIAN_POINT('Ctrl Pts',(-0.0482674166083024,-0.154116580980712,
0.413519968260394));
#36102=CARTESIAN_POINT('Ctrl Pts',(0.102798219990352,-0.124555971378489,
0.421425991459911));
#36103=CARTESIAN_POINT('Ctrl Pts',(0.160473784656316,0.018161180504086,
0.429332014659428));
#36104=CARTESIAN_POINT('Ctrl Pts',(0.072362211239822,0.144379272832728,
0.437238037858946));
#36105=CARTESIAN_POINT('Ctrl Pts',(-0.0814889451532045,0.139431760574992,
0.445144061058463));
#36106=CARTESIAN_POINT('Ctrl Pts',(-0.16130906822395,0.00781335702145124,
0.453050084257981));
#36107=CARTESIAN_POINT('Ctrl Pts',(-0.0945832152433237,-0.130903320941292,
0.460956107457498));
#36108=CARTESIAN_POINT('Ctrl Pts',(0.0580695465498112,-0.150697019886669,
0.468862130657016));
#36109=CARTESIAN_POINT('Ctrl Pts',(0.157967317741994,-0.033585570780077,
0.476768153856533));
#36110=CARTESIAN_POINT('Ctrl Pts',(0.114355024573885,0.114037679711269,
0.48467417705605));
#36111=CARTESIAN_POINT('Ctrl Pts',(-0.0331464601757716,0.15806003991218,
0.492580200255568));
#36112=CARTESIAN_POINT('Ctrl Pts',(-0.15053506650769,0.0584880995652034,
0.500486223455085));
#36113=CARTESIAN_POINT('Ctrl Pts',(-0.131165656106781,-0.0942190782023548,
0.508392246654604));
#36114=CARTESIAN_POINT('Ctrl Pts',(0.00736505942237213,-0.161330158181689,
0.51629826985412));
#36115=CARTESIAN_POINT('Ctrl Pts',(0.139204769705438,-0.0818761023161199,
0.524204293053638));
#36116=CARTESIAN_POINT('Ctrl Pts',(0.144579805236504,0.0719607112040898,
0.532110316253155));
#36117=CARTESIAN_POINT('Ctrl Pts',(0.0186070566102303,0.160422696285555,
0.540016339452673));
#36118=CARTESIAN_POINT('Ctrl Pts',(-0.124269820856485,0.103143956020315,
0.547922362652189));
#36119=CARTESIAN_POINT('Ctrl Pts',(-0.154250117916081,-0.047838950261257,
0.555828385851708));
#36120=CARTESIAN_POINT('Ctrl Pts',(-0.0440973503257164,-0.15536115258801,
0.563734409051225));
#36121=CARTESIAN_POINT('Ctrl Pts',(0.106116954510586,-0.121740938080097,
0.571640432250743));
#36122=CARTESIAN_POINT('Ctrl Pts',(0.159926185251717,0.022478418762386,
0.579546455450259));
#36123=CARTESIAN_POINT('Ctrl Pts',(0.06844576072469,0.146276593746376,0.587452478649778));
#36124=CARTESIAN_POINT('Ctrl Pts',(-0.08521623190893,0.137185487054817,
0.595358501849294));
#36125=CARTESIAN_POINT('Ctrl Pts',(-0.161461027741333,0.00346418243402402,
0.603264525048813));
#36126=CARTESIAN_POINT('Ctrl Pts',(-0.0910217954212606,-0.133404260792202,
0.611170548248329));
#36127=CARTESIAN_POINT('Ctrl Pts',(0.0621088689355897,-0.149077672502509,
0.619076571447848));
#36128=CARTESIAN_POINT('Ctrl Pts',(0.158814901250206,-0.0293170800065776,
0.626982594647363));
#36129=CARTESIAN_POINT('Ctrl Pts',(0.111240856992166,0.117077477658479,
0.634888617846883));
#36130=CARTESIAN_POINT('Ctrl Pts',(-0.0373932215478457,0.15710955101933,
0.642794641046398));
#36131=CARTESIAN_POINT('Ctrl Pts',(-0.152056326169508,0.0544108234734799,
0.650700664245917));
#36132=CARTESIAN_POINT('Ctrl Pts',(-0.1285793808941,-0.0977190198892145,
0.658606687445434));
#36133=CARTESIAN_POINT('Ctrl Pts',(0.0117092915870499,-0.161073140311291,
0.666512710644951));
#36134=CARTESIAN_POINT('Ctrl Pts',(0.14136031310814,-0.0780956203460609,
0.67441873384447));
#36135=CARTESIAN_POINT('Ctrl Pts',(0.142588392958853,0.0758301670352254,
0.682324757043986));
#36136=CARTESIAN_POINT('Ctrl Pts',(0.0142778458142493,0.160865804812787,
0.690230780243504));
#36137=CARTESIAN_POINT('Ctrl Pts',(-0.127003831063107,0.0997581622465629,
0.698136803443022));
#36138=CARTESIAN_POINT('Ctrl Pts',(-0.152905135399799,-0.0519777222202838,
0.706042826642539));
#36139=CARTESIAN_POINT('Ctrl Pts',(-0.0398952640892059,-0.156492913392945,
0.713948849842056));
#36140=CARTESIAN_POINT('Ctrl Pts',(0.109358635420242,-0.118837506285601,
0.721854873041575));
#36141=CARTESIAN_POINT('Ctrl Pts',(0.159262460275431,0.0267793350026898,
0.729760896241091));
#36142=CARTESIAN_POINT('Ctrl Pts',(0.0644796104111608,0.148067700325911,
0.737666919440608));
#36143=CARTESIAN_POINT('Ctrl Pts',(-0.0888816415139979,0.134839600464242,
0.745572942640127));
#36144=CARTESIAN_POINT('Ctrl Pts',(-0.161495747145824,-0.000887507604023794,
0.753478965839642));
#36145=CARTESIAN_POINT('Ctrl Pts',(-0.0873942830135206,-0.135808333100311,
0.761384989039162));
#36146=CARTESIAN_POINT('Ctrl Pts',(0.0661030931060867,-0.147350077018504,
0.769291012238677));
#36147=CARTESIAN_POINT('Ctrl Pts',(0.159547165626996,-0.0250273012527367,
0.777197035438197));
#36148=CARTESIAN_POINT('Ctrl Pts',(0.108045916168766,0.120032262825132,
0.785103058637712));
#36149=CARTESIAN_POINT('Ctrl Pts',(-0.0416128327510934,0.156044982751807,
0.793009081837232));
#36150=CARTESIAN_POINT('Ctrl Pts',(-0.153467171334714,0.0502940367608314,
0.800915105036747));
#36151=CARTESIAN_POINT('Ctrl Pts',(-0.125899748103356,-0.101148002356896,
0.808821128236267));
#36152=CARTESIAN_POINT('Ctrl Pts',(0.0160450336537275,-0.160699170718315,
0.816727151435783));
#36153=CARTESIAN_POINT('Ctrl Pts',(0.143413188729122,-0.0742584189441255,
0.824633174635301));
#36154=CARTESIAN_POINT('Ctrl Pts',(0.140493488625962,0.0796445370390336,
0.832539197834818));
#36155=CARTESIAN_POINT('Ctrl Pts',(0.00993818365454583,0.161192151174111,
0.840445221034335));
#36156=CARTESIAN_POINT('Ctrl Pts',(-0.129645461850996,0.0962998453542059,
0.848351244233853));
#36157=CARTESIAN_POINT('Ctrl Pts',(-0.151449428259942,-0.0560785873640905,
0.85625726743337));
#36158=CARTESIAN_POINT('Ctrl Pts',(-0.0356636339569891,-0.157511354552237,
0.864163290632887));
#36159=CARTESIAN_POINT('Ctrl Pts',(0.112519816430259,-0.115847189825252,
0.872069313832405));
#36160=CARTESIAN_POINT('Ctrl Pts',(0.158485166622555,0.0310596772400429,
0.879975337031923));
#36161=CARTESIAN_POINT('Ctrl Pts',(0.0604626990682241,0.149753436435956,
0.88788136023144));
#36162=CARTESIAN_POINT('Ctrl Pts',(-0.0924750264953536,0.132391730925763,
0.895787383430957));
#36163=CARTESIAN_POINT('Ctrl Pts',(-0.161427422231335,-0.00523081470070893,
0.903693406630475));
#36164=CARTESIAN_POINT('Ctrl Pts',(-0.083676280416081,-0.13812850671726,
0.911599429829993));
#36165=CARTESIAN_POINT('Ctrl Pts',(0.0699977998664634,-0.145487402281552,
0.91950545302951));
#36166=CARTESIAN_POINT('Ctrl Pts',(0.160262928516753,-0.020773861600756,
0.927411476229027));
#36167=CARTESIAN_POINT('Ctrl Pts',(0.104571129406605,0.123013254833025,
0.935317499428545));
#36168=CARTESIAN_POINT('Ctrl Pts',(0.0046466864803128,0.144057821902388,
0.940588181561556));
#36169=CARTESIAN_POINT('Ctrl Pts',(-0.0388047044046363,0.131206995015772,
0.943223522628062));
#36170=CARTESIAN_POINT('Ctrl Pts',(-0.0634007094575211,0.131904027763685,
0.));
#36171=CARTESIAN_POINT('Ctrl Pts',(-0.107082934395072,0.110907822426533,
0.00263534106650582));
#36172=CARTESIAN_POINT('Ctrl Pts',(-0.171221782240834,0.0224976522006178,
0.00790602319951745));
#36173=CARTESIAN_POINT('Ctrl Pts',(-0.112183720835187,-0.131503625313535,
0.0158120463990349));
#36174=CARTESIAN_POINT('Ctrl Pts',(0.0489132774597784,-0.165617841075552,
0.0237180695985523));
#36175=CARTESIAN_POINT('Ctrl Pts',(0.165500439667881,-0.0494819289239417,
0.0316240927980698));
#36176=CARTESIAN_POINT('Ctrl Pts',(0.131772142571212,0.111716807532525,
0.0395301159975872));
#36177=CARTESIAN_POINT('Ctrl Pts',(-0.0216885757328939,0.171365604902752,
0.0474361391971047));
#36178=CARTESIAN_POINT('Ctrl Pts',(-0.155435070048499,0.0753625328602259,
0.055342162396622));
#36179=CARTESIAN_POINT('Ctrl Pts',(-0.147977574602665,-0.0891217843448639,
0.0632481855961397));
#36180=CARTESIAN_POINT('Ctrl Pts',(-0.00608255375148451,-0.172632402947666,
0.0711542087956569));
#36181=CARTESIAN_POINT('Ctrl Pts',(0.141336795690974,-0.0993144443967663,
0.0790602319951745));
#36182=CARTESIAN_POINT('Ctrl Pts',(0.160355382818083,0.0642309724640062,
0.0869662551946919));
#36183=CARTESIAN_POINT('Ctrl Pts',(0.03369396879902,0.16942264573115,0.0948722783942093));
#36184=CARTESIAN_POINT('Ctrl Pts',(-0.123577498271253,0.120697968854151,
0.102778301593727));
#36185=CARTESIAN_POINT('Ctrl Pts',(-0.168581464619548,-0.0376786735363742,
0.110684324793244));
#36186=CARTESIAN_POINT('Ctrl Pts',(-0.0604325695628853,-0.161824836098358,
0.118590347992762));
#36187=CARTESIAN_POINT('Ctrl Pts',(0.102618041038548,-0.138956552138631,
0.126496371192279));
#36188=CARTESIAN_POINT('Ctrl Pts',(0.172442285927502,0.0101509555284547,
0.134402394391796));
#36189=CARTESIAN_POINT('Ctrl Pts',(0.085606245967848,0.150036502473934,
0.142308417591314));
#36190=CARTESIAN_POINT('Ctrl Pts',(-0.0790013057495479,0.153616981599344,
0.150214440790831));
#36191=CARTESIAN_POINT('Ctrl Pts',(-0.171837795990946,0.0176395801907167,
0.158120463990349));
#36192=CARTESIAN_POINT('Ctrl Pts',(-0.108563175876194,-0.134363013793315,
0.166026487189866));
#36193=CARTESIAN_POINT('Ctrl Pts',(0.0533388595104543,-0.164299570850757,
0.173932510389384));
#36194=CARTESIAN_POINT('Ctrl Pts',(0.166783636697626,-0.0449733405747439,
0.181838533588901));
#36195=CARTESIAN_POINT('Ctrl Pts',(0.128708904599136,0.11521024554501,0.189744556788419));
#36196=CARTESIAN_POINT('Ctrl Pts',(-0.0262952242291247,0.170727689684979,
0.197650579987936));
#36197=CARTESIAN_POINT('Ctrl Pts',(-0.157410681863144,0.071142533430693,
0.205556603187454));
#36198=CARTESIAN_POINT('Ctrl Pts',(-0.145521767374085,-0.0930741534751901,
0.213462626386971));
#36199=CARTESIAN_POINT('Ctrl Pts',(-0.00142931548352814,-0.172734883239477,
0.221368649586489));
#36200=CARTESIAN_POINT('Ctrl Pts',(0.143961640181145,-0.0954695186137778,
0.229274672786006));
#36201=CARTESIAN_POINT('Ctrl Pts',(0.15856640194331,0.0685279432247057,
0.237180695985524));
#36202=CARTESIAN_POINT('Ctrl Pts',(0.0291168436524689,0.17026917584915,
0.24508671918504));
#36203=CARTESIAN_POINT('Ctrl Pts',(-0.126784769192722,0.117324358634392,
0.252992742384559));
#36204=CARTESIAN_POINT('Ctrl Pts',(-0.167505022710376,-0.0422072291798334,
0.260898765584075));
#36205=CARTESIAN_POINT('Ctrl Pts',(-0.0560504027579997,-0.16339441599703,
0.268804788783594));
#36206=CARTESIAN_POINT('Ctrl Pts',(0.106324857123107,-0.136141131132482,
0.27671081198311));
#36207=CARTESIAN_POINT('Ctrl Pts',(0.172106167654692,0.0147935757511219,
0.284616835182629));
#36208=CARTESIAN_POINT('Ctrl Pts',(0.0815325590171024,0.152288622846307,
0.292522858382145));
#36209=CARTESIAN_POINT('Ctrl Pts',(-0.0831117052425459,0.151432583283679,
0.300428881581663));
#36210=CARTESIAN_POINT('Ctrl Pts',(-0.172250691961594,0.0130031514274941,
0.30833490478118));
#36211=CARTESIAN_POINT('Ctrl Pts',(-0.104903462146368,-0.137239376485036,
0.316240927980698));
#36212=CARTESIAN_POINT('Ctrl Pts',(0.0577464088698189,-0.16280274902757,
0.324146951180215));
#36213=CARTESIAN_POINT('Ctrl Pts',(0.167934853231796,-0.0404631671809053,
0.332052974379733));
#36214=CARTESIAN_POINT('Ctrl Pts',(0.125557931921148,0.118636371151428,
0.33995899757925));
#36215=CARTESIAN_POINT('Ctrl Pts',(-0.0308857922479196,0.169957202452597,
0.347865020778768));
#36216=CARTESIAN_POINT('Ctrl Pts',(-0.15927040838961,0.0668754053423362,
0.355771043978284));
#36217=CARTESIAN_POINT('Ctrl Pts',(-0.142961129076198,-0.0969613242563938,
0.363677067177803));
#36218=CARTESIAN_POINT('Ctrl Pts',(0.0032254003419117,-0.172710681837949,
0.371583090377319));
#36219=CARTESIAN_POINT('Ctrl Pts',(0.146481719781958,-0.0915559315282998,
0.379489113576838));
#36220=CARTESIAN_POINT('Ctrl Pts',(0.156662404755327,0.0727755025030601,
0.387395136776354));
#36221=CARTESIAN_POINT('Ctrl Pts',(0.0245185120208197,0.170991886932041,
0.395301159975873));
#36222=CARTESIAN_POINT('Ctrl Pts',(-0.129899945404805,0.113865653346931,
0.403207183175389));
#36223=CARTESIAN_POINT('Ctrl Pts',(-0.166306969883967,-0.0467051881091194,
0.411113206374907));
#36224=CARTESIAN_POINT('Ctrl Pts',(-0.0516275272839405,-0.164845325244123,
0.419019229574424));
#36225=CARTESIAN_POINT('Ctrl Pts',(0.109954463698797,-0.133226869440833,
0.426925252773942));
#36226=CARTESIAN_POINT('Ctrl Pts',(0.171645082290897,0.0194254614783324,
0.434831275973459));
#36227=CARTESIAN_POINT('Ctrl Pts',(0.0773996682985425,0.154430159540067,
0.442737299172977));
#36228=CARTESIAN_POINT('Ctrl Pts',(-0.0871617549656229,0.149138228833548,
0.450643322372495));
#36229=CARTESIAN_POINT('Ctrl Pts',(-0.172538513682259,0.00835727973754467,
0.458549345572012));
#36230=CARTESIAN_POINT('Ctrl Pts',(-0.101167575741718,-0.140016086385953,
0.466455368771529));
#36231=CARTESIAN_POINT('Ctrl Pts',(0.0621120273163875,-0.161187713213332,
0.474361391971047));
#36232=CARTESIAN_POINT('Ctrl Pts',(0.168964129008155,-0.0359236125244978,
0.482267415170563));
#36233=CARTESIAN_POINT('Ctrl Pts',(0.122315789120323,0.121976352462958,
0.490173438370083));
#36234=CARTESIAN_POINT('Ctrl Pts',(-0.0354539334677437,0.169063305983172,
0.498079461569598));
#36235=CARTESIAN_POINT('Ctrl Pts',(-0.161014485535541,0.0625597176785504,
0.505985484769117));
#36236=CARTESIAN_POINT('Ctrl Pts',(-0.140296683875224,-0.100778089493254,
0.513891507968634));
#36237=CARTESIAN_POINT('Ctrl Pts',(0.00787777413823514,-0.17256107180625,
0.521797531168151));
#36238=CARTESIAN_POINT('Ctrl Pts',(0.148895436114678,-0.0875758638696457,
0.529703554367669));
#36239=CARTESIAN_POINT('Ctrl Pts',(0.154644651901059,0.0769702180501986,
0.537609577567186));
#36240=CARTESIAN_POINT('Ctrl Pts',(0.0199023770137573,0.171590437430228,
0.545515600766704));
#36241=CARTESIAN_POINT('Ctrl Pts',(-0.132920798701601,0.110324267959608,
0.553421623966221));
#36242=CARTESIAN_POINT('Ctrl Pts',(-0.164988158282613,-0.0511692334787857,
0.561327647165738));
#36243=CARTESIAN_POINT('Ctrl Pts',(-0.0471671640428923,-0.166176537045534,
0.569233670365257));
#36244=CARTESIAN_POINT('Ctrl Pts',(0.113504230167178,-0.130215869088414,
0.577139693564773));
#36245=CARTESIAN_POINT('Ctrl Pts',(0.171059362043405,0.0240432419943362,
0.585045716764291));
#36246=CARTESIAN_POINT('Ctrl Pts',(0.0732105761524465,0.156459561445511,
0.592951739963808));
#36247=CARTESIAN_POINT('Ctrl Pts',(-0.0911485148172611,0.146735582170455,
0.600857763163326));
#36248=CARTESIAN_POINT('Ctrl Pts',(-0.172701051781065,0.00370533966175465,
0.608763786362843));
#36249=CARTESIAN_POINT('Ctrl Pts',(-0.0973582295625918,-0.142691127841686,
0.616669809562361));
#36250=CARTESIAN_POINT('Ctrl Pts',(0.0664325449934107,-0.159455635817593,
0.624575832761878));
#36251=CARTESIAN_POINT('Ctrl Pts',(0.169870716593952,-0.0313579730236637,
0.632481855961396));
#36252=CARTESIAN_POINT('Ctrl Pts',(0.118984830409674,0.12522776433633,0.640387879160913));
#36253=CARTESIAN_POINT('Ctrl Pts',(-0.0399963308863663,0.168046649308817,
0.648293902360431));
#36254=CARTESIAN_POINT('Ctrl Pts',(-0.162641646884031,0.0581986041684188,
0.656199925559947));
#36255=CARTESIAN_POINT('Ctrl Pts',(-0.137530366481649,-0.104521677769314,
0.664105948759466));
#36256=CARTESIAN_POINT('Ctrl Pts',(0.0125244277271302,-0.172286161772757,
0.672011971958982));
#36257=CARTESIAN_POINT('Ctrl Pts',(0.151201036531162,-0.0835322056469662,
0.679917995158501));
#36258=CARTESIAN_POINT('Ctrl Pts',(0.152514608511077,0.08110904400223,0.687824018358017));
#36259=CARTESIAN_POINT('Ctrl Pts',(0.015271790498195,0.172064392723197,
0.695730041557536));
#36260=CARTESIAN_POINT('Ctrl Pts',(-0.135845135582574,0.106702773943246,
0.703636064757053));
#36261=CARTESIAN_POINT('Ctrl Pts',(-0.163549545519903,-0.0555961238584937,
0.71154208795657));
#36262=CARTESIAN_POINT('Ctrl Pts',(-0.042672551795764,-0.167387084780248,
0.719448111156087));
#36263=CARTESIAN_POINT('Ctrl Pts',(0.116971578978639,-0.127110316425345,
0.727354134355605));
#36264=CARTESIAN_POINT('Ctrl Pts',(0.170349432203978,0.0286435642436946,
0.735260157555123));
#36265=CARTESIAN_POINT('Ctrl Pts',(0.0689683243827774,0.158375354962157,
0.74316618075464));
#36266=CARTESIAN_POINT('Ctrl Pts',(-0.0950690899731296,0.144226387925758,
0.751072203954158));
#36267=CARTESIAN_POINT('Ctrl Pts',(-0.172738188158534,-0.000949290976420475,
0.758978227153675));
#36268=CARTESIAN_POINT('Ctrl Pts',(-0.0934781897973971,-0.145262558371866,
0.766884250353192));
#36269=CARTESIAN_POINT('Ctrl Pts',(0.0707048249667505,-0.157607774687799,
0.77479027355271));
#36270=CARTESIAN_POINT('Ctrl Pts',(0.170653957167994,-0.026769563590997,
0.782696296752227));
#36271=CARTESIAN_POINT('Ctrl Pts',(0.115567475470849,0.128388245309395,
0.790602319951745));
#36272=CARTESIAN_POINT('Ctrl Pts',(-0.044509688091521,0.166907971684466,
0.798508343151262));
#36273=CARTESIAN_POINT('Ctrl Pts',(-0.164150707289131,0.0537952295263864,
0.806414366350779));
#36274=CARTESIAN_POINT('Ctrl Pts',(-0.134664192471597,-0.108189367037688,
0.814320389550297));
#36275=CARTESIAN_POINT('Ctrl Pts',(0.0171620001843438,-0.171886158484381,
0.822226412749814));
#36276=CARTESIAN_POINT('Ctrl Pts',(0.153396822002609,-0.0794278794991626,
0.830132435949332));
#36277=CARTESIAN_POINT('Ctrl Pts',(0.150273868521174,0.0851889493562029,
0.838038459148849));
#36278=CARTESIAN_POINT('Ctrl Pts',(0.010630025052753,0.17241345751384,0.845944482348367));
#36279=CARTESIAN_POINT('Ctrl Pts',(-0.138670662100443,0.10300370814974,
0.853850505547884));
#36280=CARTESIAN_POINT('Ctrl Pts',(-0.161992500097515,-0.0599824685600915,
0.861756528747401));
#36281=CARTESIAN_POINT('Ctrl Pts',(-0.0381463389702577,-0.16847642418213,
0.869662551946919));
#36282=CARTESIAN_POINT('Ctrl Pts',(0.120352823932529,-0.123911830666367,
0.877568575146436));
#36283=CARTESIAN_POINT('Ctrl Pts',(0.169518027664615,0.0332218802417698,
0.885474598345955));
#36284=CARTESIAN_POINT('Ctrl Pts',(0.064671777881489,0.160178442699814,
0.89338062154547));
#36285=CARTESIAN_POINT('Ctrl Pts',(-0.0989126265492044,0.141608111244184,
0.90128664474499));
#36286=CARTESIAN_POINT('Ctrl Pts',(-0.172665106841263,-0.00559495509920419,
0.909192667944505));
#36287=CARTESIAN_POINT('Ctrl Pts',(-0.0895013604158129,-0.147744249647878,
0.917098691144024));
#36288=CARTESIAN_POINT('Ctrl Pts',(0.0748706596781056,-0.155615430834315,
0.925004714343541));
#36289=CARTESIAN_POINT('Ctrl Pts',(0.171419547512711,-0.0222200229875446,
0.932910737543058));
#36290=CARTESIAN_POINT('Ctrl Pts',(0.111850793266265,0.131576757499091,
0.940816760742576));
#36291=CARTESIAN_POINT('Ctrl Pts',(0.00497016310172783,0.154086330973247,
0.946087442875587));
#36292=CARTESIAN_POINT('Ctrl Pts',(-0.0415060733756141,0.140340900570497,
0.948722783942093));
#36293=CARTESIAN_POINT('Ctrl Pts',(-0.146190615322833,-9.92620605964336E-5,
0.858934495415709));
#36294=CARTESIAN_POINT('Ctrl Pts',(-0.146299982018485,-0.0174419138812775,
0.85987517319294));
#36295=CARTESIAN_POINT('Ctrl Pts',(-0.143444813888727,-0.0347497500736094,
0.860815850970171));
#36296=CARTESIAN_POINT('Ctrl Pts',(-0.13746450024346,-0.0509004317121259,
0.861756528747401));
#36297=CARTESIAN_POINT('Ctrl Pts',(-0.120710446388429,-0.0961471204341042,
0.864391869813907));
#36298=CARTESIAN_POINT('Ctrl Pts',(-0.0794283926793434,-0.132311772308117,
0.867027210880413));
#36299=CARTESIAN_POINT('Ctrl Pts',(-0.032370838674336,-0.142966665992496,
0.869662551946919));
#36300=CARTESIAN_POINT('Ctrl Pts',(0.014686715330672,-0.153621559676876,
0.872297893013425));
#36301=CARTESIAN_POINT('Ctrl Pts',(0.0675197696316001,-0.138766695171622,
0.874933234079931));
#36302=CARTESIAN_POINT('Ctrl Pts',(0.10213049740408,-0.105150311100971,
0.877568575146437));
#36303=CARTESIAN_POINT('Ctrl Pts',(0.136741225176558,-0.0715339270303214,
0.880203916212942));
#36304=CARTESIAN_POINT('Ctrl Pts',(0.153129626420586,-0.019156023394278,
0.882839257279448));
#36305=CARTESIAN_POINT('Ctrl Pts',(0.143849452078747,0.028192355500085,
0.885474598345954));
#36306=CARTESIAN_POINT('Ctrl Pts',(0.134569277736908,0.0755407343944486,
0.88810993941246));
#36307=CARTESIAN_POINT('Ctrl Pts',(0.0996205278091978,0.117859588547133,
0.890745280478965));
#36308=CARTESIAN_POINT('Ctrl Pts',(0.0548820854402278,0.135923960380868,
0.893380621545471));
#36309=CARTESIAN_POINT('Ctrl Pts',(0.0101436430712571,0.153988332214605,
0.896015962611977));
#36310=CARTESIAN_POINT('Ctrl Pts',(-0.0443844917389754,0.147798221729394,
0.898651303678484));
#36311=CARTESIAN_POINT('Ctrl Pts',(-0.0839406391927675,0.120169322096223,
0.901286644744989));
#36312=CARTESIAN_POINT('Ctrl Pts',(-0.0957651970765149,0.111910188080244,
0.902074429829993));
#36313=CARTESIAN_POINT('Ctrl Pts',(-0.106251862209464,0.10173528965009,
0.902862214914997));
#36314=CARTESIAN_POINT('Ctrl Pts',(-0.115101970897794,0.0902398078595192,
0.903650000000001));
#36315=CARTESIAN_POINT('Ctrl Pts',(-0.0686121729278153,-0.0959472995825293,
-5.42101086242752E-19));
#36316=CARTESIAN_POINT('Ctrl Pts',(-0.0716149353959019,-0.0943161956304311,
-1.06730581618305E-18));
#36317=CARTESIAN_POINT('Ctrl Pts',(-0.0745354620527207,-0.0925505885939475,
1.1783117230653E-17));
#36318=CARTESIAN_POINT('Ctrl Pts',(-0.0773634912799965,-0.0906526488910235,
6.72205346941013E-18));
#36319=CARTESIAN_POINT('Ctrl Pts',(-0.0815539383946836,-0.0878403667988651,
-2.29049000805066E-18));
#36320=CARTESIAN_POINT('Ctrl Pts',(-0.0855414709026766,-0.0847378275400617,
-2.5182094749946E-17));
#36321=CARTESIAN_POINT('Ctrl Pts',(-0.089317923041959,-0.0813786482814292,
-3.31765864780564E-17));
#36322=CARTESIAN_POINT('Ctrl Pts',(-0.0927862368571965,-0.0782935601084891,
-4.05187703807701E-17));
#36323=CARTESIAN_POINT('Ctrl Pts',(-0.0960787339139733,-0.0749884873641515,
4.97114916498215E-19));
#36324=CARTESIAN_POINT('Ctrl Pts',(-0.0991698906024268,-0.0715076841230725,
-8.67361737988404E-19));
#36325=CARTESIAN_POINT('Ctrl Pts',(-0.103663297594998,-0.0664478740909087,
-2.85080986385392E-18));
#36326=CARTESIAN_POINT('Ctrl Pts',(-0.107740134647113,-0.0610110581939007,
-1.51788304147971E-17));
#36327=CARTESIAN_POINT('Ctrl Pts',(-0.111378619976329,-0.0552695407791115,
-1.51788304147971E-17));
#36328=CARTESIAN_POINT('Ctrl Pts',(-0.113566215904755,-0.0518175218802795,
-1.51788304147971E-17));
#36329=CARTESIAN_POINT('Ctrl Pts',(-0.115595886809481,-0.0482525855570875,
-3.79982201238933E-17));
#36330=CARTESIAN_POINT('Ctrl Pts',(-0.117451481229743,-0.0446106777439056,
-3.20923843055709E-17));
#36331=CARTESIAN_POINT('Ctrl Pts',(-0.121759272594108,-0.0361559319998316,
-1.83818944163349E-17));
#36332=CARTESIAN_POINT('Ctrl Pts',(-0.125146870804877,-0.027267170883122,
-1.0758832179559E-17));
#36333=CARTESIAN_POINT('Ctrl Pts',(-0.127551512867323,-0.0181239349359946,
-1.21430643318376E-17));
#36334=CARTESIAN_POINT('Ctrl Pts',(-0.128525246808636,-0.0144214798745123,
-1.27035942545157E-17));
#36335=CARTESIAN_POINT('Ctrl Pts',(-0.129337364222068,-0.0106768832185224,
-3.87407706984377E-19));
#36336=CARTESIAN_POINT('Ctrl Pts',(-0.129981634111732,-0.00690081199580598,
2.60208521396521E-18));
#36337=CARTESIAN_POINT('Ctrl Pts',(-0.130488787940845,-0.00392837915310221,
4.95534245334234E-18));
#36338=CARTESIAN_POINT('Ctrl Pts',(-0.130891436982594,-0.000937368841373321,
-5.77147351242312E-18));
#36339=CARTESIAN_POINT('Ctrl Pts',(-0.131185766414779,0.00205408358364406,
-5.20417042793042E-18));
#36340=CARTESIAN_POINT('Ctrl Pts',(-0.131681056523625,0.00708802390756766,
-4.24952717536476E-18));
#36341=CARTESIAN_POINT('Ctrl Pts',(-0.131871567589099,0.0121324651245783,
-2.3640808795201E-17));
#36342=CARTESIAN_POINT('Ctrl Pts',(-0.131747571113314,0.0171617682916428,
-1.73472347597681E-17));
#36343=CARTESIAN_POINT('Ctrl Pts',(-0.131588224313727,0.0236248823338087,
-9.16854279395534E-18));
#36344=CARTESIAN_POINT('Ctrl Pts',(-0.130910003388584,0.0300630957896326,
1.9164721863282E-18));
#36345=CARTESIAN_POINT('Ctrl Pts',(-0.129749448943416,0.0364359420359482,
1.73472347597681E-18));
#36346=CARTESIAN_POINT('Ctrl Pts',(-0.129188162258574,0.039518084159911,
1.64682313529719E-18));
#36347=CARTESIAN_POINT('Ctrl Pts',(-0.128513877700937,0.0425849598402651,
-2.5119873647686E-17));
#36348=CARTESIAN_POINT('Ctrl Pts',(-0.127729776371406,0.0456319959092621,
-2.60208521396521E-17));
#36349=CARTESIAN_POINT('Ctrl Pts',(-0.126905460209866,0.0488353077541379,
-2.69680398361349E-17));
#36350=CARTESIAN_POINT('Ctrl Pts',(-0.125961589290349,0.0520090496451376,
-6.80234412585701E-18));
#36351=CARTESIAN_POINT('Ctrl Pts',(-0.124905367512152,0.0551421622546814,
-8.67361737988404E-18));
#36352=CARTESIAN_POINT('Ctrl Pts',(-0.122242239861443,0.0630419035736882,
-1.33917927173935E-17));
#36353=CARTESIAN_POINT('Ctrl Pts',(-0.118863777535182,0.0706951392673794,
8.60987302363936E-19));
#36354=CARTESIAN_POINT('Ctrl Pts',(-0.114842094503769,0.0780194918792452,
1.73472347597681E-18));
#36355=CARTESIAN_POINT('Ctrl Pts',(-0.112169428435535,0.0828869935059547,
2.31537714896978E-18));
#36356=CARTESIAN_POINT('Ctrl Pts',(-0.109212095329563,0.0876093199712314,
1.58690079118504E-17));
#36357=CARTESIAN_POINT('Ctrl Pts',(-0.105985186696901,0.0921609434032714,
1.90819582357449E-17));
#36358=CARTESIAN_POINT('Ctrl Pts',(-0.104153982707569,0.0947438956760198,
2.09052411731938E-17));
#36359=CARTESIAN_POINT('Ctrl Pts',(-0.102235981964729,0.0972711925776025,
1.37027400976072E-17));
#36360=CARTESIAN_POINT('Ctrl Pts',(-0.10024275281245,0.0997277902811201,
1.21430643318376E-17));
#36361=CARTESIAN_POINT('Ctrl Pts',(-0.0937332858648147,0.107750521403832,
7.04949150570437E-18));
#36362=CARTESIAN_POINT('Ctrl Pts',(-0.0864043214638765,0.115051138974542,
-2.08047340785725E-18));
#36363=CARTESIAN_POINT('Ctrl Pts',(-0.0783638198438572,0.121477900017692,
0.));
#36364=CARTESIAN_POINT('Ctrl Pts',(-0.0736196559743728,0.125269903176152,
1.22754863308587E-18));
#36365=CARTESIAN_POINT('Ctrl Pts',(-0.0686268317545984,0.128757413629593,
6.34938948147863E-19));
#36366=CARTESIAN_POINT('Ctrl Pts',(-0.0634007094575211,0.131904027763685,
0.));
#36367=CARTESIAN_POINT('Origin',(0.,0.,0.));
#36368=CARTESIAN_POINT('Origin',(-0.0577350269189626,-0.1,-0.3));
#36369=CARTESIAN_POINT('',(-0.0577350269189626,-0.1,-0.3));
#36370=CARTESIAN_POINT('',(0.0577350269189626,-0.1,-0.3));
#36371=CARTESIAN_POINT('',(-0.0288675134594813,-0.1,-0.3));
#36372=CARTESIAN_POINT('',(-0.0577350269189626,-0.1,-0.1));
#36373=CARTESIAN_POINT('',(-0.0577350269189626,-0.1,-0.3));
#36374=CARTESIAN_POINT('',(0.0577350269189626,-0.1,-0.1));
#36375=CARTESIAN_POINT('',(-0.0577350269189626,-0.1,-0.1));
#36376=CARTESIAN_POINT('',(0.0577350269189626,-0.1,-0.3));
#36377=CARTESIAN_POINT('Origin',(-0.115470053837925,1.41410031829988E-17,
-0.3));
#36378=CARTESIAN_POINT('',(-0.115470053837925,1.41410031829988E-17,-0.3));
#36379=CARTESIAN_POINT('',(-0.101036297108185,-0.025,-0.3));
#36380=CARTESIAN_POINT('',(-0.115470053837925,1.38777878078145E-17,-0.1));
#36381=CARTESIAN_POINT('',(-0.115470053837925,1.41410031829988E-17,-0.3));
#36382=CARTESIAN_POINT('',(-0.115470053837925,1.41410031829988E-17,-0.1));
#36383=CARTESIAN_POINT('Origin',(-0.0577350269189626,0.1,-0.3));
#36384=CARTESIAN_POINT('',(-0.0577350269189626,0.1,-0.3));
#36385=CARTESIAN_POINT('',(-0.0721687836487032,0.075,-0.3));
#36386=CARTESIAN_POINT('',(-0.0577350269189626,0.1,-0.1));
#36387=CARTESIAN_POINT('',(-0.0577350269189626,0.1,-0.3));
#36388=CARTESIAN_POINT('',(-0.0577350269189626,0.1,-0.1));
#36389=CARTESIAN_POINT('Origin',(0.0577350269189626,0.1,-0.3));
#36390=CARTESIAN_POINT('',(0.0577350269189626,0.1,-0.3));
#36391=CARTESIAN_POINT('',(0.0288675134594813,0.1,-0.3));
#36392=CARTESIAN_POINT('',(0.0577350269189626,0.1,-0.1));
#36393=CARTESIAN_POINT('',(0.0577350269189626,0.1,-0.3));
#36394=CARTESIAN_POINT('',(0.0577350269189626,0.1,-0.1));
#36395=CARTESIAN_POINT('Origin',(0.115470053837925,0.,-0.3));
#36396=CARTESIAN_POINT('',(0.115470053837925,0.,-0.3));
#36397=CARTESIAN_POINT('',(0.101036297108185,0.025,-0.3));
#36398=CARTESIAN_POINT('',(0.115470053837925,0.,-0.1));
#36399=CARTESIAN_POINT('',(0.115470053837925,0.,-0.3));
#36400=CARTESIAN_POINT('',(0.115470053837925,0.,-0.1));
#36401=CARTESIAN_POINT('Origin',(0.0577350269189626,-0.1,-0.3));
#36402=CARTESIAN_POINT('',(0.0721687836487032,-0.075,-0.3));
#36403=CARTESIAN_POINT('',(0.0577350269189626,-0.1,-0.1));
#36404=CARTESIAN_POINT('Origin',(0.,0.,-0.1));
#36405=CARTESIAN_POINT('Origin',(0.,0.,0.));
#36406=CARTESIAN_POINT('',(-0.3,-3.67394039744206E-17,0.));
#36407=CARTESIAN_POINT('Origin',(0.,0.,0.));
#36408=CARTESIAN_POINT('Origin',(0.,0.,-0.3));
#36409=CARTESIAN_POINT('',(-0.3,-3.67394039744206E-17,-0.3));
#36410=CARTESIAN_POINT('',(-0.3,-3.67394039744206E-17,-0.3));
#36411=CARTESIAN_POINT('Origin',(0.,0.,-0.3));
#36412=CARTESIAN_POINT('Origin',(0.,0.,-0.3));
#36413=CARTESIAN_POINT('Origin',(0.,0.,1.));
#36414=CARTESIAN_POINT('',(0.,0.,0.));
#36415=CARTESIAN_POINT('',(0.,0.,0.));
#36416=CARTESIAN_POINT('',(0.,-2.8,2.2));
#36417=CARTESIAN_POINT('',(0.,0.,0.));
#36418=CARTESIAN_POINT('',(0.,0.,0.));
#36419=CARTESIAN_POINT('',(2.4,1.,0.));
#36420=CARTESIAN_POINT('',(1.4,1.,0.));
#36421=CARTESIAN_POINT('',(1.4,1.,0.));
#36422=CARTESIAN_POINT('',(-0.5,0.,7.8));
#36423=CARTESIAN_POINT('',(-2.4,1.,0.));
#36424=CARTESIAN_POINT('',(-1.4,1.,0.));
#36425=CARTESIAN_POINT('',(-1.4,1.,0.));
#36426=CARTESIAN_POINT('',(-0.5,0.,7.8));
#36427=CARTESIAN_POINT('',(-1.,0.,7.8));
#36428=CARTESIAN_POINT('',(-0.6,0.,7.8));
#36429=CARTESIAN_POINT('',(1.1,0.,7.8));
#36430=CARTESIAN_POINT('',(0.,0.,0.9));
#36431=CARTESIAN_POINT('',(0.5,0.,7.8));
#36432=CARTESIAN_POINT('',(1.,0.,7.8));
#36433=CARTESIAN_POINT('',(-3.6,-2.4,5.8));
#36434=CARTESIAN_POINT('',(-0.6,1.,2.6));
#36435=CARTESIAN_POINT('',(2.4,1.,4.));
#36436=CARTESIAN_POINT('',(-3.6,2.4,5.8));
#36437=CARTESIAN_POINT('',(3.6,-2.4,5.8));
#36438=CARTESIAN_POINT('',(3.6,2.4,5.8));
#36439=CARTESIAN_POINT('',(-2.4,1.,0.4));
#36440=CARTESIAN_POINT('',(2.4,1.,0.4));
#36441=CARTESIAN_POINT('',(0.6,1.,2.6));
#36442=CARTESIAN_POINT('',(-1.4,1.,4.2));
#36443=CARTESIAN_POINT('',(1.4,1.,4.2));
#36444=CARTESIAN_POINT('',(-2.4,1.,4.));
#36445=UNCERTAINTY_MEASURE_WITH_UNIT(LENGTH_MEASURE(0.001),#36483,
'DISTANCE_ACCURACY_VALUE',
'Maximum model space distance between geometric entities at asserted c
onnectivities');
#36446=UNCERTAINTY_MEASURE_WITH_UNIT(LENGTH_MEASURE(0.001),#36483,
'DISTANCE_ACCURACY_VALUE',
'Maximum model space distance between geometric entities at asserted c
onnectivities');
#36447=UNCERTAINTY_MEASURE_WITH_UNIT(LENGTH_MEASURE(0.001),#36483,
'DISTANCE_ACCURACY_VALUE',
'Maximum model space distance between geometric entities at asserted c
onnectivities');
#36448=UNCERTAINTY_MEASURE_WITH_UNIT(LENGTH_MEASURE(0.001),#36483,
'DISTANCE_ACCURACY_VALUE',
'Maximum model space distance between geometric entities at asserted c
onnectivities');
#36449=UNCERTAINTY_MEASURE_WITH_UNIT(LENGTH_MEASURE(0.001),#36483,
'DISTANCE_ACCURACY_VALUE',
'Maximum model space distance between geometric entities at asserted c
onnectivities');
#36450=UNCERTAINTY_MEASURE_WITH_UNIT(LENGTH_MEASURE(0.001),#36483,
'DISTANCE_ACCURACY_VALUE',
'Maximum model space distance between geometric entities at asserted c
onnectivities');
#36451=UNCERTAINTY_MEASURE_WITH_UNIT(LENGTH_MEASURE(0.001),#36483,
'DISTANCE_ACCURACY_VALUE',
'Maximum model space distance between geometric entities at asserted c
onnectivities');
#36452=UNCERTAINTY_MEASURE_WITH_UNIT(LENGTH_MEASURE(0.001),#36483,
'DISTANCE_ACCURACY_VALUE',
'Maximum model space distance between geometric entities at asserted c
onnectivities');
#36453=UNCERTAINTY_MEASURE_WITH_UNIT(LENGTH_MEASURE(0.001),#36483,
'DISTANCE_ACCURACY_VALUE',
'Maximum model space distance between geometric entities at asserted c
onnectivities');
#36454=UNCERTAINTY_MEASURE_WITH_UNIT(LENGTH_MEASURE(0.001),#36483,
'DISTANCE_ACCURACY_VALUE',
'Maximum model space distance between geometric entities at asserted c
onnectivities');
#36455=UNCERTAINTY_MEASURE_WITH_UNIT(LENGTH_MEASURE(0.001),#36483,
'DISTANCE_ACCURACY_VALUE',
'Maximum model space distance between geometric entities at asserted c
onnectivities');
#36456=UNCERTAINTY_MEASURE_WITH_UNIT(LENGTH_MEASURE(0.001),#36483,
'DISTANCE_ACCURACY_VALUE',
'Maximum model space distance between geometric entities at asserted c
onnectivities');
#36457=UNCERTAINTY_MEASURE_WITH_UNIT(LENGTH_MEASURE(0.001),#36483,
'DISTANCE_ACCURACY_VALUE',
'Maximum model space distance between geometric entities at asserted c
onnectivities');
#36458=UNCERTAINTY_MEASURE_WITH_UNIT(LENGTH_MEASURE(0.001),#36483,
'DISTANCE_ACCURACY_VALUE',
'Maximum model space distance between geometric entities at asserted c
onnectivities');
#36459=UNCERTAINTY_MEASURE_WITH_UNIT(LENGTH_MEASURE(0.001),#36483,
'DISTANCE_ACCURACY_VALUE',
'Maximum model space distance between geometric entities at asserted c
onnectivities');
#36460=UNCERTAINTY_MEASURE_WITH_UNIT(LENGTH_MEASURE(0.001),#36483,
'DISTANCE_ACCURACY_VALUE',
'Maximum model space distance between geometric entities at asserted c
onnectivities');
#36461=UNCERTAINTY_MEASURE_WITH_UNIT(LENGTH_MEASURE(0.001),#36483,
'DISTANCE_ACCURACY_VALUE',
'Maximum model space distance between geometric entities at asserted c
onnectivities');
#36462=UNCERTAINTY_MEASURE_WITH_UNIT(LENGTH_MEASURE(0.001),#36483,
'DISTANCE_ACCURACY_VALUE',
'Maximum model space distance between geometric entities at asserted c
onnectivities');
#36463=UNCERTAINTY_MEASURE_WITH_UNIT(LENGTH_MEASURE(0.001),#36483,
'DISTANCE_ACCURACY_VALUE',
'Maximum model space distance between geometric entities at asserted c
onnectivities');
#36464=(
GEOMETRIC_REPRESENTATION_CONTEXT(3)
GLOBAL_UNCERTAINTY_ASSIGNED_CONTEXT((#36445))
GLOBAL_UNIT_ASSIGNED_CONTEXT((#36483,#36485,#36486))
REPRESENTATION_CONTEXT('','3D')
);
#36465=(
GEOMETRIC_REPRESENTATION_CONTEXT(3)
GLOBAL_UNCERTAINTY_ASSIGNED_CONTEXT((#36446))
GLOBAL_UNIT_ASSIGNED_CONTEXT((#36483,#36485,#36486))
REPRESENTATION_CONTEXT('','3D')
);
#36466=(
GEOMETRIC_REPRESENTATION_CONTEXT(3)
GLOBAL_UNCERTAINTY_ASSIGNED_CONTEXT((#36447))
GLOBAL_UNIT_ASSIGNED_CONTEXT((#36483,#36485,#36486))
REPRESENTATION_CONTEXT('','3D')
);
#36467=(
GEOMETRIC_REPRESENTATION_CONTEXT(3)
GLOBAL_UNCERTAINTY_ASSIGNED_CONTEXT((#36448))
GLOBAL_UNIT_ASSIGNED_CONTEXT((#36483,#36485,#36486))
REPRESENTATION_CONTEXT('','3D')
);
#36468=(
GEOMETRIC_REPRESENTATION_CONTEXT(3)
GLOBAL_UNCERTAINTY_ASSIGNED_CONTEXT((#36449))
GLOBAL_UNIT_ASSIGNED_CONTEXT((#36483,#36485,#36486))
REPRESENTATION_CONTEXT('','3D')
);
#36469=(
GEOMETRIC_REPRESENTATION_CONTEXT(3)
GLOBAL_UNCERTAINTY_ASSIGNED_CONTEXT((#36450))
GLOBAL_UNIT_ASSIGNED_CONTEXT((#36483,#36485,#36486))
REPRESENTATION_CONTEXT('','3D')
);
#36470=(
GEOMETRIC_REPRESENTATION_CONTEXT(3)
GLOBAL_UNCERTAINTY_ASSIGNED_CONTEXT((#36451))
GLOBAL_UNIT_ASSIGNED_CONTEXT((#36483,#36485,#36486))
REPRESENTATION_CONTEXT('','3D')
);
#36471=(
GEOMETRIC_REPRESENTATION_CONTEXT(3)
GLOBAL_UNCERTAINTY_ASSIGNED_CONTEXT((#36452))
GLOBAL_UNIT_ASSIGNED_CONTEXT((#36483,#36485,#36486))
REPRESENTATION_CONTEXT('','3D')
);
#36472=(
GEOMETRIC_REPRESENTATION_CONTEXT(3)
GLOBAL_UNCERTAINTY_ASSIGNED_CONTEXT((#36453))
GLOBAL_UNIT_ASSIGNED_CONTEXT((#36483,#36485,#36486))
REPRESENTATION_CONTEXT('','3D')
);
#36473=(
GEOMETRIC_REPRESENTATION_CONTEXT(3)
GLOBAL_UNCERTAINTY_ASSIGNED_CONTEXT((#36454))
GLOBAL_UNIT_ASSIGNED_CONTEXT((#36483,#36485,#36486))
REPRESENTATION_CONTEXT('','3D')
);
#36474=(
GEOMETRIC_REPRESENTATION_CONTEXT(3)
GLOBAL_UNCERTAINTY_ASSIGNED_CONTEXT((#36455))
GLOBAL_UNIT_ASSIGNED_CONTEXT((#36483,#36485,#36486))
REPRESENTATION_CONTEXT('','3D')
);
#36475=(
GEOMETRIC_REPRESENTATION_CONTEXT(3)
GLOBAL_UNCERTAINTY_ASSIGNED_CONTEXT((#36456))
GLOBAL_UNIT_ASSIGNED_CONTEXT((#36483,#36485,#36486))
REPRESENTATION_CONTEXT('','3D')
);
#36476=(
GEOMETRIC_REPRESENTATION_CONTEXT(3)
GLOBAL_UNCERTAINTY_ASSIGNED_CONTEXT((#36457))
GLOBAL_UNIT_ASSIGNED_CONTEXT((#36483,#36485,#36486))
REPRESENTATION_CONTEXT('','3D')
);
#36477=(
GEOMETRIC_REPRESENTATION_CONTEXT(3)
GLOBAL_UNCERTAINTY_ASSIGNED_CONTEXT((#36458))
GLOBAL_UNIT_ASSIGNED_CONTEXT((#36483,#36485,#36486))
REPRESENTATION_CONTEXT('','3D')
);
#36478=(
GEOMETRIC_REPRESENTATION_CONTEXT(3)
GLOBAL_UNCERTAINTY_ASSIGNED_CONTEXT((#36459))
GLOBAL_UNIT_ASSIGNED_CONTEXT((#36483,#36485,#36486))
REPRESENTATION_CONTEXT('','3D')
);
#36479=(
GEOMETRIC_REPRESENTATION_CONTEXT(3)
GLOBAL_UNCERTAINTY_ASSIGNED_CONTEXT((#36460))
GLOBAL_UNIT_ASSIGNED_CONTEXT((#36483,#36485,#36486))
REPRESENTATION_CONTEXT('','3D')
);
#36480=(
GEOMETRIC_REPRESENTATION_CONTEXT(3)
GLOBAL_UNCERTAINTY_ASSIGNED_CONTEXT((#36461))
GLOBAL_UNIT_ASSIGNED_CONTEXT((#36483,#36485,#36486))
REPRESENTATION_CONTEXT('','3D')
);
#36481=(
GEOMETRIC_REPRESENTATION_CONTEXT(3)
GLOBAL_UNCERTAINTY_ASSIGNED_CONTEXT((#36462))
GLOBAL_UNIT_ASSIGNED_CONTEXT((#36483,#36485,#36486))
REPRESENTATION_CONTEXT('','3D')
);
#36482=(
GEOMETRIC_REPRESENTATION_CONTEXT(3)
GLOBAL_UNCERTAINTY_ASSIGNED_CONTEXT((#36463))
GLOBAL_UNIT_ASSIGNED_CONTEXT((#36483,#36485,#36486))
REPRESENTATION_CONTEXT('','3D')
);
#36483=(
LENGTH_UNIT()
NAMED_UNIT(*)
SI_UNIT(.CENTI.,.METRE.)
);
#36484=(
LENGTH_UNIT()
NAMED_UNIT(*)
SI_UNIT($,.METRE.)
);
#36485=(
NAMED_UNIT(*)
PLANE_ANGLE_UNIT()
SI_UNIT($,.RADIAN.)
);
#36486=(
NAMED_UNIT(*)
SI_UNIT($,.STERADIAN.)
SOLID_ANGLE_UNIT()
);
#36487=SHAPE_DEFINITION_REPRESENTATION(#36505,#36554);
#36488=SHAPE_DEFINITION_REPRESENTATION(#36506,#36555);
#36489=SHAPE_DEFINITION_REPRESENTATION(#36507,#36556);
#36490=SHAPE_DEFINITION_REPRESENTATION(#36508,#36557);
#36491=SHAPE_DEFINITION_REPRESENTATION(#36509,#36558);
#36492=SHAPE_DEFINITION_REPRESENTATION(#36510,#36559);
#36493=SHAPE_DEFINITION_REPRESENTATION(#36511,#36560);
#36494=SHAPE_DEFINITION_REPRESENTATION(#36512,#36561);
#36495=SHAPE_DEFINITION_REPRESENTATION(#36513,#36562);
#36496=SHAPE_DEFINITION_REPRESENTATION(#36514,#36563);
#36497=SHAPE_DEFINITION_REPRESENTATION(#36515,#36564);
#36498=SHAPE_DEFINITION_REPRESENTATION(#36516,#36565);
#36499=SHAPE_DEFINITION_REPRESENTATION(#36517,#36566);
#36500=SHAPE_DEFINITION_REPRESENTATION(#36518,#36567);
#36501=SHAPE_DEFINITION_REPRESENTATION(#36519,#36568);
#36502=SHAPE_DEFINITION_REPRESENTATION(#36520,#36569);
#36503=SHAPE_DEFINITION_REPRESENTATION(#36521,#36570);
#36504=SHAPE_DEFINITION_REPRESENTATION(#36522,#36571);
#36505=PRODUCT_DEFINITION_SHAPE('',$,#36573);
#36506=PRODUCT_DEFINITION_SHAPE('',$,#36574);
#36507=PRODUCT_DEFINITION_SHAPE('',$,#36575);
#36508=PRODUCT_DEFINITION_SHAPE('',$,#36576);
#36509=PRODUCT_DEFINITION_SHAPE('',$,#36577);
#36510=PRODUCT_DEFINITION_SHAPE('',$,#36578);
#36511=PRODUCT_DEFINITION_SHAPE('',$,#36579);
#36512=PRODUCT_DEFINITION_SHAPE('',$,#36580);
#36513=PRODUCT_DEFINITION_SHAPE('',$,#36581);
#36514=PRODUCT_DEFINITION_SHAPE('',$,#36582);
#36515=PRODUCT_DEFINITION_SHAPE('',$,#36583);
#36516=PRODUCT_DEFINITION_SHAPE('',$,#36584);
#36517=PRODUCT_DEFINITION_SHAPE('',$,#36585);
#36518=PRODUCT_DEFINITION_SHAPE('',$,#36586);
#36519=PRODUCT_DEFINITION_SHAPE('',$,#36587);
#36520=PRODUCT_DEFINITION_SHAPE('',$,#36588);
#36521=PRODUCT_DEFINITION_SHAPE('',$,#36589);
#36522=PRODUCT_DEFINITION_SHAPE('',$,#36590);
#36523=PRODUCT_DEFINITION_SHAPE($,$,#104);
#36524=PRODUCT_DEFINITION_SHAPE($,$,#105);
#36525=PRODUCT_DEFINITION_SHAPE($,$,#106);
#36526=PRODUCT_DEFINITION_SHAPE($,$,#107);
#36527=PRODUCT_DEFINITION_SHAPE($,$,#108);
#36528=PRODUCT_DEFINITION_SHAPE($,$,#109);
#36529=PRODUCT_DEFINITION_SHAPE($,$,#110);
#36530=PRODUCT_DEFINITION_SHAPE($,$,#111);
#36531=PRODUCT_DEFINITION_SHAPE($,$,#112);
#36532=PRODUCT_DEFINITION_SHAPE($,$,#113);
#36533=PRODUCT_DEFINITION_SHAPE($,$,#114);
#36534=PRODUCT_DEFINITION_SHAPE($,$,#115);
#36535=PRODUCT_DEFINITION_SHAPE($,$,#116);
#36536=PRODUCT_DEFINITION_SHAPE($,$,#117);
#36537=PRODUCT_DEFINITION_SHAPE($,$,#118);
#36538=PRODUCT_DEFINITION_SHAPE($,$,#119);
#36539=PRODUCT_DEFINITION_SHAPE($,$,#120);
#36540=PRODUCT_DEFINITION_SHAPE($,$,#121);
#36541=PRODUCT_DEFINITION_SHAPE($,$,#122);
#36542=PRODUCT_DEFINITION_SHAPE($,$,#123);
#36543=PRODUCT_DEFINITION_SHAPE($,$,#124);
#36544=PRODUCT_DEFINITION_SHAPE($,$,#125);
#36545=PRODUCT_DEFINITION_SHAPE($,$,#126);
#36546=PRODUCT_DEFINITION_SHAPE($,$,#127);
#36547=PRODUCT_DEFINITION_SHAPE($,$,#128);
#36548=PRODUCT_DEFINITION_SHAPE($,$,#129);
#36549=PRODUCT_DEFINITION_SHAPE($,$,#130);
#36550=PRODUCT_DEFINITION_SHAPE($,$,#131);
#36551=PRODUCT_DEFINITION_SHAPE($,$,#132);
#36552=PRODUCT_DEFINITION_SHAPE($,$,#133);
#36553=PRODUCT_DEFINITION_SHAPE($,$,#134);
#36554=SHAPE_REPRESENTATION('',(#9972,#10659,#10660,#10661,#10662,#10663,
#10664,#10665,#10666,#10667,#10668,#10669,#10670,#10671,#10672,#10673,#10674,
#10675,#10676,#10677,#10678,#10679,#10680,#10681,#10682,#10683,#10684,#10685,
#10686,#10687,#10688,#10689),#36464);
#36555=SHAPE_REPRESENTATION('',(#9973),#36465);
#36556=SHAPE_REPRESENTATION('',(#10172),#36466);
#36557=SHAPE_REPRESENTATION('',(#10194),#36467);
#36558=SHAPE_REPRESENTATION('',(#10207),#36468);
#36559=SHAPE_REPRESENTATION('',(#10284),#36469);
#36560=SHAPE_REPRESENTATION('',(#10297),#36470);
#36561=SHAPE_REPRESENTATION('',(#10314),#36471);
#36562=SHAPE_REPRESENTATION('',(#10401),#36472);
#36563=SHAPE_REPRESENTATION('',(#10443),#36473);
#36564=SHAPE_REPRESENTATION('',(#10453),#36474);
#36565=SHAPE_REPRESENTATION('',(#10462),#36475);
#36566=SHAPE_REPRESENTATION('',(#10480),#36476);
#36567=SHAPE_REPRESENTATION('',(#10491),#36477);
#36568=SHAPE_REPRESENTATION('',(#10496),#36478);
#36569=SHAPE_REPRESENTATION('',(#10505),#36479);
#36570=SHAPE_REPRESENTATION('',(#10559),#36480);
#36571=SHAPE_REPRESENTATION('',(#10601),#36481);
#36572=PRODUCT_DEFINITION_CONTEXT('part definition',#36628,'design');
#36573=PRODUCT_DEFINITION('MAS-651','MAS-651',#36591,#36572);
#36574=PRODUCT_DEFINITION('Switch housing','Switch housing',#36592,#36572);
#36575=PRODUCT_DEFINITION('Housing cover','Housing cover',#36593,#36572);
#36576=PRODUCT_DEFINITION('Cable entry seal','Cable entry seal',#36594,
#36572);
#36577=PRODUCT_DEFINITION('Roller actuator','Roller actuator',#36595,#36572);
#36578=PRODUCT_DEFINITION('Moving contact bridge',
'Moving contact bridge',#36596,#36572);
#36579=PRODUCT_DEFINITION('Actuating roller','Actuating roller',#36597,
#36572);
#36580=PRODUCT_DEFINITION('Terminal insulator','Terminal insulator',#36598,
#36572);
#36581=PRODUCT_DEFINITION('Fixed contact terminal',
'Fixed contact terminal',#36599,#36572);
#36582=PRODUCT_DEFINITION('Terminal clamp plate','Terminal clamp plate',
#36600,#36572);
#36583=PRODUCT_DEFINITION('Roller bushing','Roller bushing',#36601,#36572);
#36584=PRODUCT_DEFINITION('Roller pin','Roller pin',#36602,#36572);
#36585=PRODUCT_DEFINITION('Roller retaining ring',
'Roller retaining ring',#36603,#36572);
#36586=PRODUCT_DEFINITION('Compression spring','Compression spring',#36604,
#36572);
#36587=PRODUCT_DEFINITION('Roller thrust washer','Roller thrust washer',
#36605,#36572);
#36588=PRODUCT_DEFINITION('Socket head cap screw M4x12',
'Socket head cap screw M4x12',#36606,#36572);
#36589=PRODUCT_DEFINITION('Socket head cap screw M3x6',
'Socket head cap screw M3x6',#36607,#36572);
#36590=PRODUCT_DEFINITION('Socket head cap screw M3x10',
'Socket head cap screw M3x10',#36608,#36572);
#36591=PRODUCT_DEFINITION_FORMATION('',$,#36630);
#36592=PRODUCT_DEFINITION_FORMATION('',$,#36631);
#36593=PRODUCT_DEFINITION_FORMATION('',$,#36632);
#36594=PRODUCT_DEFINITION_FORMATION('',$,#36633);
#36595=PRODUCT_DEFINITION_FORMATION('',$,#36634);
#36596=PRODUCT_DEFINITION_FORMATION('',$,#36635);
#36597=PRODUCT_DEFINITION_FORMATION('',$,#36636);
#36598=PRODUCT_DEFINITION_FORMATION('',$,#36637);
#36599=PRODUCT_DEFINITION_FORMATION('',$,#36638);
#36600=PRODUCT_DEFINITION_FORMATION('',$,#36639);
#36601=PRODUCT_DEFINITION_FORMATION('',$,#36640);
#36602=PRODUCT_DEFINITION_FORMATION('',$,#36641);
#36603=PRODUCT_DEFINITION_FORMATION('',$,#36642);
#36604=PRODUCT_DEFINITION_FORMATION('',$,#36643);
#36605=PRODUCT_DEFINITION_FORMATION('',$,#36644);
#36606=PRODUCT_DEFINITION_FORMATION('',$,#36645);
#36607=PRODUCT_DEFINITION_FORMATION('',$,#36646);
#36608=PRODUCT_DEFINITION_FORMATION('',$,#36647);
#36609=PRODUCT_RELATED_PRODUCT_CATEGORY('MAS-651','MAS-651',(#36630));
#36610=PRODUCT_RELATED_PRODUCT_CATEGORY('Switch housing',
'Switch housing',(#36631));
#36611=PRODUCT_RELATED_PRODUCT_CATEGORY('Housing cover','Housing cover',
(#36632));
#36612=PRODUCT_RELATED_PRODUCT_CATEGORY('Cable entry seal',
'Cable entry seal',(#36633));
#36613=PRODUCT_RELATED_PRODUCT_CATEGORY('Roller actuator',
'Roller actuator',(#36634));
#36614=PRODUCT_RELATED_PRODUCT_CATEGORY('Moving contact bridge',
'Moving contact bridge',(#36635));
#36615=PRODUCT_RELATED_PRODUCT_CATEGORY('Actuating roller',
'Actuating roller',(#36636));
#36616=PRODUCT_RELATED_PRODUCT_CATEGORY('Terminal insulator',
'Terminal insulator',(#36637));
#36617=PRODUCT_RELATED_PRODUCT_CATEGORY('Fixed contact terminal',
'Fixed contact terminal',(#36638));
#36618=PRODUCT_RELATED_PRODUCT_CATEGORY('Terminal clamp plate',
'Terminal clamp plate',(#36639));
#36619=PRODUCT_RELATED_PRODUCT_CATEGORY('Roller bushing',
'Roller bushing',(#36640));
#36620=PRODUCT_RELATED_PRODUCT_CATEGORY('Roller pin','Roller pin',(#36641));
#36621=PRODUCT_RELATED_PRODUCT_CATEGORY('Roller retaining ring',
'Roller retaining ring',(#36642));
#36622=PRODUCT_RELATED_PRODUCT_CATEGORY('Compression spring',
'Compression spring',(#36643));
#36623=PRODUCT_RELATED_PRODUCT_CATEGORY('Roller thrust washer',
'Roller thrust washer',(#36644));
#36624=PRODUCT_RELATED_PRODUCT_CATEGORY('Socket head cap screw M4x12',
'Socket head cap screw M4x12',(#36645));
#36625=PRODUCT_RELATED_PRODUCT_CATEGORY('Socket head cap screw M3x6',
'Socket head cap screw M3x6',(#36646));
#36626=PRODUCT_RELATED_PRODUCT_CATEGORY('Socket head cap screw M3x10',
'Socket head cap screw M3x10',(#36647));
#36627=APPLICATION_PROTOCOL_DEFINITION('international standard',
'automotive_design',2009,#36628);
#36628=APPLICATION_CONTEXT(
'Core Data for Automotive Mechanical Design Process');
#36629=PRODUCT_CONTEXT('part definition',#36628,'mechanical');
#36630=PRODUCT('MAS-651','MAS-651',
'Independent direct-acting normally-closed roller-plunger limit-switch
 CAD. Removable cover, insulated terminal supports, captured bus/conta
ct bridge, native Coil return spring, integral lower travel stop, reus
able instanced hardware and free roller. Manual geometric contact open
ing4mm; no snap-action/contact-force, electrical/current/voltage, envi
ronmental seal, safety-switch, wear, load or life certification. Exter
nal wiring and anchors omitted; fits and application engineering requi
red.',(#36629));
#36631=PRODUCT('Switch housing','Switch housing',$,(#36629));
#36632=PRODUCT('Housing cover','Housing cover',$,(#36629));
#36633=PRODUCT('Cable entry seal','Cable entry seal',$,(#36629));
#36634=PRODUCT('Roller actuator','Roller actuator',$,(#36629));
#36635=PRODUCT('Moving contact bridge','Moving contact bridge',$,(#36629));
#36636=PRODUCT('Actuating roller','Actuating roller',
'Turn concentric OD and bore, face and chamfer. Nominal dimensions in 
mm. Fit limits to be assigned at assembly level.',(#36629));
#36637=PRODUCT('Terminal insulator','Terminal insulator',$,(#36629));
#36638=PRODUCT('Fixed contact terminal','Fixed contact terminal',$,(#36629));
#36639=PRODUCT('Terminal clamp plate','Terminal clamp plate',$,(#36629));
#36640=PRODUCT('Roller bushing','Roller bushing',$,(#36629));
#36641=PRODUCT('Roller pin','Roller pin',$,(#36629));
#36642=PRODUCT('Roller retaining ring','Roller retaining ring',$,(#36629));
#36643=PRODUCT('Compression spring','Compression spring',
'Reusable native Coil compression spring created and edited through Fu
sion UI. Mean diameter6mm, round wire1mm,2turns, overall free height5m
m; plain open ends. Axis+Y, initial wire centerY0, physical boundsY\X2\2212\X0\0.
5..4.5mm. Native parameters retain wire section when configuring worki
ng height4mm. No nonuniform body scaling or Boolean construction. Mate
rial temper, seats, stiffness, preload, buckling, fatigue and life not
 rated.',(#36629));
#36644=PRODUCT('Roller thrust washer','Roller thrust washer',$,(#36629));
#36645=PRODUCT('Socket head cap screw M4x12',
'Socket head cap screw M4x12',$,(#36629));
#36646=PRODUCT('Socket head cap screw M3x6',
'Socket head cap screw M3x6',$,(#36629));
#36647=PRODUCT('Socket head cap screw M3x10',
'Socket head cap screw M3x10',$,(#36629));
#36648=PRESENTATION_STYLE_ASSIGNMENT((#36662));
#36649=PRESENTATION_STYLE_ASSIGNMENT((#36663));
#36650=PRESENTATION_STYLE_ASSIGNMENT((#36664));
#36651=PRESENTATION_STYLE_ASSIGNMENT((#36665));
#36652=PRESENTATION_STYLE_ASSIGNMENT((#36666));
#36653=PRESENTATION_STYLE_ASSIGNMENT((#36667));
#36654=PRESENTATION_STYLE_ASSIGNMENT((#36668));
#36655=PRESENTATION_STYLE_ASSIGNMENT((#36669));
#36656=PRESENTATION_STYLE_ASSIGNMENT((#36670));
#36657=PRESENTATION_STYLE_ASSIGNMENT((#36671));
#36658=PRESENTATION_STYLE_ASSIGNMENT((#36672));
#36659=PRESENTATION_STYLE_ASSIGNMENT((#36673));
#36660=PRESENTATION_STYLE_ASSIGNMENT((#36674));
#36661=PRESENTATION_STYLE_ASSIGNMENT((#36675));
#36662=SURFACE_STYLE_USAGE(.BOTH.,#36676);
#36663=SURFACE_STYLE_USAGE(.BOTH.,#36677);
#36664=SURFACE_STYLE_USAGE(.BOTH.,#36678);
#36665=SURFACE_STYLE_USAGE(.BOTH.,#36679);
#36666=SURFACE_STYLE_USAGE(.BOTH.,#36680);
#36667=SURFACE_STYLE_USAGE(.BOTH.,#36681);
#36668=SURFACE_STYLE_USAGE(.BOTH.,#36682);
#36669=SURFACE_STYLE_USAGE(.BOTH.,#36683);
#36670=SURFACE_STYLE_USAGE(.BOTH.,#36684);
#36671=SURFACE_STYLE_USAGE(.BOTH.,#36685);
#36672=SURFACE_STYLE_USAGE(.BOTH.,#36686);
#36673=SURFACE_STYLE_USAGE(.BOTH.,#36687);
#36674=SURFACE_STYLE_USAGE(.BOTH.,#36688);
#36675=SURFACE_STYLE_USAGE(.BOTH.,#36689);
#36676=SURFACE_SIDE_STYLE('',(#36690));
#36677=SURFACE_SIDE_STYLE('',(#36691));
#36678=SURFACE_SIDE_STYLE('',(#36692));
#36679=SURFACE_SIDE_STYLE('',(#36693));
#36680=SURFACE_SIDE_STYLE('',(#36694));
#36681=SURFACE_SIDE_STYLE('',(#36695));
#36682=SURFACE_SIDE_STYLE('',(#36696));
#36683=SURFACE_SIDE_STYLE('',(#36697));
#36684=SURFACE_SIDE_STYLE('',(#36698));
#36685=SURFACE_SIDE_STYLE('',(#36699));
#36686=SURFACE_SIDE_STYLE('',(#36700));
#36687=SURFACE_SIDE_STYLE('',(#36701));
#36688=SURFACE_SIDE_STYLE('',(#36702));
#36689=SURFACE_SIDE_STYLE('',(#36703));
#36690=SURFACE_STYLE_FILL_AREA(#36704);
#36691=SURFACE_STYLE_FILL_AREA(#36705);
#36692=SURFACE_STYLE_FILL_AREA(#36706);
#36693=SURFACE_STYLE_FILL_AREA(#36707);
#36694=SURFACE_STYLE_FILL_AREA(#36708);
#36695=SURFACE_STYLE_FILL_AREA(#36709);
#36696=SURFACE_STYLE_FILL_AREA(#36710);
#36697=SURFACE_STYLE_FILL_AREA(#36711);
#36698=SURFACE_STYLE_FILL_AREA(#36712);
#36699=SURFACE_STYLE_FILL_AREA(#36713);
#36700=SURFACE_STYLE_FILL_AREA(#36714);
#36701=SURFACE_STYLE_FILL_AREA(#36715);
#36702=SURFACE_STYLE_FILL_AREA(#36716);
#36703=SURFACE_STYLE_FILL_AREA(#36717);
#36704=FILL_AREA_STYLE('Steel - Satin',(#36718));
#36705=FILL_AREA_STYLE('Dark blue',(#36719));
#36706=FILL_AREA_STYLE('Sky blue',(#36720));
#36707=FILL_AREA_STYLE('Charcoal',(#36721));
#36708=FILL_AREA_STYLE('Light blue',(#36722));
#36709=FILL_AREA_STYLE('Contact gray',(#36723));
#36710=FILL_AREA_STYLE('Roller gray',(#36724));
#36711=FILL_AREA_STYLE('Insulator gray',(#36725));
#36712=FILL_AREA_STYLE('Clamp gray',(#36726));
#36713=FILL_AREA_STYLE('Bearing gray',(#36727));
#36714=FILL_AREA_STYLE('Pin gray',(#36728));
#36715=FILL_AREA_STYLE('Dark gray',(#36729));
#36716=FILL_AREA_STYLE('Spring gray',(#36730));
#36717=FILL_AREA_STYLE('Washer gray',(#36731));
#36718=FILL_AREA_STYLE_COLOUR('Steel - Satin',#36732);
#36719=FILL_AREA_STYLE_COLOUR('Dark blue',#36733);
#36720=FILL_AREA_STYLE_COLOUR('Sky blue',#36734);
#36721=FILL_AREA_STYLE_COLOUR('Charcoal',#36735);
#36722=FILL_AREA_STYLE_COLOUR('Light blue',#36736);
#36723=FILL_AREA_STYLE_COLOUR('Contact gray',#36737);
#36724=FILL_AREA_STYLE_COLOUR('Roller gray',#36738);
#36725=FILL_AREA_STYLE_COLOUR('Insulator gray',#36739);
#36726=FILL_AREA_STYLE_COLOUR('Clamp gray',#36740);
#36727=FILL_AREA_STYLE_COLOUR('Bearing gray',#36741);
#36728=FILL_AREA_STYLE_COLOUR('Pin gray',#36742);
#36729=FILL_AREA_STYLE_COLOUR('Dark gray',#36743);
#36730=FILL_AREA_STYLE_COLOUR('Spring gray',#36744);
#36731=FILL_AREA_STYLE_COLOUR('Washer gray',#36745);
#36732=COLOUR_RGB('Steel - Satin',0.627450980392157,0.627450980392157,0.627450980392157);
#36733=COLOUR_RGB('Dark blue',0.0901960784313725,0.270588235294118,0.513725490196078);
#36734=COLOUR_RGB('Sky blue',0.317647058823529,0.686274509803922,0.890196078431372);
#36735=COLOUR_RGB('Charcoal',0.164705882352941,0.184313725490196,0.211764705882353);
#36736=COLOUR_RGB('Light blue',0.662745098039216,0.831372549019608,0.949019607843137);
#36737=COLOUR_RGB('Contact gray',0.725490196078431,0.752941176470588,0.792156862745098);
#36738=COLOUR_RGB('Roller gray',0.407843137254902,0.447058823529412,0.498039215686275);
#36739=COLOUR_RGB('Insulator gray',0.576470588235294,0.615686274509804,
0.666666666666667);
#36740=COLOUR_RGB('Clamp gray',0.407843137254902,0.447058823529412,0.498039215686275);
#36741=COLOUR_RGB('Bearing gray',0.725490196078431,0.752941176470588,0.792156862745098);
#36742=COLOUR_RGB('Pin gray',0.576470588235294,0.615686274509804,0.666666666666667);
#36743=COLOUR_RGB('Dark gray',0.250980392156863,0.282352941176471,0.32156862745098);
#36744=COLOUR_RGB('Spring gray',0.407843137254902,0.447058823529412,0.498039215686275);
#36745=COLOUR_RGB('Washer gray',0.725490196078431,0.752941176470588,0.792156862745098);
ENDSEC;
END-ISO-10303-21;
